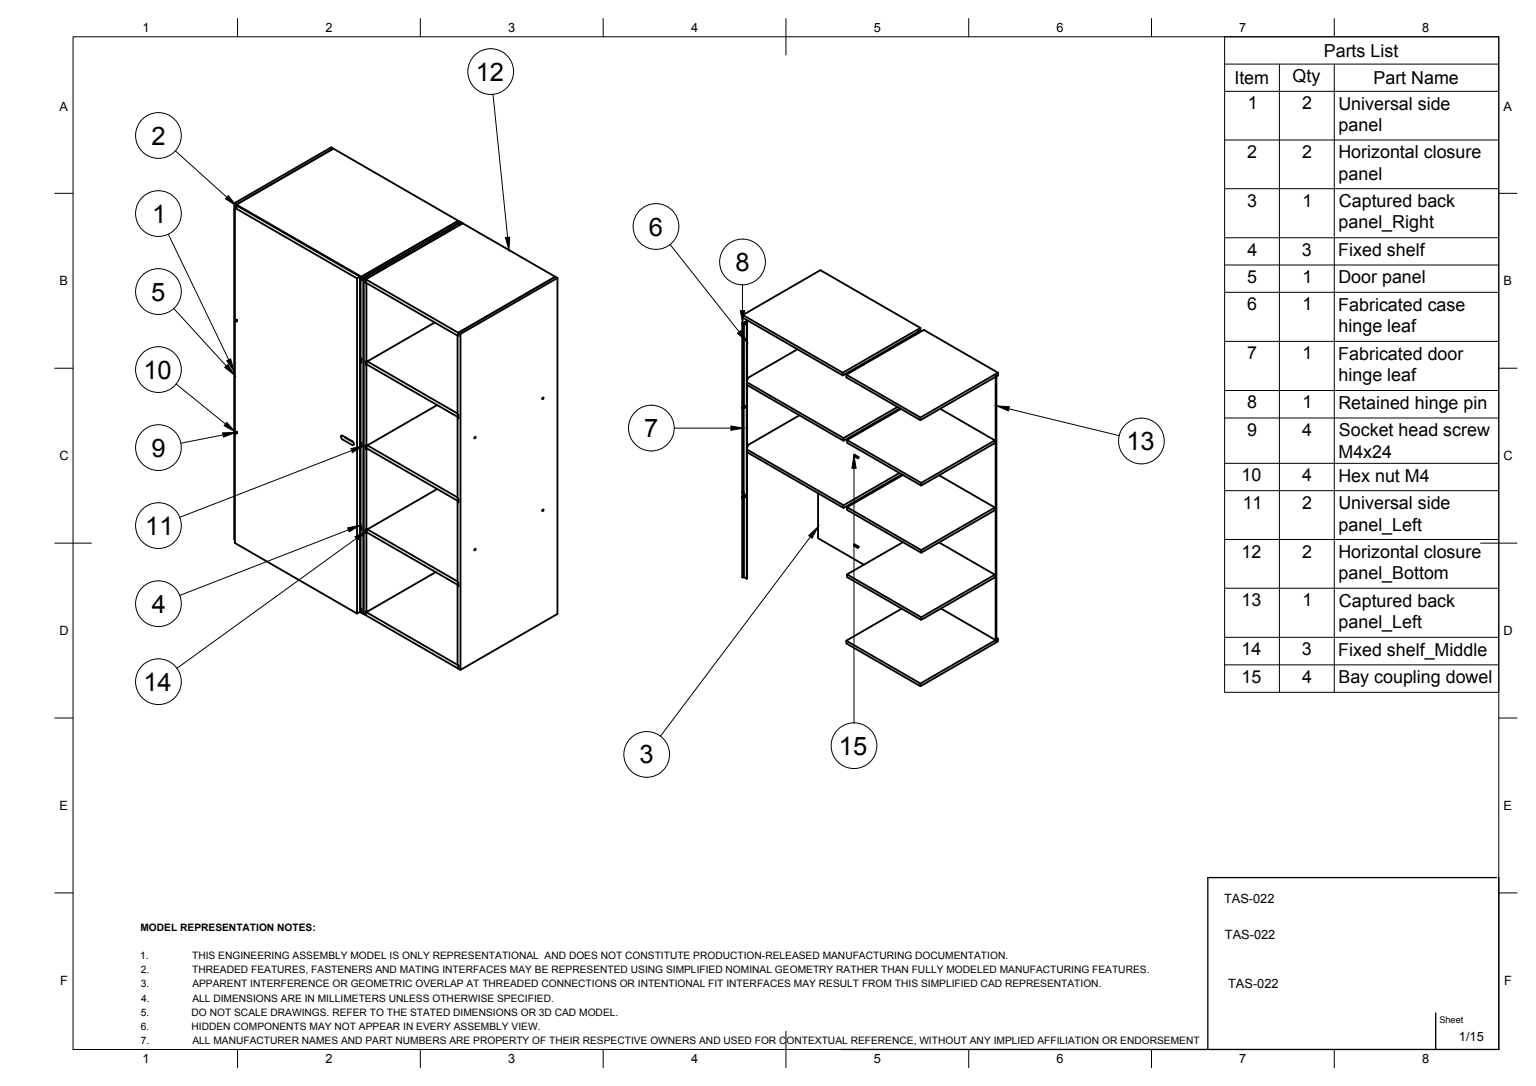
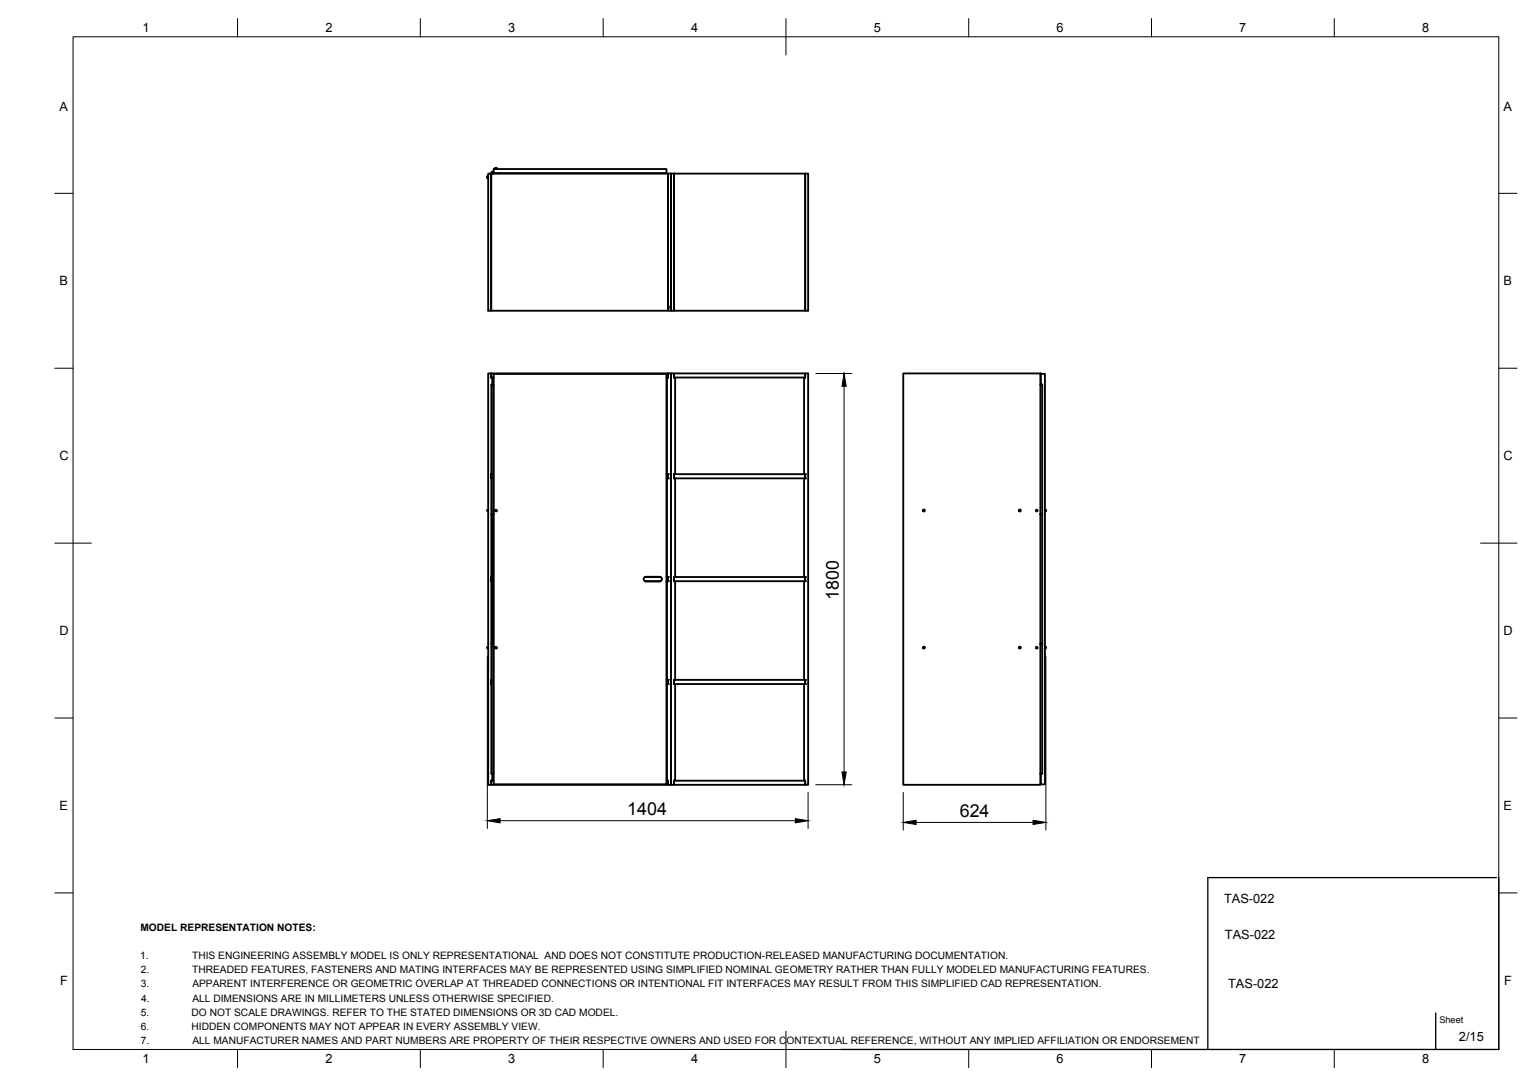
ISO-10303-21;
HEADER;
/* Generated by software containing ST-Developer
 * from STEP Tools, Inc. (www.steptools.com) 
 */

FILE_DESCRIPTION(
/* description */ (''),
/* implementation_level */ '2;1');

FILE_NAME(
/* name */ 'TAS-022.step',
/* time_stamp */ '2026-11-15T21:02:08-08:00',
/* author */ (''),
/* organization */ (''),
/* preprocessor_version */ 'ST-DEVELOPER v20.2',
/* originating_system */ 'Autodesk Translation Framework v15.17.0.0',
/* authorisation */ '');

FILE_SCHEMA (('AUTOMOTIVE_DESIGN { 1 0 10303 214 3 1 1 }'));
ENDSEC;

DATA;
#10=MECHANICAL_DESIGN_GEOMETRIC_PRESENTATION_REPRESENTATION('',(#602,#603,
#604,#605,#606,#607,#608,#609,#610,#611,#612,#613,#614,#615,#616),#31566);
#11=ITEM_DEFINED_TRANSFORMATION($,$,#6008,#6250);
#12=ITEM_DEFINED_TRANSFORMATION($,$,#6069,#6251);
#13=ITEM_DEFINED_TRANSFORMATION($,$,#5897,#6252);
#14=ITEM_DEFINED_TRANSFORMATION($,$,#6080,#6253);
#15=ITEM_DEFINED_TRANSFORMATION($,$,#5904,#6254);
#16=ITEM_DEFINED_TRANSFORMATION($,$,#5925,#6255);
#17=ITEM_DEFINED_TRANSFORMATION($,$,#5958,#6256);
#18=ITEM_DEFINED_TRANSFORMATION($,$,#5987,#6257);
#19=ITEM_DEFINED_TRANSFORMATION($,$,#6089,#6258);
#20=ITEM_DEFINED_TRANSFORMATION($,$,#6143,#6259);
#21=ITEM_DEFINED_TRANSFORMATION($,$,#6171,#6260);
#22=ITEM_DEFINED_TRANSFORMATION($,$,#6226,#6261);
#23=ITEM_DEFINED_TRANSFORMATION($,$,#6001,#6262);
#24=ITEM_DEFINED_TRANSFORMATION($,$,#6237,#6263);
#25=ITEM_DEFINED_TRANSFORMATION($,$,#6244,#6264);
#26=ITEM_DEFINED_TRANSFORMATION($,$,#6008,#6265);
#27=ITEM_DEFINED_TRANSFORMATION($,$,#6069,#6266);
#28=ITEM_DEFINED_TRANSFORMATION($,$,#6080,#6267);
#29=ITEM_DEFINED_TRANSFORMATION($,$,#6080,#6268);
#30=ITEM_DEFINED_TRANSFORMATION($,$,#6089,#6269);
#31=ITEM_DEFINED_TRANSFORMATION($,$,#6143,#6270);
#32=ITEM_DEFINED_TRANSFORMATION($,$,#6089,#6271);
#33=ITEM_DEFINED_TRANSFORMATION($,$,#6143,#6272);
#34=ITEM_DEFINED_TRANSFORMATION($,$,#6089,#6273);
#35=ITEM_DEFINED_TRANSFORMATION($,$,#6143,#6274);
#36=ITEM_DEFINED_TRANSFORMATION($,$,#6171,#6275);
#37=ITEM_DEFINED_TRANSFORMATION($,$,#6226,#6276);
#38=ITEM_DEFINED_TRANSFORMATION($,$,#6237,#6277);
#39=ITEM_DEFINED_TRANSFORMATION($,$,#6237,#6278);
#40=ITEM_DEFINED_TRANSFORMATION($,$,#6244,#6279);
#41=ITEM_DEFINED_TRANSFORMATION($,$,#6244,#6280);
#42=ITEM_DEFINED_TRANSFORMATION($,$,#6244,#6281);
#43=(
REPRESENTATION_RELATIONSHIP($,$,#31642,#31635)
REPRESENTATION_RELATIONSHIP_WITH_TRANSFORMATION(#11)
SHAPE_REPRESENTATION_RELATIONSHIP()
);
#44=(
REPRESENTATION_RELATIONSHIP($,$,#31643,#31635)
REPRESENTATION_RELATIONSHIP_WITH_TRANSFORMATION(#12)
SHAPE_REPRESENTATION_RELATIONSHIP()
);
#45=(
REPRESENTATION_RELATIONSHIP($,$,#31636,#31635)
REPRESENTATION_RELATIONSHIP_WITH_TRANSFORMATION(#13)
SHAPE_REPRESENTATION_RELATIONSHIP()
);
#46=(
REPRESENTATION_RELATIONSHIP($,$,#31644,#31635)
REPRESENTATION_RELATIONSHIP_WITH_TRANSFORMATION(#14)
SHAPE_REPRESENTATION_RELATIONSHIP()
);
#47=(
REPRESENTATION_RELATIONSHIP($,$,#31637,#31635)
REPRESENTATION_RELATIONSHIP_WITH_TRANSFORMATION(#15)
SHAPE_REPRESENTATION_RELATIONSHIP()
);
#48=(
REPRESENTATION_RELATIONSHIP($,$,#31638,#31635)
REPRESENTATION_RELATIONSHIP_WITH_TRANSFORMATION(#16)
SHAPE_REPRESENTATION_RELATIONSHIP()
);
#49=(
REPRESENTATION_RELATIONSHIP($,$,#31639,#31635)
REPRESENTATION_RELATIONSHIP_WITH_TRANSFORMATION(#17)
SHAPE_REPRESENTATION_RELATIONSHIP()
);
#50=(
REPRESENTATION_RELATIONSHIP($,$,#31640,#31635)
REPRESENTATION_RELATIONSHIP_WITH_TRANSFORMATION(#18)
SHAPE_REPRESENTATION_RELATIONSHIP()
);
#51=(
REPRESENTATION_RELATIONSHIP($,$,#31645,#31635)
REPRESENTATION_RELATIONSHIP_WITH_TRANSFORMATION(#19)
SHAPE_REPRESENTATION_RELATIONSHIP()
);
#52=(
REPRESENTATION_RELATIONSHIP($,$,#31646,#31635)
REPRESENTATION_RELATIONSHIP_WITH_TRANSFORMATION(#20)
SHAPE_REPRESENTATION_RELATIONSHIP()
);
#53=(
REPRESENTATION_RELATIONSHIP($,$,#31647,#31635)
REPRESENTATION_RELATIONSHIP_WITH_TRANSFORMATION(#21)
SHAPE_REPRESENTATION_RELATIONSHIP()
);
#54=(
REPRESENTATION_RELATIONSHIP($,$,#31648,#31635)
REPRESENTATION_RELATIONSHIP_WITH_TRANSFORMATION(#22)
SHAPE_REPRESENTATION_RELATIONSHIP()
);
#55=(
REPRESENTATION_RELATIONSHIP($,$,#31641,#31635)
REPRESENTATION_RELATIONSHIP_WITH_TRANSFORMATION(#23)
SHAPE_REPRESENTATION_RELATIONSHIP()
);
#56=(
REPRESENTATION_RELATIONSHIP($,$,#31649,#31635)
REPRESENTATION_RELATIONSHIP_WITH_TRANSFORMATION(#24)
SHAPE_REPRESENTATION_RELATIONSHIP()
);
#57=(
REPRESENTATION_RELATIONSHIP($,$,#31650,#31635)
REPRESENTATION_RELATIONSHIP_WITH_TRANSFORMATION(#25)
SHAPE_REPRESENTATION_RELATIONSHIP()
);
#58=(
REPRESENTATION_RELATIONSHIP($,$,#31642,#31635)
REPRESENTATION_RELATIONSHIP_WITH_TRANSFORMATION(#26)
SHAPE_REPRESENTATION_RELATIONSHIP()
);
#59=(
REPRESENTATION_RELATIONSHIP($,$,#31643,#31635)
REPRESENTATION_RELATIONSHIP_WITH_TRANSFORMATION(#27)
SHAPE_REPRESENTATION_RELATIONSHIP()
);
#60=(
REPRESENTATION_RELATIONSHIP($,$,#31644,#31635)
REPRESENTATION_RELATIONSHIP_WITH_TRANSFORMATION(#28)
SHAPE_REPRESENTATION_RELATIONSHIP()
);
#61=(
REPRESENTATION_RELATIONSHIP($,$,#31644,#31635)
REPRESENTATION_RELATIONSHIP_WITH_TRANSFORMATION(#29)
SHAPE_REPRESENTATION_RELATIONSHIP()
);
#62=(
REPRESENTATION_RELATIONSHIP($,$,#31645,#31635)
REPRESENTATION_RELATIONSHIP_WITH_TRANSFORMATION(#30)
SHAPE_REPRESENTATION_RELATIONSHIP()
);
#63=(
REPRESENTATION_RELATIONSHIP($,$,#31646,#31635)
REPRESENTATION_RELATIONSHIP_WITH_TRANSFORMATION(#31)
SHAPE_REPRESENTATION_RELATIONSHIP()
);
#64=(
REPRESENTATION_RELATIONSHIP($,$,#31645,#31635)
REPRESENTATION_RELATIONSHIP_WITH_TRANSFORMATION(#32)
SHAPE_REPRESENTATION_RELATIONSHIP()
);
#65=(
REPRESENTATION_RELATIONSHIP($,$,#31646,#31635)
REPRESENTATION_RELATIONSHIP_WITH_TRANSFORMATION(#33)
SHAPE_REPRESENTATION_RELATIONSHIP()
);
#66=(
REPRESENTATION_RELATIONSHIP($,$,#31645,#31635)
REPRESENTATION_RELATIONSHIP_WITH_TRANSFORMATION(#34)
SHAPE_REPRESENTATION_RELATIONSHIP()
);
#67=(
REPRESENTATION_RELATIONSHIP($,$,#31646,#31635)
REPRESENTATION_RELATIONSHIP_WITH_TRANSFORMATION(#35)
SHAPE_REPRESENTATION_RELATIONSHIP()
);
#68=(
REPRESENTATION_RELATIONSHIP($,$,#31647,#31635)
REPRESENTATION_RELATIONSHIP_WITH_TRANSFORMATION(#36)
SHAPE_REPRESENTATION_RELATIONSHIP()
);
#69=(
REPRESENTATION_RELATIONSHIP($,$,#31648,#31635)
REPRESENTATION_RELATIONSHIP_WITH_TRANSFORMATION(#37)
SHAPE_REPRESENTATION_RELATIONSHIP()
);
#70=(
REPRESENTATION_RELATIONSHIP($,$,#31649,#31635)
REPRESENTATION_RELATIONSHIP_WITH_TRANSFORMATION(#38)
SHAPE_REPRESENTATION_RELATIONSHIP()
);
#71=(
REPRESENTATION_RELATIONSHIP($,$,#31649,#31635)
REPRESENTATION_RELATIONSHIP_WITH_TRANSFORMATION(#39)
SHAPE_REPRESENTATION_RELATIONSHIP()
);
#72=(
REPRESENTATION_RELATIONSHIP($,$,#31650,#31635)
REPRESENTATION_RELATIONSHIP_WITH_TRANSFORMATION(#40)
SHAPE_REPRESENTATION_RELATIONSHIP()
);
#73=(
REPRESENTATION_RELATIONSHIP($,$,#31650,#31635)
REPRESENTATION_RELATIONSHIP_WITH_TRANSFORMATION(#41)
SHAPE_REPRESENTATION_RELATIONSHIP()
);
#74=(
REPRESENTATION_RELATIONSHIP($,$,#31650,#31635)
REPRESENTATION_RELATIONSHIP_WITH_TRANSFORMATION(#42)
SHAPE_REPRESENTATION_RELATIONSHIP()
);
#75=CONTEXT_DEPENDENT_SHAPE_REPRESENTATION(#43,#31603);
#76=CONTEXT_DEPENDENT_SHAPE_REPRESENTATION(#44,#31604);
#77=CONTEXT_DEPENDENT_SHAPE_REPRESENTATION(#45,#31605);
#78=CONTEXT_DEPENDENT_SHAPE_REPRESENTATION(#46,#31606);
#79=CONTEXT_DEPENDENT_SHAPE_REPRESENTATION(#47,#31607);
#80=CONTEXT_DEPENDENT_SHAPE_REPRESENTATION(#48,#31608);
#81=CONTEXT_DEPENDENT_SHAPE_REPRESENTATION(#49,#31609);
#82=CONTEXT_DEPENDENT_SHAPE_REPRESENTATION(#50,#31610);
#83=CONTEXT_DEPENDENT_SHAPE_REPRESENTATION(#51,#31611);
#84=CONTEXT_DEPENDENT_SHAPE_REPRESENTATION(#52,#31612);
#85=CONTEXT_DEPENDENT_SHAPE_REPRESENTATION(#53,#31613);
#86=CONTEXT_DEPENDENT_SHAPE_REPRESENTATION(#54,#31614);
#87=CONTEXT_DEPENDENT_SHAPE_REPRESENTATION(#55,#31615);
#88=CONTEXT_DEPENDENT_SHAPE_REPRESENTATION(#56,#31616);
#89=CONTEXT_DEPENDENT_SHAPE_REPRESENTATION(#57,#31617);
#90=CONTEXT_DEPENDENT_SHAPE_REPRESENTATION(#58,#31618);
#91=CONTEXT_DEPENDENT_SHAPE_REPRESENTATION(#59,#31619);
#92=CONTEXT_DEPENDENT_SHAPE_REPRESENTATION(#60,#31620);
#93=CONTEXT_DEPENDENT_SHAPE_REPRESENTATION(#61,#31621);
#94=CONTEXT_DEPENDENT_SHAPE_REPRESENTATION(#62,#31622);
#95=CONTEXT_DEPENDENT_SHAPE_REPRESENTATION(#63,#31623);
#96=CONTEXT_DEPENDENT_SHAPE_REPRESENTATION(#64,#31624);
#97=CONTEXT_DEPENDENT_SHAPE_REPRESENTATION(#65,#31625);
#98=CONTEXT_DEPENDENT_SHAPE_REPRESENTATION(#66,#31626);
#99=CONTEXT_DEPENDENT_SHAPE_REPRESENTATION(#67,#31627);
#100=CONTEXT_DEPENDENT_SHAPE_REPRESENTATION(#68,#31628);
#101=CONTEXT_DEPENDENT_SHAPE_REPRESENTATION(#69,#31629);
#102=CONTEXT_DEPENDENT_SHAPE_REPRESENTATION(#70,#31630);
#103=CONTEXT_DEPENDENT_SHAPE_REPRESENTATION(#71,#31631);
#104=CONTEXT_DEPENDENT_SHAPE_REPRESENTATION(#72,#31632);
#105=CONTEXT_DEPENDENT_SHAPE_REPRESENTATION(#73,#31633);
#106=CONTEXT_DEPENDENT_SHAPE_REPRESENTATION(#74,#31634);
#107=NEXT_ASSEMBLY_USAGE_OCCURRENCE('Universal side panel:1',
'Universal side panel:1','Universal side panel:1',#31652,#31659,
'Universal side panel:1');
#108=NEXT_ASSEMBLY_USAGE_OCCURRENCE('Horizontal closure panel:1',
'Horizontal closure panel:1','Horizontal closure panel:1',#31652,#31660,
'Horizontal closure panel:1');
#109=NEXT_ASSEMBLY_USAGE_OCCURRENCE('Captured back panel_Right:1',
'Captured back panel_Right:1','Captured back panel_Right:1',#31652,#31653,
'Captured back panel_Right:1');
#110=NEXT_ASSEMBLY_USAGE_OCCURRENCE('Fixed shelf:1','Fixed shelf:1',
'Fixed shelf:1',#31652,#31661,'Fixed shelf:1');
#111=NEXT_ASSEMBLY_USAGE_OCCURRENCE('Door panel:1','Door panel:1',
'Door panel:1',#31652,#31654,'Door panel:1');
#112=NEXT_ASSEMBLY_USAGE_OCCURRENCE('Fabricated case hinge leaf:1',
'Fabricated case hinge leaf:1','Fabricated case hinge leaf:1',#31652,#31655,
'Fabricated case hinge leaf:1');
#113=NEXT_ASSEMBLY_USAGE_OCCURRENCE('Fabricated door hinge leaf:1',
'Fabricated door hinge leaf:1','Fabricated door hinge leaf:1',#31652,#31656,
'Fabricated door hinge leaf:1');
#114=NEXT_ASSEMBLY_USAGE_OCCURRENCE('Retained hinge pin:1',
'Retained hinge pin:1','Retained hinge pin:1',#31652,#31657,
'Retained hinge pin:1');
#115=NEXT_ASSEMBLY_USAGE_OCCURRENCE('Socket head screw M4x24:1',
'Socket head screw M4x24:1','Socket head screw M4x24:1',#31652,#31662,
'Socket head screw M4x24:1');
#116=NEXT_ASSEMBLY_USAGE_OCCURRENCE('Hex nut M4:1','Hex nut M4:1',
'Hex nut M4:1',#31652,#31663,'Hex nut M4:1');
#117=NEXT_ASSEMBLY_USAGE_OCCURRENCE('Universal side panel_Left:1',
'Universal side panel_Left:1','Universal side panel_Left:1',#31652,#31664,
'Universal side panel_Left:1');
#118=NEXT_ASSEMBLY_USAGE_OCCURRENCE('Horizontal closure panel_Bottom:1',
'Horizontal closure panel_Bottom:1','Horizontal closure panel_Bottom:1',
#31652,#31665,'Horizontal closure panel_Bottom:1');
#119=NEXT_ASSEMBLY_USAGE_OCCURRENCE('Captured back panel_Left:1',
'Captured back panel_Left:1','Captured back panel_Left:1',#31652,#31658,
'Captured back panel_Left:1');
#120=NEXT_ASSEMBLY_USAGE_OCCURRENCE('Fixed shelf_Middle:1',
'Fixed shelf_Middle:1','Fixed shelf_Middle:1',#31652,#31666,
'Fixed shelf_Middle:1');
#121=NEXT_ASSEMBLY_USAGE_OCCURRENCE('Bay coupling dowel:1',
'Bay coupling dowel:1','Bay coupling dowel:1',#31652,#31667,
'Bay coupling dowel:1');
#122=NEXT_ASSEMBLY_USAGE_OCCURRENCE('Universal side panel:2',
'Universal side panel:2','Universal side panel:2',#31652,#31659,
'Universal side panel:2');
#123=NEXT_ASSEMBLY_USAGE_OCCURRENCE('Horizontal closure panel:2',
'Horizontal closure panel:2','Horizontal closure panel:2',#31652,#31660,
'Horizontal closure panel:2');
#124=NEXT_ASSEMBLY_USAGE_OCCURRENCE('Fixed shelf:2','Fixed shelf:2',
'Fixed shelf:2',#31652,#31661,'Fixed shelf:2');
#125=NEXT_ASSEMBLY_USAGE_OCCURRENCE('Fixed shelf:3','Fixed shelf:3',
'Fixed shelf:3',#31652,#31661,'Fixed shelf:3');
#126=NEXT_ASSEMBLY_USAGE_OCCURRENCE('Socket head screw M4x24:2',
'Socket head screw M4x24:2','Socket head screw M4x24:2',#31652,#31662,
'Socket head screw M4x24:2');
#127=NEXT_ASSEMBLY_USAGE_OCCURRENCE('Hex nut M4:2','Hex nut M4:2',
'Hex nut M4:2',#31652,#31663,'Hex nut M4:2');
#128=NEXT_ASSEMBLY_USAGE_OCCURRENCE('Socket head screw M4x24:3',
'Socket head screw M4x24:3','Socket head screw M4x24:3',#31652,#31662,
'Socket head screw M4x24:3');
#129=NEXT_ASSEMBLY_USAGE_OCCURRENCE('Hex nut M4:3','Hex nut M4:3',
'Hex nut M4:3',#31652,#31663,'Hex nut M4:3');
#130=NEXT_ASSEMBLY_USAGE_OCCURRENCE('Socket head screw M4x24:4',
'Socket head screw M4x24:4','Socket head screw M4x24:4',#31652,#31662,
'Socket head screw M4x24:4');
#131=NEXT_ASSEMBLY_USAGE_OCCURRENCE('Hex nut M4:4','Hex nut M4:4',
'Hex nut M4:4',#31652,#31663,'Hex nut M4:4');
#132=NEXT_ASSEMBLY_USAGE_OCCURRENCE('Universal side panel_Left:2',
'Universal side panel_Left:2','Universal side panel_Left:2',#31652,#31664,
'Universal side panel_Left:2');
#133=NEXT_ASSEMBLY_USAGE_OCCURRENCE('Horizontal closure panel_Bottom:2',
'Horizontal closure panel_Bottom:2','Horizontal closure panel_Bottom:2',
#31652,#31665,'Horizontal closure panel_Bottom:2');
#134=NEXT_ASSEMBLY_USAGE_OCCURRENCE('Fixed shelf_Middle:2',
'Fixed shelf_Middle:2','Fixed shelf_Middle:2',#31652,#31666,
'Fixed shelf_Middle:2');
#135=NEXT_ASSEMBLY_USAGE_OCCURRENCE('Fixed shelf_Middle:3',
'Fixed shelf_Middle:3','Fixed shelf_Middle:3',#31652,#31666,
'Fixed shelf_Middle:3');
#136=NEXT_ASSEMBLY_USAGE_OCCURRENCE('Bay coupling dowel:2',
'Bay coupling dowel:2','Bay coupling dowel:2',#31652,#31667,
'Bay coupling dowel:2');
#137=NEXT_ASSEMBLY_USAGE_OCCURRENCE('Bay coupling dowel:3',
'Bay coupling dowel:3','Bay coupling dowel:3',#31652,#31667,
'Bay coupling dowel:3');
#138=NEXT_ASSEMBLY_USAGE_OCCURRENCE('Bay coupling dowel:4',
'Bay coupling dowel:4','Bay coupling dowel:4',#31652,#31667,
'Bay coupling dowel:4');
#139=B_SPLINE_SURFACE_WITH_KNOTS('',3,3,((#26552,#26553,#26554,#26555,#26556,
#26557,#26558,#26559,#26560,#26561,#26562,#26563,#26564,#26565,#26566,#26567,
#26568,#26569,#26570,#26571,#26572,#26573,#26574,#26575,#26576,#26577,#26578,
#26579,#26580,#26581,#26582,#26583,#26584,#26585,#26586,#26587,#26588,#26589,
#26590,#26591,#26592,#26593,#26594,#26595,#26596,#26597,#26598,#26599,#26600,
#26601,#26602,#26603,#26604,#26605,#26606,#26607,#26608,#26609,#26610,#26611,
#26612,#26613,#26614,#26615,#26616,#26617,#26618,#26619,#26620,#26621,#26622,
#26623,#26624,#26625,#26626,#26627,#26628,#26629,#26630,#26631,#26632,#26633,
#26634,#26635,#26636,#26637,#26638,#26639,#26640,#26641,#26642,#26643,#26644,
#26645,#26646,#26647,#26648,#26649,#26650,#26651,#26652,#26653,#26654,#26655,
#26656,#26657,#26658,#26659,#26660,#26661,#26662,#26663,#26664,#26665,#26666,
#26667,#26668,#26669,#26670,#26671,#26672,#26673,#26674,#26675,#26676,#26677,
#26678,#26679,#26680,#26681,#26682,#26683,#26684,#26685,#26686,#26687,#26688,
#26689,#26690,#26691,#26692,#26693,#26694,#26695,#26696,#26697,#26698,#26699,
#26700,#26701,#26702,#26703,#26704,#26705,#26706,#26707,#26708,#26709,#26710,
#26711,#26712,#26713,#26714,#26715,#26716,#26717,#26718,#26719,#26720,#26721,
#26722,#26723,#26724,#26725,#26726,#26727,#26728,#26729,#26730,#26731,#26732,
#26733,#26734,#26735,#26736,#26737,#26738,#26739,#26740,#26741,#26742,#26743,
#26744,#26745,#26746,#26747,#26748,#26749,#26750,#26751,#26752,#26753,#26754,
#26755,#26756,#26757,#26758,#26759,#26760,#26761,#26762,#26763,#26764,#26765,
#26766,#26767,#26768,#26769,#26770,#26771,#26772),(#26773,#26774,#26775,
#26776,#26777,#26778,#26779,#26780,#26781,#26782,#26783,#26784,#26785,#26786,
#26787,#26788,#26789,#26790,#26791,#26792,#26793,#26794,#26795,#26796,#26797,
#26798,#26799,#26800,#26801,#26802,#26803,#26804,#26805,#26806,#26807,#26808,
#26809,#26810,#26811,#26812,#26813,#26814,#26815,#26816,#26817,#26818,#26819,
#26820,#26821,#26822,#26823,#26824,#26825,#26826,#26827,#26828,#26829,#26830,
#26831,#26832,#26833,#26834,#26835,#26836,#26837,#26838,#26839,#26840,#26841,
#26842,#26843,#26844,#26845,#26846,#26847,#26848,#26849,#26850,#26851,#26852,
#26853,#26854,#26855,#26856,#26857,#26858,#26859,#26860,#26861,#26862,#26863,
#26864,#26865,#26866,#26867,#26868,#26869,#26870,#26871,#26872,#26873,#26874,
#26875,#26876,#26877,#26878,#26879,#26880,#26881,#26882,#26883,#26884,#26885,
#26886,#26887,#26888,#26889,#26890,#26891,#26892,#26893,#26894,#26895,#26896,
#26897,#26898,#26899,#26900,#26901,#26902,#26903,#26904,#26905,#26906,#26907,
#26908,#26909,#26910,#26911,#26912,#26913,#26914,#26915,#26916,#26917,#26918,
#26919,#26920,#26921,#26922,#26923,#26924,#26925,#26926,#26927,#26928,#26929,
#26930,#26931,#26932,#26933,#26934,#26935,#26936,#26937,#26938,#26939,#26940,
#26941,#26942,#26943,#26944,#26945,#26946,#26947,#26948,#26949,#26950,#26951,
#26952,#26953,#26954,#26955,#26956,#26957,#26958,#26959,#26960,#26961,#26962,
#26963,#26964,#26965,#26966,#26967,#26968,#26969,#26970,#26971,#26972,#26973,
#26974,#26975,#26976,#26977,#26978,#26979,#26980,#26981,#26982,#26983,#26984,
#26985,#26986,#26987,#26988,#26989,#26990,#26991,#26992,#26993),(#26994,
#26995,#26996,#26997,#26998,#26999,#27000,#27001,#27002,#27003,#27004,#27005,
#27006,#27007,#27008,#27009,#27010,#27011,#27012,#27013,#27014,#27015,#27016,
#27017,#27018,#27019,#27020,#27021,#27022,#27023,#27024,#27025,#27026,#27027,
#27028,#27029,#27030,#27031,#27032,#27033,#27034,#27035,#27036,#27037,#27038,
#27039,#27040,#27041,#27042,#27043,#27044,#27045,#27046,#27047,#27048,#27049,
#27050,#27051,#27052,#27053,#27054,#27055,#27056,#27057,#27058,#27059,#27060,
#27061,#27062,#27063,#27064,#27065,#27066,#27067,#27068,#27069,#27070,#27071,
#27072,#27073,#27074,#27075,#27076,#27077,#27078,#27079,#27080,#27081,#27082,
#27083,#27084,#27085,#27086,#27087,#27088,#27089,#27090,#27091,#27092,#27093,
#27094,#27095,#27096,#27097,#27098,#27099,#27100,#27101,#27102,#27103,#27104,
#27105,#27106,#27107,#27108,#27109,#27110,#27111,#27112,#27113,#27114,#27115,
#27116,#27117,#27118,#27119,#27120,#27121,#27122,#27123,#27124,#27125,#27126,
#27127,#27128,#27129,#27130,#27131,#27132,#27133,#27134,#27135,#27136,#27137,
#27138,#27139,#27140,#27141,#27142,#27143,#27144,#27145,#27146,#27147,#27148,
#27149,#27150,#27151,#27152,#27153,#27154,#27155,#27156,#27157,#27158,#27159,
#27160,#27161,#27162,#27163,#27164,#27165,#27166,#27167,#27168,#27169,#27170,
#27171,#27172,#27173,#27174,#27175,#27176,#27177,#27178,#27179,#27180,#27181,
#27182,#27183,#27184,#27185,#27186,#27187,#27188,#27189,#27190,#27191,#27192,
#27193,#27194,#27195,#27196,#27197,#27198,#27199,#27200,#27201,#27202,#27203,
#27204,#27205,#27206,#27207,#27208,#27209,#27210,#27211,#27212,#27213,#27214),
(#27215,#27216,#27217,#27218,#27219,#27220,#27221,#27222,#27223,#27224,
#27225,#27226,#27227,#27228,#27229,#27230,#27231,#27232,#27233,#27234,#27235,
#27236,#27237,#27238,#27239,#27240,#27241,#27242,#27243,#27244,#27245,#27246,
#27247,#27248,#27249,#27250,#27251,#27252,#27253,#27254,#27255,#27256,#27257,
#27258,#27259,#27260,#27261,#27262,#27263,#27264,#27265,#27266,#27267,#27268,
#27269,#27270,#27271,#27272,#27273,#27274,#27275,#27276,#27277,#27278,#27279,
#27280,#27281,#27282,#27283,#27284,#27285,#27286,#27287,#27288,#27289,#27290,
#27291,#27292,#27293,#27294,#27295,#27296,#27297,#27298,#27299,#27300,#27301,
#27302,#27303,#27304,#27305,#27306,#27307,#27308,#27309,#27310,#27311,#27312,
#27313,#27314,#27315,#27316,#27317,#27318,#27319,#27320,#27321,#27322,#27323,
#27324,#27325,#27326,#27327,#27328,#27329,#27330,#27331,#27332,#27333,#27334,
#27335,#27336,#27337,#27338,#27339,#27340,#27341,#27342,#27343,#27344,#27345,
#27346,#27347,#27348,#27349,#27350,#27351,#27352,#27353,#27354,#27355,#27356,
#27357,#27358,#27359,#27360,#27361,#27362,#27363,#27364,#27365,#27366,#27367,
#27368,#27369,#27370,#27371,#27372,#27373,#27374,#27375,#27376,#27377,#27378,
#27379,#27380,#27381,#27382,#27383,#27384,#27385,#27386,#27387,#27388,#27389,
#27390,#27391,#27392,#27393,#27394,#27395,#27396,#27397,#27398,#27399,#27400,
#27401,#27402,#27403,#27404,#27405,#27406,#27407,#27408,#27409,#27410,#27411,
#27412,#27413,#27414,#27415,#27416,#27417,#27418,#27419,#27420,#27421,#27422,
#27423,#27424,#27425,#27426,#27427,#27428,#27429,#27430,#27431,#27432,#27433,
#27434,#27435)),.UNSPECIFIED.,.F.,.F.,.F.,(4,4),(4,1,1,1,1,1,1,1,1,1,1,
1,1,1,1,1,1,1,1,1,1,1,1,1,1,1,1,1,1,1,1,1,1,1,1,1,1,1,1,1,1,1,1,1,1,1,1,
1,1,1,1,1,1,1,1,1,1,1,1,1,1,1,1,1,1,1,1,1,1,1,1,1,1,1,1,1,1,1,1,1,1,1,1,
1,1,1,1,1,1,1,1,1,1,1,1,1,1,1,1,1,1,1,1,1,1,1,1,1,1,1,1,1,1,1,1,1,1,1,1,
1,1,1,1,1,1,1,1,1,1,1,1,1,1,1,1,1,1,1,1,1,1,1,1,1,1,1,1,1,1,1,1,1,1,1,1,
1,1,1,1,1,1,1,1,1,1,1,1,1,1,1,1,1,1,1,1,1,1,1,1,1,1,1,1,1,1,1,1,1,1,1,1,
1,1,1,1,1,1,1,1,1,1,1,1,1,1,1,1,1,1,1,1,1,1,1,1,1,1,1,4),(-0.000319813591940947,
0.0463078634348368),(8.31044143726206,9.30824121805847,10.305895513377,
11.3035498086955,12.301204104014,13.2988583993325,14.296512694651,15.2941669899695,
16.291821285288,17.2894755806066,18.2871298759251,19.2847841712436,20.2824384665621,
21.2800927618806,22.2777470571991,23.2754013525176,24.2730556478361,25.2707099431546,
26.2683642384732,27.2660185337917,28.2636728291102,29.2613271244287,30.2589814197472,
31.2566357150657,32.2542900103842,33.2519443057027,34.2495986010213,35.2472528963398,
36.2449071916583,37.2425614869768,38.2402157822953,39.2378700776138,40.2355243729323,
41.2331786682508,42.2308329635693,43.2284872588879,44.2261415542064,45.2237958495249,
46.2214501448434,47.2191044401619,48.2167587354804,49.2144130307989,50.2120673261174,
51.209721621436,52.2073759167545,53.205030212073,54.2026845073915,55.20033880271,
56.1979930980285,57.195647393347,58.1933016886655,59.190955983984,60.1886102793026,
61.1862645746211,62.1839188699396,63.1815731652581,64.1792274605766,65.1768817558951,
66.1745360512136,67.1721903465321,68.1698446418506,69.1674989371692,70.1651532324877,
71.1628075278062,72.1604618231247,73.1581161184432,74.1557704137617,75.1534247090802,
76.1510790043987,77.1487332997173,78.1463875950358,79.1440418903543,80.1416961856728,
81.1393504809913,82.1370047763098,83.1346590716283,84.1323133669468,85.1299676622653,
86.1276219575839,87.1252762529024,88.1229305482209,89.1205848435394,90.1182391388579,
91.1158934341764,92.1135477294949,93.1112020248134,94.1088563201319,95.1065106154505,
96.104164910769,97.1018192060875,98.099473501406,99.0971277967245,100.094782092043,
101.092436387362,102.09009068268,103.087744977999,104.085399273317,105.083053568636,
106.080707863954,107.078362159273,108.076016454591,109.07367074991,110.071325045228,
111.068979340547,112.066633635865,113.064287931184,114.061942226502,115.059596521821,
116.057250817139,117.054905112458,118.052559407776,119.050213703095,120.047867998413,
121.045522293732,122.04317658905,123.040830884369,124.038485179687,125.036139475006,
126.033793770324,127.031448065643,128.029102360961,129.02675665628,130.024410951598,
131.022065246917,132.019719542235,133.017373837554,134.015028132872,135.012682428191,
136.010336723509,137.007991018828,138.005645314146,139.003299609465,140.000953904783,
140.998608200102,141.99626249542,142.993916790739,143.991571086058,144.989225381376,
145.986879676695,146.984533972013,147.982188267332,148.97984256265,149.977496857969,
150.975151153287,151.972805448606,152.970459743924,153.968114039243,154.965768334561,
155.96342262988,156.961076925198,157.958731220517,158.956385515835,159.954039811154,
160.951694106472,161.949348401791,162.947002697109,163.944656992428,164.942311287746,
165.939965583065,166.937619878383,167.935274173702,168.93292846902,169.930582764339,
170.928237059657,171.925891354976,172.923545650294,173.921199945613,174.918854240931,
175.91650853625,176.914162831568,177.911817126887,178.909471422205,179.907125717524,
180.904780012842,181.902434308161,182.900088603479,183.897742898798,184.895397194116,
185.893051489435,186.890705784754,187.888360080072,188.886014375391,189.883668670709,
190.881322966028,191.878977261346,192.876631556665,193.874285851983,194.871940147302,
195.86959444262,196.867248737939,197.864903033257,198.862557328576,199.860211623894,
200.857865919213,201.855520214531,202.85317450985,203.850828805168,204.848483100487,
205.846137395805,206.843791691124,207.841445986442,208.839100281761,209.836754577079,
210.834408872398,211.832063167716,212.829717463035,213.827371758353,214.825026053672,
215.82268034899,216.820334644309,217.817988939627,218.815643234946,219.813297530264,
220.810951825583,221.808606120901,222.80626041622,223.803914711538,224.801569006857,
225.799543115767),.UNSPECIFIED.);
#140=B_SPLINE_SURFACE_WITH_KNOTS('',3,3,((#27548,#27549,#27550,#27551,#27552,
#27553,#27554,#27555,#27556,#27557,#27558,#27559,#27560,#27561,#27562,#27563,
#27564,#27565,#27566,#27567,#27568,#27569,#27570,#27571,#27572,#27573,#27574,
#27575,#27576,#27577,#27578,#27579,#27580,#27581,#27582,#27583,#27584,#27585,
#27586,#27587,#27588,#27589,#27590,#27591,#27592,#27593,#27594,#27595,#27596,
#27597,#27598,#27599,#27600,#27601,#27602,#27603,#27604,#27605,#27606,#27607,
#27608,#27609,#27610,#27611,#27612,#27613,#27614,#27615,#27616,#27617,#27618,
#27619,#27620,#27621,#27622,#27623,#27624,#27625,#27626,#27627,#27628,#27629,
#27630,#27631,#27632,#27633,#27634,#27635,#27636,#27637,#27638,#27639,#27640,
#27641,#27642,#27643,#27644,#27645,#27646,#27647,#27648,#27649,#27650,#27651,
#27652,#27653,#27654,#27655,#27656,#27657,#27658,#27659,#27660,#27661,#27662,
#27663,#27664,#27665,#27666,#27667,#27668,#27669,#27670,#27671,#27672,#27673,
#27674,#27675,#27676,#27677,#27678,#27679,#27680,#27681,#27682,#27683,#27684,
#27685,#27686,#27687,#27688,#27689,#27690,#27691,#27692,#27693,#27694,#27695,
#27696,#27697,#27698,#27699,#27700,#27701,#27702,#27703,#27704,#27705,#27706,
#27707,#27708,#27709,#27710,#27711,#27712,#27713,#27714,#27715,#27716,#27717,
#27718,#27719,#27720,#27721,#27722,#27723,#27724,#27725,#27726,#27727,#27728,
#27729,#27730,#27731,#27732,#27733,#27734,#27735,#27736,#27737,#27738,#27739,
#27740,#27741,#27742,#27743,#27744,#27745,#27746,#27747,#27748,#27749,#27750,
#27751,#27752,#27753,#27754,#27755,#27756,#27757,#27758,#27759,#27760,#27761,
#27762,#27763,#27764,#27765,#27766,#27767,#27768),(#27769,#27770,#27771,
#27772,#27773,#27774,#27775,#27776,#27777,#27778,#27779,#27780,#27781,#27782,
#27783,#27784,#27785,#27786,#27787,#27788,#27789,#27790,#27791,#27792,#27793,
#27794,#27795,#27796,#27797,#27798,#27799,#27800,#27801,#27802,#27803,#27804,
#27805,#27806,#27807,#27808,#27809,#27810,#27811,#27812,#27813,#27814,#27815,
#27816,#27817,#27818,#27819,#27820,#27821,#27822,#27823,#27824,#27825,#27826,
#27827,#27828,#27829,#27830,#27831,#27832,#27833,#27834,#27835,#27836,#27837,
#27838,#27839,#27840,#27841,#27842,#27843,#27844,#27845,#27846,#27847,#27848,
#27849,#27850,#27851,#27852,#27853,#27854,#27855,#27856,#27857,#27858,#27859,
#27860,#27861,#27862,#27863,#27864,#27865,#27866,#27867,#27868,#27869,#27870,
#27871,#27872,#27873,#27874,#27875,#27876,#27877,#27878,#27879,#27880,#27881,
#27882,#27883,#27884,#27885,#27886,#27887,#27888,#27889,#27890,#27891,#27892,
#27893,#27894,#27895,#27896,#27897,#27898,#27899,#27900,#27901,#27902,#27903,
#27904,#27905,#27906,#27907,#27908,#27909,#27910,#27911,#27912,#27913,#27914,
#27915,#27916,#27917,#27918,#27919,#27920,#27921,#27922,#27923,#27924,#27925,
#27926,#27927,#27928,#27929,#27930,#27931,#27932,#27933,#27934,#27935,#27936,
#27937,#27938,#27939,#27940,#27941,#27942,#27943,#27944,#27945,#27946,#27947,
#27948,#27949,#27950,#27951,#27952,#27953,#27954,#27955,#27956,#27957,#27958,
#27959,#27960,#27961,#27962,#27963,#27964,#27965,#27966,#27967,#27968,#27969,
#27970,#27971,#27972,#27973,#27974,#27975,#27976,#27977,#27978,#27979,#27980,
#27981,#27982,#27983,#27984,#27985,#27986,#27987,#27988,#27989),(#27990,
#27991,#27992,#27993,#27994,#27995,#27996,#27997,#27998,#27999,#28000,#28001,
#28002,#28003,#28004,#28005,#28006,#28007,#28008,#28009,#28010,#28011,#28012,
#28013,#28014,#28015,#28016,#28017,#28018,#28019,#28020,#28021,#28022,#28023,
#28024,#28025,#28026,#28027,#28028,#28029,#28030,#28031,#28032,#28033,#28034,
#28035,#28036,#28037,#28038,#28039,#28040,#28041,#28042,#28043,#28044,#28045,
#28046,#28047,#28048,#28049,#28050,#28051,#28052,#28053,#28054,#28055,#28056,
#28057,#28058,#28059,#28060,#28061,#28062,#28063,#28064,#28065,#28066,#28067,
#28068,#28069,#28070,#28071,#28072,#28073,#28074,#28075,#28076,#28077,#28078,
#28079,#28080,#28081,#28082,#28083,#28084,#28085,#28086,#28087,#28088,#28089,
#28090,#28091,#28092,#28093,#28094,#28095,#28096,#28097,#28098,#28099,#28100,
#28101,#28102,#28103,#28104,#28105,#28106,#28107,#28108,#28109,#28110,#28111,
#28112,#28113,#28114,#28115,#28116,#28117,#28118,#28119,#28120,#28121,#28122,
#28123,#28124,#28125,#28126,#28127,#28128,#28129,#28130,#28131,#28132,#28133,
#28134,#28135,#28136,#28137,#28138,#28139,#28140,#28141,#28142,#28143,#28144,
#28145,#28146,#28147,#28148,#28149,#28150,#28151,#28152,#28153,#28154,#28155,
#28156,#28157,#28158,#28159,#28160,#28161,#28162,#28163,#28164,#28165,#28166,
#28167,#28168,#28169,#28170,#28171,#28172,#28173,#28174,#28175,#28176,#28177,
#28178,#28179,#28180,#28181,#28182,#28183,#28184,#28185,#28186,#28187,#28188,
#28189,#28190,#28191,#28192,#28193,#28194,#28195,#28196,#28197,#28198,#28199,
#28200,#28201,#28202,#28203,#28204,#28205,#28206,#28207,#28208,#28209,#28210),
(#28211,#28212,#28213,#28214,#28215,#28216,#28217,#28218,#28219,#28220,
#28221,#28222,#28223,#28224,#28225,#28226,#28227,#28228,#28229,#28230,#28231,
#28232,#28233,#28234,#28235,#28236,#28237,#28238,#28239,#28240,#28241,#28242,
#28243,#28244,#28245,#28246,#28247,#28248,#28249,#28250,#28251,#28252,#28253,
#28254,#28255,#28256,#28257,#28258,#28259,#28260,#28261,#28262,#28263,#28264,
#28265,#28266,#28267,#28268,#28269,#28270,#28271,#28272,#28273,#28274,#28275,
#28276,#28277,#28278,#28279,#28280,#28281,#28282,#28283,#28284,#28285,#28286,
#28287,#28288,#28289,#28290,#28291,#28292,#28293,#28294,#28295,#28296,#28297,
#28298,#28299,#28300,#28301,#28302,#28303,#28304,#28305,#28306,#28307,#28308,
#28309,#28310,#28311,#28312,#28313,#28314,#28315,#28316,#28317,#28318,#28319,
#28320,#28321,#28322,#28323,#28324,#28325,#28326,#28327,#28328,#28329,#28330,
#28331,#28332,#28333,#28334,#28335,#28336,#28337,#28338,#28339,#28340,#28341,
#28342,#28343,#28344,#28345,#28346,#28347,#28348,#28349,#28350,#28351,#28352,
#28353,#28354,#28355,#28356,#28357,#28358,#28359,#28360,#28361,#28362,#28363,
#28364,#28365,#28366,#28367,#28368,#28369,#28370,#28371,#28372,#28373,#28374,
#28375,#28376,#28377,#28378,#28379,#28380,#28381,#28382,#28383,#28384,#28385,
#28386,#28387,#28388,#28389,#28390,#28391,#28392,#28393,#28394,#28395,#28396,
#28397,#28398,#28399,#28400,#28401,#28402,#28403,#28404,#28405,#28406,#28407,
#28408,#28409,#28410,#28411,#28412,#28413,#28414,#28415,#28416,#28417,#28418,
#28419,#28420,#28421,#28422,#28423,#28424,#28425,#28426,#28427,#28428,#28429,
#28430,#28431)),.UNSPECIFIED.,.F.,.F.,.F.,(4,4),(4,1,1,1,1,1,1,1,1,1,1,
1,1,1,1,1,1,1,1,1,1,1,1,1,1,1,1,1,1,1,1,1,1,1,1,1,1,1,1,1,1,1,1,1,1,1,1,
1,1,1,1,1,1,1,1,1,1,1,1,1,1,1,1,1,1,1,1,1,1,1,1,1,1,1,1,1,1,1,1,1,1,1,1,
1,1,1,1,1,1,1,1,1,1,1,1,1,1,1,1,1,1,1,1,1,1,1,1,1,1,1,1,1,1,1,1,1,1,1,1,
1,1,1,1,1,1,1,1,1,1,1,1,1,1,1,1,1,1,1,1,1,1,1,1,1,1,1,1,1,1,1,1,1,1,1,1,
1,1,1,1,1,1,1,1,1,1,1,1,1,1,1,1,1,1,1,1,1,1,1,1,1,1,1,1,1,1,1,1,1,1,1,1,
1,1,1,1,1,1,1,1,1,1,1,1,1,1,1,1,1,1,1,1,1,1,1,1,1,1,1,4),(-0.000277866170942688,
0.0463346228827458),(11.6151017126826,12.6130758144294,13.6107301097479,
14.6083844050664,15.6060387003849,16.6036929957034,17.601347291022,18.5990015863405,
19.596655881659,20.5943101769775,21.591964472296,22.5896187676145,23.587273062933,
24.5849273582515,25.58258165357,26.5802359488886,27.5778902442071,28.5755445395256,
29.5731988348441,30.5708531301626,31.5685074254811,32.5661617207996,33.5638160161181,
34.5614703114366,35.5591246067551,36.5567789020737,37.5544331973922,38.5520874927107,
39.5497417880292,40.5473960833477,41.5450503786662,42.5427046739847,43.5403589693032,
44.5380132646217,45.5356675599403,46.5333218552588,47.5309761505773,48.5286304458958,
49.5262847412143,50.5239390365328,51.5215933318513,52.5192476271698,53.5169019224883,
54.5145562178069,55.5122105131254,56.5098648084439,57.5075191037624,58.5051733990809,
59.5028276943994,60.5004819897179,61.4981362850364,62.4957905803549,63.4934448756734,
64.491099170992,65.4887534663105,66.486407761629,67.4840620569475,68.481716352266,
69.4793706475845,70.477024942903,71.4746792382215,72.4723335335401,73.4699878288586,
74.4676421241771,75.4652964194956,76.4629507148141,77.4606050101326,78.4582593054511,
79.4559136007696,80.4535678960881,81.4512221914066,82.4488764867252,83.4465307820437,
84.4441850773622,85.4418393726807,86.4394936679992,87.4371479633177,88.4348022586362,
89.4324565539547,90.4301108492732,91.4277651445918,92.4254194399103,93.4230737352288,
94.4207280305473,95.4183823258658,96.4160366211843,97.4136909165028,98.4113452118213,
99.4089995071398,100.406653802458,101.404308097777,102.401962393095,103.399616688414,
104.397270983732,105.394925279051,106.392579574369,107.390233869688,108.387888165006,
109.385542460325,110.383196755643,111.380851050962,112.37850534628,113.376159641599,
114.373813936918,115.371468232236,116.369122527555,117.366776822873,118.364431118192,
119.36208541351,120.359739708829,121.357394004147,122.355048299466,123.352702594784,
124.350356890103,125.348011185421,126.34566548074,127.343319776058,128.340974071377,
129.338628366695,130.336282662014,131.333936957332,132.331591252651,133.329245547969,
134.326899843288,135.324554138606,136.322208433925,137.319862729243,138.317517024562,
139.31517131988,140.312825615199,141.310479910517,142.308134205836,143.305788501154,
144.303442796473,145.301097091791,146.29875138711,147.296405682428,148.294059977747,
149.291714273065,150.289368568384,151.287022863702,152.284677159021,153.282331454339,
154.279985749658,155.277640044976,156.275294340295,157.272948635613,158.270602930932,
159.268257226251,160.265911521569,161.263565816888,162.261220112206,163.258874407525,
164.256528702843,165.254182998162,166.25183729348,167.249491588799,168.247145884117,
169.244800179436,170.242454474754,171.240108770073,172.237763065391,173.23541736071,
174.233071656028,175.230725951347,176.228380246665,177.226034541984,178.223688837302,
179.221343132621,180.218997427939,181.216651723258,182.214306018576,183.211960313895,
184.209614609213,185.207268904532,186.20492319985,187.202577495169,188.200231790487,
189.197886085806,190.195540381124,191.193194676443,192.190848971761,193.18850326708,
194.186157562398,195.183811857717,196.181466153035,197.179120448354,198.176774743672,
199.174429038991,200.172083334309,201.169737629628,202.167391924946,203.165046220265,
204.162700515584,205.160354810902,206.158009106221,207.155663401539,208.153317696858,
209.150971992176,210.148626287495,211.146280582813,212.143934878132,213.14158917345,
214.139243468769,215.136897764087,216.134552059406,217.132206354724,218.129860650043,
219.127514945361,220.12516924068,221.122823535998,222.120477831317,223.118132126635,
224.115786421954,225.113440717272,226.111095012591,227.108749307909,228.106403603228,
229.104057898546),.UNSPECIFIED.);
#141=B_SPLINE_SURFACE_WITH_KNOTS('',3,3,((#30599,#30600,#30601,#30602,#30603,
#30604,#30605,#30606,#30607,#30608,#30609,#30610,#30611,#30612,#30613,#30614,
#30615,#30616,#30617,#30618,#30619,#30620,#30621,#30622,#30623,#30624,#30625,
#30626,#30627,#30628,#30629,#30630,#30631,#30632,#30633,#30634,#30635,#30636,
#30637,#30638,#30639),(#30640,#30641,#30642,#30643,#30644,#30645,#30646,
#30647,#30648,#30649,#30650,#30651,#30652,#30653,#30654,#30655,#30656,#30657,
#30658,#30659,#30660,#30661,#30662,#30663,#30664,#30665,#30666,#30667,#30668,
#30669,#30670,#30671,#30672,#30673,#30674,#30675,#30676,#30677,#30678,#30679,
#30680),(#30681,#30682,#30683,#30684,#30685,#30686,#30687,#30688,#30689,
#30690,#30691,#30692,#30693,#30694,#30695,#30696,#30697,#30698,#30699,#30700,
#30701,#30702,#30703,#30704,#30705,#30706,#30707,#30708,#30709,#30710,#30711,
#30712,#30713,#30714,#30715,#30716,#30717,#30718,#30719,#30720,#30721),
(#30722,#30723,#30724,#30725,#30726,#30727,#30728,#30729,#30730,#30731,
#30732,#30733,#30734,#30735,#30736,#30737,#30738,#30739,#30740,#30741,#30742,
#30743,#30744,#30745,#30746,#30747,#30748,#30749,#30750,#30751,#30752,#30753,
#30754,#30755,#30756,#30757,#30758,#30759,#30760,#30761,#30762)),
 .UNSPECIFIED.,.F.,.F.,.F.,(4,4),(4,1,1,1,1,1,1,1,1,1,1,1,1,1,1,1,1,1,1,
1,1,1,1,1,1,1,1,1,1,1,1,1,1,1,1,1,1,1,4),(-0.000343277739397919,0.0451836381137164),
(11.8612367265173,12.8594360281068,13.8572920519568,14.8551480758068,15.8530040996568,
16.8508601235068,17.8487161473568,18.8465721712069,19.8444281950569,20.8422842189069,
21.8401402427569,22.8379962666069,23.8358522904569,24.833708314307,25.831564338157,
26.829420362007,27.827276385857,28.825132409707,29.822988433557,30.8208444574071,
31.8187004812571,32.8165565051071,33.8144125289571,34.8122685528071,35.8101245766571,
36.8079806005072,37.8058366243572,38.8036926482072,39.8015486720572,40.7994046959072,
41.7972607197572,42.7951167436073,43.7929727674573,44.7908287913073,45.7886848151573,
46.7865408390073,47.7843968628573,48.7822528867074,49.7801089105574),
 .UNSPECIFIED.);
#142=B_SPLINE_SURFACE_WITH_KNOTS('',3,3,((#30864,#30865,#30866,#30867,#30868,
#30869,#30870,#30871,#30872,#30873,#30874,#30875,#30876,#30877,#30878,#30879,
#30880,#30881,#30882,#30883,#30884,#30885,#30886,#30887,#30888,#30889,#30890,
#30891,#30892,#30893,#30894,#30895,#30896,#30897,#30898,#30899,#30900,#30901,
#30902,#30903,#30904),(#30905,#30906,#30907,#30908,#30909,#30910,#30911,
#30912,#30913,#30914,#30915,#30916,#30917,#30918,#30919,#30920,#30921,#30922,
#30923,#30924,#30925,#30926,#30927,#30928,#30929,#30930,#30931,#30932,#30933,
#30934,#30935,#30936,#30937,#30938,#30939,#30940,#30941,#30942,#30943,#30944,
#30945),(#30946,#30947,#30948,#30949,#30950,#30951,#30952,#30953,#30954,
#30955,#30956,#30957,#30958,#30959,#30960,#30961,#30962,#30963,#30964,#30965,
#30966,#30967,#30968,#30969,#30970,#30971,#30972,#30973,#30974,#30975,#30976,
#30977,#30978,#30979,#30980,#30981,#30982,#30983,#30984,#30985,#30986),
(#30987,#30988,#30989,#30990,#30991,#30992,#30993,#30994,#30995,#30996,
#30997,#30998,#30999,#31000,#31001,#31002,#31003,#31004,#31005,#31006,#31007,
#31008,#31009,#31010,#31011,#31012,#31013,#31014,#31015,#31016,#31017,#31018,
#31019,#31020,#31021,#31022,#31023,#31024,#31025,#31026,#31027)),
 .UNSPECIFIED.,.F.,.F.,.F.,(4,4),(4,1,1,1,1,1,1,1,1,1,1,1,1,1,1,1,1,1,1,
1,1,1,1,1,1,1,1,1,1,1,1,1,1,1,1,1,1,1,4),(-0.000237777559020256,0.0452322082991495),
(14.398141012777,15.395997036627,16.393853060477,17.391709084327,18.389565108177,
19.3874211320271,20.3852771558771,21.3831331797271,22.3809892035771,23.3788452274271,
24.3767012512771,25.3745572751272,26.3724132989772,27.3702693228272,28.3681253466772,
29.3659813705272,30.3638373943772,31.3616934182273,32.3595494420773,33.3574054659273,
34.3552614897773,35.3531175136273,36.3509735374774,37.3488295613274,38.3466855851774,
39.3445416090274,40.3423976328774,41.3402536567274,42.3381096805775,43.3359657044275,
44.3338217282775,45.3316777521275,46.3295337759775,47.3273897998275,48.3252458236776,
49.3231018475276,50.3209578713776,51.3188138952276,52.3170131439472),
 .UNSPECIFIED.);
#143=B_SPLINE_CURVE_WITH_KNOTS('',3,(#8253,#8254,#8255,#8256,#8257,#8258,
#8259,#8260,#8261,#8262,#8263,#8264,#8265,#8266,#8267,#8268,#8269,#8270,
#8271,#8272,#8273,#8274,#8275,#8276,#8277,#8278,#8279,#8280,#8281,#8282,
#8283,#8284,#8285,#8286,#8287,#8288,#8289,#8290,#8291,#8292,#8293,#8294,
#8295,#8296,#8297,#8298,#8299,#8300,#8301,#8302,#8303,#8304,#8305,#8306,
#8307,#8308,#8309,#8310,#8311,#8312,#8313,#8314,#8315,#8316,#8317,#8318,
#8319,#8320,#8321,#8322,#8323,#8324,#8325,#8326,#8327,#8328,#8329,#8330,
#8331,#8332,#8333,#8334,#8335,#8336,#8337,#8338,#8339,#8340,#8341,#8342,
#8343,#8344,#8345,#8346,#8347,#8348,#8349,#8350,#8351,#8352,#8353,#8354,
#8355,#8356,#8357,#8358,#8359,#8360,#8361,#8362,#8363,#8364,#8365,#8366,
#8367,#8368,#8369,#8370,#8371,#8372,#8373,#8374,#8375,#8376,#8377,#8378,
#8379,#8380,#8381,#8382,#8383,#8384,#8385,#8386,#8387,#8388,#8389,#8390,
#8391,#8392,#8393,#8394,#8395,#8396,#8397,#8398,#8399,#8400,#8401,#8402,
#8403,#8404,#8405,#8406,#8407,#8408,#8409,#8410,#8411,#8412,#8413,#8414,
#8415,#8416,#8417,#8418,#8419,#8420,#8421,#8422,#8423,#8424,#8425,#8426,
#8427,#8428,#8429,#8430,#8431,#8432),.UNSPECIFIED.,.F.,.F.,(4,2,2,2,2,2,
2,2,2,2,2,2,2,2,2,2,2,2,2,2,2,2,2,2,2,2,2,2,2,2,2,2,2,2,2,2,2,2,2,2,2,2,
2,2,2,2,2,2,2,2,2,2,2,2,2,2,2,2,2,2,2,2,2,2,2,2,2,2,2,2,2,2,2,2,2,2,2,2,
2,2,2,2,2,2,2,2,2,2,2,4),(-0.653335368055541,-0.630827744391981,-0.626780791882163,
-0.615626822227101,-0.613746386507816,-0.612773986726421,-0.611996972682137,
-0.611081108109938,-0.609417169194799,-0.600987942963921,-0.556733574729332,
-0.540402511494848,-0.537539421553271,-0.535750932317557,-0.534355220875731,
-0.532810773622695,-0.530272110915929,-0.521046244569413,-0.477579256047151,
-0.460385567031773,-0.458303841262293,-0.457304148793678,-0.456528658473224,
-0.455645529724309,-0.454098108893724,-0.447294147774132,-0.405054436843288,
-0.384578213990074,-0.38157676784101,-0.379775756134279,-0.378385853015247,
-0.376886876698328,-0.374508645759818,-0.366710711675292,-0.353961386986977,
-0.318721581419464,-0.304334472491172,-0.302369786948392,-0.301393524301113,
-0.300636770619692,-0.300635149391518,-0.300633934570592,-0.299773777137359,
-0.298296239677128,-0.292512595872408,-0.281693807009336,-0.260197418545613,
-0.228783310911029,-0.225338003047899,-0.223573337585265,-0.222177359960143,
-0.220612973393571,-0.21799528402457,-0.207930804816358,-0.162219818185453,
-0.148527226542504,-0.146557350854722,-0.145569231240051,-0.144791085512274,
-0.144786680978626,-0.144782342094403,-0.144778067499853,-0.144773855871636,
-0.14476970593007,-0.144765616428515,-0.144761586142939,-0.144757613893166,
-0.144753698522794,-0.144749838896611,-0.144746033926486,-0.144742282547943,
-0.144738583717294,-0.144734936410761,-0.14473133964255,-0.144727792454873,
-0.144724293904568,-0.144720843073948,-0.144717439062714,-0.143799095744793,
-0.142128551391516,-0.134081724732716,-0.0862253127166185,-0.074309960962854,
-0.0714277983940767,-0.0697756867164645,-0.0685093800882442,-0.0668722738521374,
-0.0639797476153101,-0.0504343015806197,-0.00237550598267959),
 .UNSPECIFIED.);
#144=B_SPLINE_CURVE_WITH_KNOTS('',3,(#8435,#8436,#8437,#8438,#8439,#8440,
#8441,#8442,#8443,#8444,#8445,#8446,#8447,#8448,#8449,#8450,#8451,#8452,
#8453,#8454,#8455,#8456,#8457,#8458,#8459,#8460,#8461,#8462,#8463,#8464,
#8465,#8466,#8467,#8468,#8469,#8470,#8471,#8472,#8473,#8474,#8475,#8476,
#8477,#8478,#8479,#8480),.UNSPECIFIED.,.F.,.F.,(4,3,3,3,3,3,3,3,3,3,3,3,
3,3,3,4),(11.6154215191109,11.8187185627336,12.0221213811096,12.225521337906,
12.4295729519081,12.6130758144294,12.8095574916101,13.0098506461445,13.2057833991446,
13.4082567544463,13.6107301097479,13.8095830942474,14.0081354944698,14.2064856860045,
14.405222870008,14.5586904309875),.UNSPECIFIED.);
#145=B_SPLINE_CURVE_WITH_KNOTS('',3,(#8485,#8486,#8487,#8488,#8489,#8490,
#8491,#8492,#8493,#8494,#8495,#8496,#8497,#8498,#8499,#8500,#8501,#8502,
#8503,#8504,#8505,#8506,#8507,#8508,#8509,#8510,#8511,#8512,#8513,#8514,
#8515,#8516,#8517,#8518,#8519,#8520,#8521,#8522,#8523,#8524,#8525,#8526,
#8527,#8528,#8529,#8530,#8531,#8532,#8533,#8534,#8535,#8536,#8537,#8538,
#8539,#8540,#8541,#8542,#8543,#8544,#8545,#8546,#8547,#8548,#8549,#8550,
#8551,#8552,#8553,#8554,#8555,#8556,#8557,#8558,#8559,#8560,#8561,#8562,
#8563,#8564,#8565,#8566,#8567,#8568,#8569,#8570,#8571,#8572,#8573,#8574,
#8575,#8576,#8577,#8578,#8579,#8580,#8581,#8582,#8583,#8584,#8585,#8586,
#8587,#8588,#8589,#8590,#8591,#8592,#8593,#8594,#8595,#8596,#8597,#8598,
#8599,#8600,#8601,#8602,#8603,#8604,#8605,#8606,#8607,#8608,#8609,#8610,
#8611,#8612,#8613,#8614,#8615,#8616,#8617,#8618,#8619,#8620,#8621,#8622,
#8623,#8624,#8625,#8626,#8627,#8628,#8629,#8630,#8631,#8632,#8633,#8634,
#8635,#8636,#8637,#8638,#8639,#8640,#8641,#8642,#8643,#8644,#8645,#8646,
#8647,#8648,#8649,#8650,#8651,#8652,#8653,#8654,#8655,#8656,#8657,#8658,
#8659,#8660,#8661,#8662,#8663,#8664,#8665,#8666,#8667,#8668,#8669,#8670,
#8671,#8672,#8673,#8674,#8675,#8676,#8677,#8678,#8679,#8680,#8681,#8682,
#8683,#8684,#8685,#8686,#8687,#8688,#8689,#8690,#8691,#8692,#8693,#8694,
#8695,#8696,#8697,#8698,#8699,#8700,#8701,#8702,#8703,#8704,#8705,#8706,
#8707,#8708,#8709,#8710,#8711,#8712),.UNSPECIFIED.,.F.,.F.,(4,2,2,2,2,2,
2,2,2,2,2,2,2,2,2,2,2,2,2,2,2,2,2,2,2,2,2,2,2,2,2,2,2,2,2,2,2,2,2,2,2,2,
2,2,2,2,2,2,2,2,2,2,2,2,2,2,2,2,2,2,2,2,2,2,2,2,2,2,2,2,2,2,2,2,2,2,2,2,
2,2,2,2,2,2,2,2,2,2,2,2,2,2,2,2,2,2,2,2,2,2,2,2,2,2,2,2,2,2,2,2,2,2,2,4),
(-1.6336654916901,-1.62824277434945,-1.62601171074565,-1.624708877687,-1.6233247278785,
-1.62161410474044,-1.61899596189488,-1.60680221938704,-1.6011802590482,
-1.55684017909535,-1.54916111619138,-1.54753892156619,-1.54663489729833,
-1.54585978304054,-1.54487991998877,-1.54289633121139,-1.5296339235447,
-1.48520136692885,-1.47340055857452,-1.47065690995958,-1.46907012892602,
-1.46768598011242,-1.46597775714764,-1.4633677530548,-1.45129750604337,
-1.44556096533492,-1.40129806456246,-1.39350831030722,-1.39188716495599,
-1.39098333430837,-1.39020826958534,-1.38922827148699,-1.38724344208687,
-1.37393644792458,-1.32949096921034,-1.31773095829262,-1.31499049362004,
-1.31340456923182,-1.31202058445466,-1.31031181617812,-1.30769959177109,
-1.29559297003898,-1.28989305877005,-1.24565483681943,-1.23784311635413,
-1.23622076067487,-1.23531673125631,-1.23454168558734,-1.23356200900558,
-1.23157908814874,-1.21833509092066,-1.17402336377544,-1.16207355744685,
-1.15931923840855,-1.15773004421791,-1.15634601748633,-1.15464080147506,
-1.15204069030614,-1.14011669802976,-1.13425294786415,-1.09002010954997,
-1.08216922476865,-1.08054405662702,-1.07963919938582,-1.07886366008202,
-1.07788370259289,-1.0759018980825,-1.06272293592201,-1.01822887514452,
-1.00642636019806,-1.00368159793581,-1.00209402781417,-1.00070909950449,
-0.998999792590983,-0.996387898992575,-0.984303707478293,-0.978562335419278,
-0.934265673249539,-0.926505505245042,-0.924885861743567,-0.923982208703502,
-0.923207402451168,-0.922227683627303,-0.920241865211176,-0.906873961270504,
-0.88411589228476,-0.851960939902135,-0.848540506939741,-0.846787635027711,
-0.845400566840057,-0.843845769683438,-0.841243335623051,-0.83123413446508,
-0.786213312405221,-0.783501460588735,-0.78068872680155,-0.771150793859352,
-0.769512412813916,-0.768516529635411,-0.767738571407755,-0.766856690726504,
-0.765335358356058,-0.758997735852844,-0.74658534600533,-0.715079298221367,
-0.706091953952895,-0.695113383326078,-0.692334032603312,-0.690722102582697,
-0.689338476098884,-0.687659041120033,-0.684489667747269,-0.663993301109061,
-0.653335368055541),.UNSPECIFIED.);
#146=B_SPLINE_CURVE_WITH_KNOTS('',3,(#8714,#8715,#8716,#8717,#8718,#8719,
#8720,#8721,#8722,#8723,#8724,#8725,#8726,#8727,#8728,#8729,#8730,#8731,
#8732,#8733,#8734,#8735),.UNSPECIFIED.,.F.,.F.,(4,3,3,3,3,3,3,4),(14.5586904309875,
14.6083844050664,14.8072779846533,15.0069681635862,15.205429275443,15.4057339879139,
15.6060387003849,15.7079632679491),.UNSPECIFIED.);
#147=B_SPLINE_CURVE_WITH_KNOTS('',3,(#8736,#8737,#8738,#8739,#8740,#8741,
#8742,#8743,#8744,#8745,#8746,#8747,#8748,#8749,#8750,#8751,#8752,#8753,
#8754,#8755,#8756,#8757,#8758,#8759,#8760,#8761,#8762,#8763,#8764,#8765,
#8766,#8767,#8768,#8769,#8770,#8771,#8772,#8773,#8774,#8775,#8776,#8777,
#8778,#8779,#8780,#8781,#8782,#8783,#8784,#8785,#8786,#8787,#8788,#8789,
#8790,#8791,#8792,#8793,#8794,#8795,#8796,#8797,#8798,#8799,#8800,#8801,
#8802,#8803,#8804,#8805,#8806,#8807,#8808,#8809,#8810,#8811,#8812,#8813,
#8814,#8815,#8816,#8817,#8818,#8819,#8820,#8821,#8822,#8823,#8824,#8825,
#8826,#8827,#8828,#8829,#8830,#8831,#8832,#8833,#8834,#8835,#8836,#8837,
#8838,#8839,#8840,#8841,#8842,#8843,#8844,#8845,#8846,#8847,#8848,#8849,
#8850,#8851,#8852,#8853,#8854,#8855,#8856,#8857,#8858,#8859,#8860,#8861,
#8862,#8863,#8864,#8865,#8866,#8867,#8868,#8869,#8870,#8871,#8872,#8873,
#8874,#8875,#8876,#8877,#8878,#8879,#8880,#8881,#8882,#8883,#8884,#8885,
#8886,#8887,#8888,#8889,#8890,#8891,#8892,#8893,#8894,#8895,#8896,#8897,
#8898,#8899,#8900,#8901,#8902,#8903,#8904,#8905,#8906,#8907,#8908,#8909,
#8910,#8911,#8912,#8913,#8914,#8915,#8916,#8917,#8918,#8919,#8920,#8921,
#8922,#8923,#8924,#8925),.UNSPECIFIED.,.F.,.F.,(4,2,2,2,2,2,2,2,2,2,2,2,
2,2,2,2,2,2,2,2,2,2,2,2,2,2,2,2,2,2,2,2,2,2,2,2,2,2,2,2,2,2,2,2,2,2,2,2,
2,2,2,2,2,2,2,2,2,2,2,2,2,2,2,2,2,2,2,2,2,2,2,2,2,2,2,2,2,2,2,2,2,2,2,2,
2,2,2,2,2,2,2,2,2,2,4),(-1.96156625886934,-1.92659860641184,-1.90732716118048,
-1.90286421065159,-1.90094647127445,-1.89954351095447,-1.8982517845789,
-1.8961662975017,-1.8910505695977,-1.85295586623046,-1.83677685872955,-1.82869766194432,
-1.82556091643153,-1.82328055334917,-1.82224677965939,-1.82150705897721,
-1.82076683087637,-1.81951432342556,-1.81614474862376,-1.77737520988576,
-1.75101524588943,-1.74680273494602,-1.74491784438801,-1.74350935177083,
-1.74219119292114,-1.74001398644813,-1.73441877740491,-1.72902251786991,
-1.68185009784626,-1.67344964171479,-1.67021757871639,-1.66857723309331,
-1.66755432831436,-1.66661569045782,-1.66586016418002,-1.66494256104391,
-1.66330661834126,-1.65625786254823,-1.65112631001996,-1.61401639950501,
-1.60075283621853,-1.59271817070388,-1.59030364055039,-1.58878965239272,
-1.58739112773879,-1.58558629130853,-1.58259410755891,-1.56301235661922,
-1.52015182014857,-1.51327333271664,-1.51171272841562,-1.51082253653344,
-1.51004662635945,-1.50904904701185,-1.50697192224075,-1.48075539495684,
-1.45662573109801,-1.44446585919773,-1.43692019679761,-1.43456166917119,
-1.43306137571554,-1.4316606324867,-1.42983175833002,-1.42675298709056,
-1.42001711839465,-1.41770846204196,-1.41716875646762,-1.41696492803138,
-1.40795048521513,-1.36463969373078,-1.35764500565798,-1.35607705176135,
-1.35518563671651,-1.35440955895738,-1.35341355539906,-1.35134824301463,
-1.32434638940583,-1.2954124703417,-1.28216332848089,-1.27932300317243,
-1.27771471567474,-1.27647054573972,-1.27484724908334,-1.2720161087679,
-1.26038097227321,-1.25422245589898,-1.20985943944406,-1.20211370256844,
-1.20049457541361,-1.1995908433108,-1.19881539007934,-1.19783419533342,
-1.19584416643524,-1.18238927459852,-1.16059938204844),.UNSPECIFIED.);
#148=B_SPLINE_CURVE_WITH_KNOTS('',3,(#8931,#8932,#8933,#8934,#8935,#8936,
#8937,#8938,#8939,#8940,#8941,#8942,#8943,#8944,#8945,#8946,#8947,#8948,
#8949,#8950,#8951,#8952,#8953,#8954,#8955,#8956,#8957,#8958,#8959,#8960,
#8961,#8962,#8963,#8964,#8965,#8966,#8967,#8968,#8969,#8970,#8971,#8972,
#8973,#8974,#8975,#8976,#8977,#8978,#8979,#8980,#8981,#8982,#8983,#8984,
#8985,#8986,#8987,#8988,#8989,#8990,#8991,#8992,#8993,#8994,#8995,#8996,
#8997,#8998,#8999,#9000,#9001,#9002,#9003,#9004,#9005,#9006,#9007,#9008,
#9009,#9010,#9011,#9012,#9013,#9014,#9015,#9016,#9017,#9018,#9019,#9020,
#9021,#9022,#9023,#9024,#9025,#9026,#9027,#9028,#9029,#9030,#9031,#9032,
#9033,#9034,#9035,#9036,#9037,#9038,#9039,#9040,#9041,#9042,#9043,#9044,
#9045,#9046,#9047,#9048,#9049,#9050,#9051,#9052,#9053,#9054,#9055,#9056,
#9057,#9058,#9059,#9060,#9061,#9062,#9063,#9064,#9065,#9066,#9067,#9068,
#9069,#9070,#9071,#9072,#9073,#9074,#9075,#9076,#9077,#9078,#9079,#9080,
#9081,#9082,#9083,#9084,#9085,#9086,#9087,#9088,#9089,#9090,#9091,#9092,
#9093,#9094,#9095,#9096,#9097,#9098,#9099,#9100,#9101,#9102,#9103,#9104,
#9105,#9106,#9107,#9108,#9109,#9110,#9111,#9112,#9113,#9114,#9115,#9116,
#9117,#9118,#9119,#9120,#9121,#9122,#9123,#9124,#9125,#9126,#9127,#9128,
#9129,#9130,#9131,#9132,#9133,#9134),.UNSPECIFIED.,.F.,.F.,(4,2,2,2,2,2,
2,2,2,2,2,2,2,2,2,2,2,2,2,2,2,2,2,2,2,2,2,2,2,2,2,2,2,2,2,2,2,2,2,2,2,2,
2,2,2,2,2,2,2,2,2,2,2,2,2,2,2,2,2,2,2,2,2,2,2,2,2,2,2,2,2,2,2,2,2,2,2,2,
2,2,2,2,2,2,2,2,2,2,2,2,2,2,2,2,2,2,2,2,2,2,2,4),(-0.801408127637272,-0.771904677294534,
-0.751442090154587,-0.748428518202366,-0.746617300878863,-0.745217680836779,
-0.743706329861739,-0.741304237752424,-0.733386602621748,-0.720392548290882,
-0.683066689877591,-0.680645798525123,-0.670881406783786,-0.669230887192859,
-0.668231001131795,-0.667452194474505,-0.666572096085563,-0.665059079143899,
-0.658829139984269,-0.646731802189187,-0.615311961864202,-0.595784809569082,
-0.592794302056391,-0.590989806409757,-0.589591149222151,-0.58807662181382,
-0.585660378563243,-0.577612350772039,-0.564318967812487,-0.527090627162658,
-0.515410864829396,-0.513511092530095,-0.512535428626712,-0.511760485328853,
-0.510853003212082,-0.509215519425141,-0.501155740811697,-0.457121788570278,
-0.451061783489783,-0.439352749456757,-0.436515784737386,-0.434891280240044,
-0.433647313499648,-0.432040620565844,-0.429207006864917,-0.416062417170359,
-0.387544125155396,-0.359970542496619,-0.357913715509054,-0.356919247295317,
-0.356142821151476,-0.355248846198673,-0.353672974964434,-0.346585723927676,
-0.302824429737408,-0.295737905645828,-0.283746050595315,-0.281141179661321,
-0.279434418599533,-0.278050198859604,-0.278046556306593,-0.278042933535727,
-0.278039330860513,-0.278035748120137,-0.278032185143909,-0.278028641790449,
-0.278025117901929,-0.27802161331344,-0.276454418593738,-0.27378638452301,
-0.270528827498608,-0.263883193018837,-0.218608880745754,-0.215607053633344,
-0.204047426930947,-0.202152034702858,-0.201177175042177,-0.200402106203344,
-0.199493588868725,-0.197852007844497,-0.189841277995573,-0.17179962766557,
-0.143562182184153,-0.142818928501005,-0.128370978435724,-0.125607678451565,
-0.123851801111013,-0.122462799847458,-0.121163245944523,-0.1189474899834,
-0.112262154601947,-0.101870128429215,-0.0841239827932793,-0.0506805348753447,
-0.0472186712931119,-0.0459515968833834,-0.0452081520807635,-0.0444189234570229,
-0.0433326806342394,-0.0421190019783787,-0.0400060299954982,-0.000460192131931113),
 .UNSPECIFIED.);
#149=B_SPLINE_CURVE_WITH_KNOTS('',3,(#9135,#9136,#9137,#9138,#9139,#9140,
#9141,#9142,#9143,#9144,#9145,#9146,#9147,#9148,#9149,#9150,#9151,#9152,
#9153,#9154,#9155,#9156,#9157,#9158,#9159,#9160,#9161,#9162,#9163,#9164,
#9165,#9166,#9167,#9168,#9169,#9170,#9171,#9172,#9173,#9174,#9175,#9176,
#9177,#9178,#9179,#9180,#9181,#9182),.UNSPECIFIED.,.F.,.F.,(4,2,2,2,2,2,
2,2,2,2,2,2,2,2,2,2,2,2,2,2,2,2,2,4),(-1.81289741918331,-1.79235234454203,
-1.78478324876529,-1.78272148458332,-1.7812503218432,-1.77995523560585,
-1.77855196256831,-1.77671541388916,-1.77361390266173,-1.74909585464625,
-1.73161125982571,-1.71276134110456,-1.70476946226344,-1.70312906515652,
-1.7022212026979,-1.70144668432188,-1.70047251592632,-1.69857848023461,
-1.68702630209632,-1.68239431982946,-1.67041134096808,-1.64675668637411,
-1.63539767253542,-1.6336654916901),.UNSPECIFIED.);
#150=B_SPLINE_CURVE_WITH_KNOTS('',3,(#9183,#9184,#9185,#9186,#9187,#9188,
#9189,#9190,#9191,#9192,#9193,#9194,#9195,#9196,#9197,#9198,#9199,#9200,
#9201,#9202,#9203,#9204,#9205,#9206,#9207,#9208,#9209,#9210,#9211,#9212,
#9213,#9214,#9215,#9216,#9217,#9218,#9219,#9220,#9221,#9222,#9223,#9224,
#9225,#9226,#9227,#9228,#9229,#9230,#9231,#9232,#9233,#9234,#9235,#9236,
#9237,#9238,#9239,#9240,#9241,#9242,#9243,#9244,#9245,#9246,#9247,#9248,
#9249,#9250,#9251,#9252,#9253,#9254,#9255,#9256,#9257,#9258,#9259,#9260,
#9261,#9262,#9263,#9264,#9265,#9266,#9267,#9268,#9269,#9270,#9271,#9272,
#9273,#9274,#9275,#9276,#9277,#9278,#9279,#9280,#9281,#9282,#9283,#9284,
#9285,#9286,#9287,#9288,#9289,#9290,#9291,#9292,#9293,#9294,#9295,#9296,
#9297,#9298,#9299,#9300,#9301,#9302,#9303,#9304,#9305,#9306,#9307,#9308,
#9309,#9310,#9311,#9312,#9313,#9314,#9315,#9316,#9317,#9318,#9319,#9320,
#9321,#9322,#9323,#9324,#9325,#9326,#9327,#9328,#9329,#9330,#9331,#9332,
#9333,#9334,#9335,#9336,#9337,#9338,#9339,#9340,#9341,#9342,#9343,#9344,
#9345,#9346,#9347,#9348,#9349,#9350,#9351,#9352,#9353,#9354,#9355,#9356,
#9357,#9358,#9359,#9360,#9361,#9362,#9363,#9364,#9365,#9366,#9367,#9368,
#9369,#9370,#9371,#9372,#9373,#9374,#9375,#9376,#9377,#9378,#9379,#9380,
#9381,#9382,#9383,#9384,#9385,#9386,#9387,#9388,#9389,#9390,#9391,#9392,
#9393,#9394,#9395,#9396,#9397,#9398,#9399,#9400,#9401,#9402,#9403,#9404,
#9405,#9406,#9407,#9408,#9409,#9410,#9411,#9412),.UNSPECIFIED.,.F.,.F.,
(4,2,2,2,2,2,2,2,2,2,2,2,2,2,2,2,2,2,2,2,2,2,2,2,2,2,2,2,2,2,2,2,2,2,2,
2,2,2,2,2,2,2,2,2,2,2,2,2,2,2,2,2,2,2,2,2,2,2,2,2,2,2,2,2,2,2,2,2,2,2,2,
2,2,2,2,2,2,2,2,2,2,2,2,2,2,2,2,2,2,2,2,2,2,2,2,2,2,2,2,2,2,2,2,2,2,2,2,
2,2,2,2,2,2,2,4),(-1.16059938204844,-1.1376397772446,-1.12627602602123,
-1.1235642455996,-1.12198454315578,-1.12059976257337,-1.11888194649149,
-1.11624076774638,-1.10370817248241,-1.09839856355534,-1.05405115718455,
-1.04639052196066,-1.04477748284121,-1.04387549746159,-1.0431003064223,
-1.04211799854659,-1.04012159902785,-1.02645301065094,-0.981337467812207,
-0.980728000890515,-0.97777127065291,-0.970968395755761,-0.968317500957512,
-0.96659675087213,-0.96521183928086,-0.963634416107002,-0.960932614519319,
-0.949700756310211,-0.904844704578137,-0.891299986684652,-0.889307262715579,
-0.888325648236691,-0.887550423730124,-0.88664769779691,-0.885031767615919,
-0.877327713087126,-0.83301917203181,-0.827450519045247,-0.815190331133996,
-0.81256684605222,-0.810854332565948,-0.809469725225646,-0.807885732046655,
-0.80515529101041,-0.79354231042098,-0.748945170347644,-0.735573487866166,
-0.733585926908107,-0.732605173851814,-0.731829884440097,-0.730926272233222,
-0.729306374000881,-0.721538602885769,-0.677278750639153,-0.67164297165601,
-0.659460346590478,-0.656842543132981,-0.655131817032984,-0.653747380126196,
-0.652162183977738,-0.649426138983973,-0.637734925803899,-0.593203211178834,
-0.579842744108246,-0.57785563847789,-0.57687502690842,-0.576099783551829,
-0.575196137709143,-0.57357608524576,-0.565805828057025,-0.521548910673776,
-0.515925333397171,-0.503727690052195,-0.501108819157562,-0.499397737304334,
-0.498013239680856,-0.496428223466524,-0.493693120062289,-0.482015714941103,
-0.437470293613529,-0.424107031283538,-0.422119764776551,-0.421139092677314,
-0.420363803615383,-0.419460101222214,-0.417839969156371,-0.410069726470485,
-0.365808978978721,-0.360176112749597,-0.347987368207441,-0.345368969248814,
-0.343657966719378,-0.342273380938134,-0.340688096280346,-0.337952105066744,
-0.334654785091259,-0.327895667582497,-0.282252028942882,-0.278007373554725,
-0.268121248016352,-0.26646460782486,-0.26546285836712,-0.264683753490306,
-0.263804632321155,-0.262296254837789,-0.256297409696362,-0.244803207878878,
-0.200084593430525,-0.194419701583132,-0.190137617062854,-0.188431824324415,
-0.187015054963182,-0.185713404355037,-0.18374539821509,-0.179839088431723),
 .UNSPECIFIED.);
#151=B_SPLINE_CURVE_WITH_KNOTS('',3,(#9417,#9418,#9419,#9420,#9421,#9422,
#9423,#9424,#9425,#9426,#9427,#9428,#9429,#9430,#9431,#9432,#9433,#9434,
#9435,#9436,#9437,#9438,#9439,#9440,#9441,#9442,#9443,#9444,#9445,#9446,
#9447,#9448,#9449,#9450,#9451,#9452,#9453,#9454,#9455,#9456,#9457,#9458,
#9459,#9460,#9461,#9462,#9463,#9464,#9465,#9466,#9467,#9468,#9469,#9470,
#9471,#9472,#9473,#9474,#9475,#9476,#9477,#9478,#9479,#9480,#9481,#9482,
#9483,#9484,#9485,#9486,#9487,#9488,#9489,#9490,#9491,#9492,#9493,#9494,
#9495,#9496,#9497,#9498,#9499,#9500,#9501,#9502,#9503,#9504,#9505,#9506,
#9507,#9508,#9509,#9510,#9511,#9512,#9513,#9514,#9515,#9516,#9517,#9518,
#9519,#9520,#9521,#9522,#9523,#9524,#9525,#9526,#9527,#9528,#9529,#9530,
#9531,#9532,#9533,#9534,#9535,#9536,#9537,#9538,#9539,#9540,#9541,#9542,
#9543,#9544,#9545,#9546,#9547,#9548,#9549,#9550,#9551,#9552,#9553,#9554,
#9555,#9556,#9557,#9558,#9559,#9560,#9561,#9562,#9563,#9564,#9565,#9566,
#9567,#9568,#9569,#9570,#9571,#9572,#9573,#9574,#9575,#9576,#9577,#9578,
#9579,#9580,#9581,#9582,#9583,#9584,#9585,#9586,#9587,#9588,#9589,#9590,
#9591,#9592,#9593,#9594,#9595,#9596,#9597,#9598,#9599,#9600,#9601,#9602,
#9603,#9604,#9605,#9606,#9607,#9608,#9609,#9610,#9611,#9612,#9613,#9614,
#9615,#9616,#9617,#9618,#9619,#9620,#9621,#9622,#9623,#9624,#9625,#9626,
#9627,#9628,#9629,#9630,#9631,#9632,#9633,#9634,#9635,#9636,#9637,#9638,
#9639,#9640,#9641,#9642,#9643,#9644,#9645,#9646,#9647,#9648,#9649,#9650,
#9651,#9652,#9653,#9654,#9655,#9656,#9657,#9658,#9659,#9660,#9661,#9662),
 .UNSPECIFIED.,.F.,.F.,(4,2,2,2,2,2,2,2,2,2,2,2,2,2,2,2,2,2,2,2,2,2,2,2,
2,2,2,2,2,2,2,2,2,2,2,2,2,2,2,2,2,2,2,2,2,2,2,2,2,2,2,2,2,2,2,2,2,2,2,2,
2,2,2,2,2,2,2,2,2,2,2,2,2,2,2,2,2,2,2,2,2,2,2,2,2,2,2,2,2,2,2,2,2,2,2,2,
2,2,2,2,2,2,2,2,2,2,2,2,2,2,2,2,2,2,2,2,2,2,2,2,2,2,4),(-1.78170360182271,
-1.7683034713062,-1.76015236616984,-1.75850313810802,-1.75759311919535,
-1.75681841226449,-1.75584610244542,-1.7539618167832,-1.74266556262803,
-1.73948173379604,-1.69417695521611,-1.6875210575979,-1.6842599541551,-1.68158696731005,
-1.68002014497342,-1.68001665882529,-1.68001315345354,-1.68000962869081,
-1.68000608437026,-1.68000252033479,-1.67999893643978,-1.6799953325033,
-1.67999170837276,-1.67998806410434,-1.6786040634517,-1.67689600952329,
-1.67428623934759,-1.66221675422773,-1.65648257263056,-1.61222843942018,
-1.60443125533508,-1.60280972901297,-1.60190585059751,-1.6011307634256,
-1.60015079482505,-1.59816643150886,-1.58487764914714,-1.54043328091605,
-1.52866065004123,-1.52591909480963,-1.52433282449036,-1.52294870594554,
-1.52123998724339,-1.51862823484705,-1.50653108257774,-1.50082076657738,
-1.45654737952848,-1.44877058525294,-1.44715024079711,-1.44624658910164,
-1.44547142993403,-1.44449102850313,-1.44250467060609,-1.42915784135289,
-1.38460988847945,-1.3729787048207,-1.37024720773038,-1.36866309708836,
-1.36727868011315,-1.36556677833113,-1.36294490741458,-1.35070585169779,
-1.34512190547531,-1.30075430359628,-1.29309009947167,-1.2914766452433,
-1.29057446657813,-1.28979910365859,-1.28881655769146,-1.28681965332622,
-1.27314336775102,-1.22792737328192,-1.21717892514324,-1.21451417774121,
-1.21294474717732,-1.21155851819679,-1.20982515731541,-1.20713388138239,
-1.19382234134101,-1.16103764777963,-1.13889122566265,-1.13635875792502,
-1.13527646427588,-1.13448819239254,-1.13374412780774,-1.13247266843914,
-1.1289801428155,-1.10267999448151,-1.07484765762306,-1.0618766250044,-1.05905417491396,
-1.05745002590426,-1.05620624249344,-1.05457942965848,-1.05173192746894,
-1.04453897210281,-0.994860709142551,-0.986297799958003,-0.98302502426953,
-0.980635604246661,-0.97968360741896,-0.978894906226537,-0.978064199925879,
-0.976773390819549,-0.972809368846552,-0.945708455311416,-0.909985235145147,
-0.904766067901712,-0.902653293736338,-0.901349022433496,-0.899935801846121,
-0.898009969296553,-0.893554244926042,-0.87445635710687,-0.847765591138597,
-0.826984890938684,-0.824869950215989,-0.823864122518408,-0.823086545253413,
-0.822199863358343,-0.820657124645047,-0.814037228101076,-0.801408127637272),
 .UNSPECIFIED.);
#152=B_SPLINE_CURVE_WITH_KNOTS('',3,(#9664,#9665,#9666,#9667,#9668,#9669,
#9670,#9671,#9672,#9673,#9674,#9675,#9676,#9677,#9678,#9679,#9680,#9681,
#9682,#9683,#9684,#9685,#9686,#9687,#9688,#9689,#9690,#9691,#9692,#9693,
#9694,#9695,#9696,#9697,#9698,#9699,#9700,#9701,#9702,#9703,#9704,#9705,
#9706,#9707,#9708,#9709,#9710,#9711),.UNSPECIFIED.,.F.,.F.,(4,2,2,2,2,2,
2,2,2,2,2,2,2,2,2,2,2,2,2,2,2,2,2,4),(-0.179839088431723,-0.179004660102891,
-0.172374834811605,-0.153999719879391,-0.126873490254025,-0.123674374577756,
-0.112527659510257,-0.110814604507059,-0.109796381892867,-0.109015163230315,
-0.108145490985755,-0.106679338754425,-0.101304554848563,-0.0793271074036512,
-0.0601174400930077,-0.0374409868942284,-0.0343738583758793,-0.0325469315184454,
-0.0311447844141434,-0.0298491743177718,-0.0283730448890918,-0.0262994601569834,
-0.0189618397680811,-0.000459929193491284),.UNSPECIFIED.);
#153=B_SPLINE_CURVE_WITH_KNOTS('',3,(#9712,#9713,#9714,#9715,#9716,#9717,
#9718,#9719,#9720,#9721,#9722,#9723,#9724,#9725,#9726,#9727,#9728,#9729,
#9730,#9731,#9732,#9733,#9734,#9735,#9736,#9737,#9738,#9739,#9740,#9741,
#9742,#9743,#9744,#9745,#9746,#9747,#9748,#9749,#9750,#9751,#9752,#9753,
#9754,#9755,#9756,#9757,#9758,#9759,#9760,#9761,#9762,#9763,#9764,#9765,
#9766,#9767,#9768,#9769,#9770,#9771,#9772,#9773,#9774,#9775,#9776,#9777,
#9778,#9779,#9780,#9781,#9782,#9783,#9784,#9785,#9786,#9787,#9788,#9789,
#9790,#9791,#9792,#9793,#9794,#9795,#9796,#9797,#9798,#9799,#9800,#9801,
#9802,#9803,#9804,#9805,#9806,#9807,#9808,#9809,#9810,#9811,#9812,#9813,
#9814,#9815,#9816,#9817,#9818,#9819,#9820,#9821,#9822,#9823,#9824,#9825,
#9826,#9827,#9828,#9829,#9830,#9831,#9832,#9833,#9834,#9835,#9836,#9837,
#9838,#9839,#9840,#9841,#9842,#9843,#9844,#9845,#9846,#9847,#9848,#9849,
#9850,#9851,#9852,#9853,#9854,#9855,#9856,#9857,#9858,#9859,#9860,#9861,
#9862,#9863,#9864,#9865,#9866,#9867,#9868,#9869,#9870,#9871,#9872,#9873,
#9874,#9875,#9876,#9877,#9878,#9879,#9880,#9881,#9882,#9883,#9884,#9885,
#9886,#9887,#9888,#9889,#9890,#9891,#9892,#9893,#9894,#9895,#9896,#9897,
#9898,#9899),.UNSPECIFIED.,.F.,.F.,(4,2,2,2,2,2,2,2,2,2,2,2,2,2,2,2,2,2,
2,2,2,2,2,2,2,2,2,2,2,2,2,2,2,2,2,2,2,2,2,2,2,2,2,2,2,2,2,2,2,2,2,2,2,2,
2,2,2,2,2,2,2,2,2,2,2,2,2,2,2,2,2,2,2,2,2,2,2,2,2,2,2,2,2,2,2,2,2,2,2,2,
2,2,2,4),(-1.96101216699422,-1.92376717516262,-1.91917787234555,-1.9170715814596,
-1.91586081289646,-1.91477679581723,-1.91398832062296,-1.91324491239542,
-1.91197642912747,-1.90850241090579,-1.87547801514069,-1.86158912457042,
-1.84852008682589,-1.84059656044399,-1.83824196921588,-1.83693558219688,
-1.83569195369257,-1.83406594785621,-1.83122140892527,-1.81941367803316,
-1.81692010615816,-1.78422705433009,-1.76863014499697,-1.76130508366823,
-1.75970556859133,-1.75880653793929,-1.75803098224364,-1.75704446118011,
-1.75502708662785,-1.75007437755261,-1.74882325422875,-1.71120624932441,
-1.68886568661235,-1.68556753951387,-1.68287050887521,-1.68129814241858,
-1.68005452906571,-1.67842843291343,-1.67558345517448,-1.66377002905829,
-1.65779691645305,-1.61374502958058,-1.60569256002353,-1.60405568913376,
-1.60314844501536,-1.60237364520623,-1.60139810459358,-1.5994984084991,
-1.5878133738894,-1.58430598393704,-1.53951502022394,-1.52959422421342,
-1.52699809262552,-1.525443918536,-1.52405542162033,-1.52229804978378,-1.51886029944821,
-1.48818017953218,-1.47300156061752,-1.45141937034938,-1.44888796864739,
-1.44780592253626,-1.44701775311612,-1.44627373119915,-1.44500223906049,
-1.44150906290255,-1.41531456876857,-1.38738726300822,-1.37439139561185,
-1.37156753483781,-1.36996317459946,-1.36871950786582,-1.36709325132243,
-1.36424776181924,-1.35242901342353,-1.34645996467531,-1.30240277478005,
-1.29435412790247,-1.29271742926612,-1.29181019781711,-1.29103535865443,
-1.29005970432006,-1.28815959654163,-1.2764656554289,-1.23927878053355,
-1.22598257637473,-1.21793239096081,-1.21551608655893,-1.21400165580142,
-1.21260318188758,-1.21079905653591,-1.20780943779862,-1.18832580841037,
-1.16006334462802),.UNSPECIFIED.);
#154=B_SPLINE_CURVE_WITH_KNOTS('',3,(#9905,#9906,#9907,#9908,#9909,#9910,
#9911,#9912,#9913,#9914,#9915,#9916,#9917,#9918,#9919,#9920,#9921,#9922,
#9923,#9924,#9925,#9926,#9927,#9928,#9929,#9930,#9931,#9932,#9933,#9934,
#9935,#9936,#9937,#9938,#9939,#9940,#9941,#9942,#9943,#9944,#9945,#9946,
#9947,#9948,#9949,#9950,#9951,#9952,#9953,#9954,#9955,#9956,#9957,#9958,
#9959,#9960,#9961,#9962,#9963,#9964,#9965,#9966,#9967,#9968,#9969,#9970,
#9971,#9972,#9973,#9974,#9975,#9976,#9977,#9978,#9979,#9980,#9981,#9982,
#9983,#9984,#9985,#9986,#9987,#9988,#9989,#9990,#9991,#9992,#9993,#9994,
#9995,#9996,#9997,#9998,#9999,#10000,#10001,#10002,#10003,#10004,#10005,
#10006,#10007,#10008,#10009,#10010,#10011,#10012,#10013,#10014,#10015,#10016,
#10017,#10018,#10019,#10020,#10021,#10022,#10023,#10024,#10025,#10026,#10027,
#10028,#10029,#10030,#10031,#10032,#10033,#10034,#10035,#10036,#10037,#10038,
#10039,#10040,#10041,#10042,#10043,#10044,#10045,#10046,#10047,#10048,#10049,
#10050,#10051,#10052,#10053,#10054,#10055,#10056,#10057,#10058,#10059,#10060,
#10061,#10062,#10063,#10064,#10065,#10066,#10067,#10068,#10069,#10070,#10071,
#10072,#10073,#10074,#10075,#10076,#10077,#10078,#10079,#10080,#10081,#10082,
#10083,#10084,#10085,#10086,#10087,#10088,#10089,#10090,#10091,#10092,#10093,
#10094,#10095,#10096),.UNSPECIFIED.,.F.,.F.,(4,2,2,2,2,2,2,2,2,2,2,2,2,
2,2,2,2,2,2,2,2,2,2,2,2,2,2,2,2,2,2,2,2,2,2,2,2,2,2,2,2,2,2,2,2,2,2,2,2,
2,2,2,2,2,2,2,2,2,2,2,2,2,2,2,2,2,2,2,2,2,2,2,2,2,2,2,2,2,2,2,2,2,2,2,2,
2,2,2,2,2,2,2,2,2,2,4),(-0.801823037117727,-0.784023688630058,-0.748236216965953,
-0.743586130610892,-0.734137760490493,-0.732502706660029,-0.731496521688587,
-0.730718715557687,-0.729831825304929,-0.728288847054723,-0.721669774653257,
-0.679532187120232,-0.659054313011043,-0.656039644380564,-0.654227841747118,
-0.65282781291851,-0.651316063679858,-0.648913431264255,-0.640994857138846,
-0.628000107946309,-0.59067408091829,-0.588205860252348,-0.578467710707284,
-0.576818153455657,-0.575818406173578,-0.575039430906672,-0.574158830909266,
-0.572644243380937,-0.566398001636382,-0.554254698223316,-0.522866566914076,
-0.503351584149827,-0.500360679939091,-0.498555806302408,-0.497156773936174,
-0.495641758255807,-0.493224558567718,-0.485171698523447,-0.471868650049994,
-0.434654141773758,-0.42295664892934,-0.421055775568878,-0.420079714382638,
-0.419304542715883,-0.41839689339127,-0.416759365443317,-0.408704504461344,
-0.36465233719712,-0.358600433035996,-0.346877533138093,-0.344038904018225,
-0.34241373939341,-0.341169421219202,-0.339562456542801,-0.336728893046519,
-0.333285133261875,-0.32610575247773,-0.280967774503045,-0.267332966169678,
-0.265336558013755,-0.264353846875286,-0.263578156060303,-0.262675364350169,
-0.261060248456879,-0.253495608508123,-0.209057037856655,-0.203567110206695,
-0.191219352075125,-0.188589374827605,-0.186874494202279,-0.185489208472802,
-0.184185854912427,-0.181955130936223,-0.174829591332179,-0.163534598241662,
-0.141246156991975,-0.113842073031692,-0.110345277958001,-0.109072826961984,
-0.108328342963589,-0.107539760286596,-0.106457257348446,-0.105248874065434,
-0.096530403189441,-0.0637805650890347,-0.0543807919409418,-0.047944208926656,
-0.0355754467491948,-0.032944031202,-0.0312286807453503,-0.0298433250117053,
-0.0285399838281314,-0.026987174811537,-0.0247253126703711,-0.0174352431576566,
-0.000459544977384845),.UNSPECIFIED.);
#155=B_SPLINE_CURVE_WITH_KNOTS('',3,(#10097,#10098,#10099,#10100,#10101,
#10102,#10103,#10104,#10105,#10106,#10107,#10108,#10109,#10110,#10111,#10112,
#10113,#10114,#10115,#10116,#10117,#10118,#10119,#10120,#10121,#10122,#10123,
#10124,#10125,#10126,#10127,#10128,#10129,#10130,#10131,#10132,#10133,#10134,
#10135,#10136,#10137,#10138),.UNSPECIFIED.,.F.,.F.,(4,2,2,2,2,2,2,2,2,2,
2,2,2,2,2,2,2,2,2,2,4),(-1.96082039462719,-1.92070626802204,-1.91715845252776,
-1.91461382190151,-1.91352933422924,-1.91274060793303,-1.91199702907982,
-1.91072838209475,-1.90725461064772,-1.87421821339129,-1.86065306692995,
-1.84738310607834,-1.83937084944378,-1.83700683909421,-1.83569950017748,
-1.83445544565923,-1.83283222266144,-1.83000102813636,-1.81836400302013,
-1.78688518876395,-1.78170360182271),.UNSPECIFIED.);
#156=B_SPLINE_CURVE_WITH_KNOTS('',3,(#10139,#10140,#10141,#10142,#10143,
#10144,#10145,#10146,#10147,#10148,#10149,#10150,#10151,#10152,#10153,#10154,
#10155,#10156,#10157,#10158,#10159,#10160,#10161,#10162,#10163,#10164,#10165,
#10166,#10167,#10168,#10169,#10170,#10171,#10172,#10173,#10174,#10175,#10176,
#10177,#10178,#10179,#10180,#10181,#10182,#10183,#10184,#10185,#10186,#10187,
#10188,#10189,#10190,#10191,#10192,#10193,#10194,#10195,#10196,#10197,#10198,
#10199,#10200,#10201,#10202,#10203,#10204,#10205,#10206,#10207,#10208,#10209,
#10210,#10211,#10212,#10213,#10214,#10215,#10216,#10217,#10218,#10219,#10220,
#10221,#10222,#10223,#10224,#10225,#10226,#10227,#10228,#10229,#10230,#10231,
#10232,#10233,#10234,#10235,#10236,#10237,#10238,#10239,#10240,#10241,#10242,
#10243,#10244,#10245,#10246,#10247,#10248,#10249,#10250,#10251,#10252,#10253,
#10254,#10255,#10256,#10257,#10258,#10259,#10260,#10261,#10262,#10263,#10264,
#10265,#10266,#10267,#10268,#10269,#10270,#10271,#10272,#10273,#10274,#10275,
#10276,#10277,#10278,#10279,#10280,#10281,#10282,#10283,#10284,#10285,#10286,
#10287,#10288,#10289,#10290,#10291,#10292,#10293,#10294,#10295,#10296,#10297,
#10298,#10299,#10300,#10301,#10302,#10303,#10304,#10305,#10306,#10307,#10308,
#10309,#10310,#10311,#10312,#10313,#10314,#10315,#10316,#10317,#10318,#10319,
#10320,#10321,#10322,#10323,#10324,#10325,#10326,#10327,#10328,#10329,#10330,
#10331,#10332,#10333,#10334,#10335,#10336,#10337,#10338,#10339,#10340,#10341,
#10342,#10343,#10344,#10345,#10346,#10347,#10348,#10349,#10350,#10351,#10352,
#10353,#10354,#10355,#10356,#10357,#10358,#10359,#10360,#10361,#10362,#10363,
#10364,#10365,#10366,#10367,#10368,#10369,#10370,#10371,#10372,#10373,#10374,
#10375,#10376,#10377,#10378,#10379,#10380,#10381,#10382,#10383,#10384,#10385,
#10386,#10387,#10388,#10389,#10390,#10391,#10392,#10393,#10394,#10395,#10396,
#10397,#10398,#10399,#10400),.UNSPECIFIED.,.F.,.F.,(4,2,2,2,2,2,2,2,2,2,
2,2,2,2,2,2,2,2,2,2,2,2,2,2,2,2,2,2,2,2,2,2,2,2,2,2,2,2,2,2,2,2,2,2,2,2,
2,2,2,2,2,2,2,2,2,2,2,2,2,2,2,2,2,2,2,2,2,2,2,2,2,2,2,2,2,2,2,2,2,2,2,2,
2,2,2,2,2,2,2,2,2,2,2,2,2,2,2,2,2,2,2,2,2,2,2,2,2,2,2,2,2,2,2,2,2,2,2,2,
2,2,2,2,2,2,2,2,2,2,2,2,4),(-1.16006334462802,-1.15695415773548,-1.14474945801418,
-1.1384835212994,-1.13696775675719,-1.13608710360694,-1.13530850417252,
-1.13430980687523,-1.13266316283683,-1.12297489238004,-1.12044201026335,
-1.11773919680172,-1.07264935312383,-1.0626171347475,-1.06001135200755,
-1.05845499964908,-1.05706681523399,-1.05531289005775,-1.05189147787606,
-1.01969367382795,-0.996664971587923,-0.987683575977689,-0.984301447550536,
-0.98184998017665,-0.980781908412959,-0.979996002807677,-0.979141695400166,
-0.977744027978682,-0.972812016930496,-0.964203164138319,-0.913636729286196,
-0.909632855671912,-0.905359791922181,-0.903655801450463,-0.902239835094713,
-0.900789427450258,-0.89866883324834,-0.892986555460999,-0.86254509480548,
-0.83001341333935,-0.826587213803111,-0.825326045222767,-0.824584079532824,
-0.82379474050363,-0.82270564491046,-0.820133158279236,-0.81653539403444,
-0.806706087163201,-0.790434250599599,-0.75551229896386,-0.750267129360909,
-0.748150329443177,-0.746845589379873,-0.745433442788112,-0.743511902949968,
-0.739078825493073,-0.720157113690752,-0.696429735461047,-0.69189367332266,
-0.672465848865159,-0.670360788465909,-0.669357068236445,-0.668579930658033,
-0.667692434270443,-0.666145216361041,-0.659459703818438,-0.617161185997022,
-0.596926086575843,-0.593918857449199,-0.592109796601966,-0.59071086913406,
-0.589199301478028,-0.586794796819266,-0.578850493438041,-0.565794242564795,
-0.528302874044586,-0.51652982154755,-0.5146269094935,-0.513650780184225,
-0.512876068996261,-0.511969566580366,-0.510335653515445,-0.502329443503596,
-0.45827481948449,-0.452358937542683,-0.440491888383449,-0.437896327364134,
-0.436192738284626,-0.434809137716271,-0.433219446646547,-0.430461757521969,
-0.418457603982108,-0.374156879685298,-0.360934898138545,-0.358952770209601,
-0.35797330452174,-0.357198324398725,-0.356294244948602,-0.354671563827857,
-0.346853483585681,-0.302647613358889,-0.296960961400647,-0.284838745673712,
-0.282225439913434,-0.280516312201983,-0.279132277810025,-0.279128611007164,
-0.279124964267943,-0.279121337871524,-0.279117731647333,-0.279114145433364,
-0.279110579073727,-0.279107032414747,-0.279103505295488,-0.279099997559475,
-0.277534013334995,-0.27486828581183,-0.271615246042411,-0.264981764272871,
-0.219770585861685,-0.217144613204222,-0.214781761059414,-0.20498229486787,
-0.203330010624083,-0.202329597795403,-0.201550721549415,-0.200670941485566,
-0.199159379667798,-0.193079815473416,-0.181369706556269,-0.179645560381916),
 .UNSPECIFIED.);
#157=B_SPLINE_CURVE_WITH_KNOTS('',3,(#10405,#10406,#10407,#10408,#10409,
#10410,#10411,#10412,#10413,#10414,#10415,#10416,#10417,#10418,#10419,#10420,
#10421,#10422,#10423,#10424,#10425,#10426,#10427,#10428,#10429,#10430,#10431,
#10432,#10433,#10434,#10435,#10436,#10437,#10438,#10439,#10440,#10441,#10442,
#10443,#10444,#10445,#10446,#10447,#10448,#10449,#10450,#10451,#10452,#10453,
#10454,#10455,#10456,#10457,#10458,#10459,#10460,#10461,#10462,#10463,#10464,
#10465,#10466,#10467,#10468,#10469,#10470,#10471,#10472,#10473,#10474,#10475,
#10476,#10477,#10478,#10479,#10480,#10481,#10482,#10483,#10484,#10485,#10486,
#10487,#10488,#10489,#10490,#10491,#10492,#10493,#10494,#10495,#10496,#10497,
#10498,#10499,#10500,#10501,#10502,#10503,#10504,#10505,#10506,#10507,#10508,
#10509,#10510,#10511,#10512,#10513,#10514,#10515,#10516,#10517,#10518,#10519,
#10520,#10521,#10522,#10523,#10524,#10525,#10526,#10527,#10528,#10529,#10530,
#10531,#10532,#10533,#10534,#10535,#10536,#10537,#10538,#10539,#10540,#10541,
#10542,#10543,#10544,#10545,#10546,#10547,#10548,#10549,#10550,#10551,#10552,
#10553,#10554,#10555,#10556,#10557,#10558,#10559,#10560,#10561,#10562,#10563,
#10564,#10565,#10566,#10567,#10568,#10569,#10570,#10571,#10572,#10573,#10574,
#10575,#10576,#10577,#10578,#10579,#10580,#10581,#10582,#10583,#10584,#10585,
#10586,#10587,#10588,#10589,#10590,#10591,#10592,#10593,#10594,#10595,#10596,
#10597,#10598,#10599,#10600,#10601,#10602,#10603,#10604,#10605,#10606,#10607,
#10608,#10609,#10610,#10611,#10612,#10613,#10614,#10615,#10616,#10617,#10618,
#10619,#10620,#10621,#10622,#10623,#10624,#10625,#10626,#10627,#10628,#10629,
#10630),.UNSPECIFIED.,.F.,.F.,(4,2,2,2,2,2,2,2,2,2,2,2,2,2,2,2,2,2,2,2,
2,2,2,2,2,2,2,2,2,2,2,2,2,2,2,2,2,2,2,2,2,2,2,2,2,2,2,2,2,2,2,2,2,2,2,2,
2,2,2,2,2,2,2,2,2,2,2,2,2,2,2,2,2,2,2,2,2,2,2,2,2,2,2,2,2,2,2,2,2,2,2,2,
2,2,2,2,2,2,2,2,2,2,2,2,2,2,2,2,2,2,2,2,4),(-1.78245136437627,-1.76744044651287,
-1.75496919641081,-1.74728112270941,-1.74490405263102,-1.74339802224992,
-1.74199611848338,-1.74017170218288,-1.73711360002286,-1.71486580862118,
-1.68499366565813,-1.67378534549286,-1.66985375023133,-1.66796819612799,
-1.66643876899596,-1.66556118299284,-1.66480902918777,-1.66382929018424,
-1.66184704944844,-1.64856351373072,-1.60412737186443,-1.5923178011154,
-1.58957297252364,-1.58798565011603,-1.58660111378115,-1.58489252232963,
-1.5822821607462,-1.57021433320557,-1.56447214109838,-1.52020452863946,
-1.5123993553305,-1.51077689030042,-1.50987259045687,-1.50909720466784,
-1.5081169389866,-1.50613223700723,-1.49285161387435,-1.44841284953191,
-1.43660277466148,-1.43385780268983,-1.43227039322715,-1.43088577849989,
-1.4291770871478,-1.42656656705961,-1.41449789444906,-1.40875552526734,
-1.36448531324231,-1.35667982495156,-1.35505727599923,-1.35415292678178,
-1.35337749705619,-1.35239717377589,-1.35041234846992,-1.33713063438558,
-1.2926887754824,-1.28087886780686,-1.27813380019534,-1.27654631418265,
-1.27516162006554,-1.27345281452343,-1.27084208980897,-1.25877189484171,
-1.25302995623571,-1.20875672779544,-1.20095144357245,-1.19932884235413,
-1.1984244506648,-1.19764897630252,-1.19666858605155,-1.19468359071432,
-1.18139937448144,-1.13695199547072,-1.125145703998,-1.12240078611983,-1.12081327756465,
-1.11942849894447,-1.11771950577922,-1.11510833937865,-1.10303313971384,
-1.09729475574108,-1.05301636508646,-1.04521395682267,-1.04359146636839,
-1.0426870677612,-1.04191154516288,-1.04093103968034,-1.03894563374888,
-1.02565163788004,-0.981186197547841,-0.969613041403155,-0.966786549053474,
-0.965164124911114,-0.963919684307093,-0.962309928405141,-0.959463764181939,
-0.946126913318555,-0.91683411388054,-0.890256546211244,-0.888179354489889,
-0.887180696211669,-0.886403645886897,-0.885511930484752,-0.883947141057405,
-0.8770251718542,-0.833945411873018,-0.82498038043356,-0.813851879763301,
-0.811062702029817,-0.809448885648118,-0.808079154677382,-0.806409161350799,
-0.803282707101805,-0.801823037117727),.UNSPECIFIED.);
#158=B_SPLINE_CURVE_WITH_KNOTS('',3,(#10632,#10633,#10634,#10635,#10636,
#10637,#10638,#10639,#10640,#10641,#10642,#10643,#10644,#10645,#10646,#10647,
#10648,#10649,#10650,#10651,#10652,#10653,#10654,#10655,#10656,#10657,#10658,
#10659,#10660,#10661,#10662,#10663,#10664,#10665,#10666,#10667,#10668,#10669,
#10670,#10671),.UNSPECIFIED.,.F.,.F.,(4,2,2,2,2,2,2,2,2,2,2,2,2,2,2,2,2,
2,2,4),(-0.179645560381916,-0.146159827420209,-0.129625542324312,-0.126756128831658,
-0.124968331411959,-0.123576090393712,-0.122278902789586,-0.120117575492598,
-0.113829602671236,-0.104254931678754,-0.0859058002356539,-0.0515823491832586,
-0.0482339200198023,-0.04698433590299,-0.0462444809476119,-0.0454533815944531,
-0.0443552942672115,-0.0431247166638934,-0.0409690007589198,-0.000460167162021457),
 .UNSPECIFIED.);
#159=B_SPLINE_CURVE_WITH_KNOTS('',3,(#10672,#10673,#10674,#10675,#10676,
#10677,#10678,#10679,#10680,#10681,#10682,#10683,#10684,#10685,#10686,#10687,
#10688,#10689,#10690,#10691,#10692,#10693,#10694,#10695,#10696,#10697,#10698,
#10699,#10700,#10701,#10702,#10703,#10704,#10705,#10706,#10707,#10708,#10709,
#10710,#10711,#10712,#10713,#10714,#10715,#10716,#10717,#10718,#10719,#10720,
#10721,#10722,#10723,#10724,#10725,#10726,#10727,#10728,#10729,#10730,#10731,
#10732,#10733,#10734,#10735,#10736,#10737,#10738,#10739,#10740,#10741,#10742,
#10743,#10744,#10745,#10746,#10747,#10748,#10749,#10750,#10751,#10752,#10753),
 .UNSPECIFIED.,.F.,.F.,(4,3,3,3,3,3,3,3,3,3,3,3,3,3,3,3,3,3,3,3,3,3,3,3,
3,3,3,4),(40.8407044966675,41.037551545115,41.2342884007446,41.4315010101563,
41.5450503786662,41.7435926695272,41.9433706706416,42.1414562093936,42.3420804416891,
42.5427046739847,42.7412469648515,42.9410249659644,43.1391105047221,43.3397347370126,
43.5403589693032,43.7389012601772,43.9386792612883,44.1367648000535,44.3373890323376,
44.5380132646217,44.73655555549,44.9363335566026,45.1344190953619,45.3350433276511,
45.5356675599403,45.7342191671502,45.9323412904286,45.9751165534704),
 .UNSPECIFIED.);
#160=B_SPLINE_CURVE_WITH_KNOTS('',3,(#10759,#10760,#10761,#10762,#10763,
#10764,#10765,#10766,#10767,#10768),.UNSPECIFIED.,.F.,.F.,(4,1,1,1,1,1,
1,4),(47.1238898038471,47.2191044401619,48.2167587354804,49.2144130307989,
50.2120673261174,51.209721621436,52.2073759167545,52.258435828933),
 .UNSPECIFIED.);
#161=B_SPLINE_CURVE_WITH_KNOTS('',3,(#10769,#10770,#10771,#10772,#10773,
#10774,#10775,#10776,#10777,#10778,#10779,#10780,#10781,#10782,#10783,#10784,
#10785,#10786,#10787,#10788,#10789,#10790,#10791,#10792,#10793,#10794,#10795,
#10796,#10797,#10798,#10799,#10800,#10801,#10802,#10803,#10804,#10805,#10806,
#10807,#10808,#10809,#10810,#10811,#10812,#10813,#10814,#10815,#10816,#10817,
#10818,#10819,#10820,#10821,#10822,#10823,#10824,#10825,#10826,#10827,#10828,
#10829,#10830,#10831,#10832,#10833,#10834,#10835,#10836,#10837,#10838,#10839,
#10840,#10841,#10842,#10843,#10844,#10845,#10846,#10847,#10848),
 .UNSPECIFIED.,.F.,.F.,(4,2,2,2,2,2,2,2,2,2,2,2,2,2,2,2,2,2,2,2,2,2,2,2,
2,2,2,2,2,2,2,2,2,2,2,2,2,2,2,4),(-1.96178773563397,-1.92347939810595,-1.91073511481936,
-1.90292598792833,-1.90053555319041,-1.89902662633692,-1.89762587074075,
-1.89580840232572,-1.89277393262601,-1.87151561093926,-1.84084783188495,
-1.82947385729186,-1.82550356473007,-1.8236047526262,-1.82208126938198,
-1.82119774096839,-1.82119520336292,-1.82119265557688,-1.82119009753962,
-1.82118752915564,-1.82118495033417,-1.8211823610022,-1.82117976106885,
-1.82117715043766,-1.82117429426872,-1.82117138581178,-1.82116842391008,
-1.82116540739256,-1.8211623350403,-1.82115920561571,-1.82115601783292,
-1.82115277037097,-1.82114946188555,-1.8211460909899,-1.82114265625302,
-1.82040032794713,-1.81940500783992,-1.81734421145247,-1.78996315859545,
-1.78245136437627),.UNSPECIFIED.);
#162=B_SPLINE_CURVE_WITH_KNOTS('',3,(#10850,#10851,#10852,#10853,#10854,
#10855,#10856,#10857,#10858,#10859,#10860,#10861,#10862,#10863,#10864,#10865,
#10866,#10867,#10868),.UNSPECIFIED.,.F.,.F.,(4,3,3,3,3,3,4),(45.9751165534704,
46.1731883187463,46.371748648452,46.5333218552588,46.7351974297426,46.936614823472,
47.1238898038471),.UNSPECIFIED.);
#163=B_SPLINE_CURVE_WITH_KNOTS('',3,(#10869,#10870,#10871,#10872,#10873,
#10874,#10875,#10876,#10877),.UNSPECIFIED.,.F.,.F.,(4,1,1,1,1,1,4),(47.1238961499042,
47.5309761505773,48.5286304458958,49.5262847412143,50.5239390365328,51.5215933318513,
52.2572181212454),.UNSPECIFIED.);
#164=B_SPLINE_CURVE_WITH_KNOTS('',3,(#10883,#10884,#10885,#10886,#10887,
#10888,#10889,#10890,#10891,#10892,#10893,#10894,#10895,#10896,#10897,#10898,
#10899,#10900,#10901,#10902,#10903,#10904,#10905,#10906,#10907,#10908,#10909,
#10910,#10911,#10912,#10913,#10914,#10915,#10916,#10917,#10918,#10919,#10920,
#10921,#10922,#10923,#10924,#10925,#10926,#10927,#10928,#10929,#10930,#10931,
#10932,#10933,#10934,#10935,#10936,#10937,#10938,#10939,#10940,#10941,#10942,
#10943,#10944,#10945,#10946,#10947,#10948,#10949,#10950,#10951,#10952,#10953,
#10954,#10955,#10956,#10957,#10958,#10959,#10960,#10961),.UNSPECIFIED.,
 .F.,.F.,(4,3,3,3,3,3,3,3,3,3,3,3,3,3,3,3,3,3,3,3,3,3,3,3,3,3,4),(53.4070753006206,
53.6059776023134,53.8012697164857,54.0019771119386,54.2026845073915,54.4012267982613,
54.6010047993735,54.7990903381343,54.9997145704222,55.20033880271,55.3988810935798,
55.598659094692,55.7967446334529,55.9973688657407,56.1979930980285,56.3965353888983,
56.5963133900105,56.7943989287714,56.9950231610592,57.195647393347,57.3941896842168,
57.593967685329,57.7920532240898,57.9926774563777,58.1933016886655,58.3918561713772,
58.5417292850076),.UNSPECIFIED.);
#165=B_SPLINE_CURVE_WITH_KNOTS('',3,(#10962,#10963,#10964,#10965,#10966),
 .UNSPECIFIED.,.F.,.F.,(4,1,4),(52.258435828933,53.205030212073,53.4070751110267),
 .UNSPECIFIED.);
#166=B_SPLINE_CURVE_WITH_KNOTS('',3,(#10968,#10969,#10970,#10971,#10972),
 .UNSPECIFIED.,.F.,.F.,(4,1,4),(52.2572181212454,52.5192476271698,53.4070663386681),
 .UNSPECIFIED.);
#167=B_SPLINE_CURVE_WITH_KNOTS('',3,(#10973,#10974,#10975,#10976,#10977,
#10978,#10979,#10980,#10981,#10982,#10983,#10984,#10985,#10986,#10987,#10988,
#10989,#10990,#10991,#10992,#10993,#10994,#10995,#10996,#10997,#10998,#10999,
#11000,#11001,#11002,#11003,#11004,#11005,#11006,#11007,#11008,#11009,#11010,
#11011,#11012,#11013,#11014,#11015,#11016,#11017,#11018,#11019,#11020,#11021,
#11022,#11023,#11024,#11025,#11026,#11027,#11028,#11029,#11030,#11031,#11032,
#11033,#11034,#11035,#11036,#11037,#11038,#11039,#11040,#11041,#11042,#11043,
#11044,#11045,#11046,#11047,#11048,#11049,#11050,#11051,#11052,#11053,#11054,
#11055,#11056,#11057,#11058,#11059,#11060,#11061,#11062,#11063,#11064,#11065,
#11066,#11067,#11068,#11069,#11070,#11071,#11072,#11073,#11074,#11075,#11076,
#11077,#11078,#11079,#11080,#11081,#11082,#11083,#11084,#11085,#11086,#11087,
#11088,#11089,#11090,#11091,#11092,#11093,#11094,#11095,#11096,#11097,#11098,
#11099,#11100,#11101,#11102,#11103,#11104,#11105,#11106,#11107,#11108,#11109,
#11110,#11111,#11112,#11113,#11114,#11115,#11116,#11117,#11118,#11119,#11120,
#11121,#11122,#11123,#11124,#11125,#11126,#11127,#11128,#11129,#11130,#11131,
#11132,#11133,#11134,#11135,#11136,#11137,#11138,#11139,#11140,#11141,#11142,
#11143,#11144,#11145,#11146,#11147,#11148,#11149,#11150,#11151,#11152,#11153,
#11154,#11155,#11156,#11157,#11158,#11159,#11160,#11161,#11162,#11163,#11164,
#11165,#11166,#11167,#11168,#11169,#11170,#11171,#11172,#11173,#11174,#11175,
#11176,#11177,#11178),.UNSPECIFIED.,.F.,.F.,(4,2,2,2,2,2,2,2,2,2,2,2,2,
2,2,2,2,2,2,2,2,2,2,2,2,2,2,2,2,2,2,2,2,2,2,2,2,2,2,2,2,2,2,2,2,2,2,2,2,
2,2,2,2,2,2,2,2,2,2,2,2,2,2,2,2,2,2,2,2,2,2,2,2,2,2,2,2,2,2,2,2,2,2,2,2,
2,2,2,2,2,2,2,2,2,2,2,2,2,2,2,2,2,4),(-1.96099419632204,-1.9513014516148,
-1.94705951164587,-1.94578983431876,-1.94492169502107,-1.9441940110656,
-1.94341529944014,-1.9424137279511,-1.940756701998,-1.93084818045289,-1.92480688438048,
-1.88994208877432,-1.87783407705868,-1.87031015121589,-1.86795254339656,
-1.86645140333815,-1.8650488587348,-1.86321616798416,-1.86012766341501,
-1.83632661012051,-1.80776401932063,-1.7967812745366,-1.79290358211023,
-1.79103690831438,-1.78952379918941,-1.78864836093318,-1.78787226852566,
-1.78687802310176,-1.78482095368383,-1.75738027635625,-1.73611252486617,
-1.72287171959117,-1.71484626714234,-1.71243310640668,-1.71091968139516,
-1.70952147906946,-1.70771678347637,-1.70472422476947,-1.68509287867101,
-1.65350122315967,-1.64158070348884,-1.63748503725748,-1.63554371449086,
-1.63397964407068,-1.63309383521585,-1.63231896430528,-1.63133966310854,
-1.62935794755935,-1.61613987482373,-1.57186099742114,-1.55986936415193,
-1.55711277197064,-1.55552342328942,-1.55413994866787,-1.55243629460014,
-1.54984020758755,-1.53796381210697,-1.53205178107876,-1.48797261876864,
-1.47996931392474,-1.47833559782826,-1.4774291621164,-1.4766544791083,-1.47567835335914,
-1.47377535273746,-1.46199701405454,-1.45879867385188,-1.42401399646666,
-1.40486802874797,-1.40174719177353,-1.40007901797911,-1.39871017640028,
-1.3970967062199,-1.39430638570165,-1.38315152433583,-1.37418258624708,
-1.34281894606483,-1.33047301571277,-1.3241597126109,-1.32264052491424,
-1.32175925565685,-1.32098102864057,-1.31998398700684,-1.3183424905339,
-1.30875141242944,-1.30608038552172,-1.26882902289581,-1.25585053328359,
-1.24793927144096,-1.24553836663165,-1.24402759529358,-1.24262839942346,
-1.24081757456435,-1.2378042992866,-1.21733797459818,-1.17517999007401,
-1.16855323294771,-1.16701024258132,-1.16612364974782,-1.16534630400568,
-1.16434100140869,-1.16222796112255,-1.16023075385596),.UNSPECIFIED.);
#168=B_SPLINE_CURVE_WITH_KNOTS('',3,(#11184,#11185,#11186,#11187,#11188,
#11189,#11190,#11191,#11192,#11193,#11194,#11195,#11196,#11197,#11198,#11199,
#11200,#11201,#11202,#11203,#11204,#11205,#11206,#11207,#11208,#11209,#11210,
#11211,#11212,#11213,#11214,#11215,#11216,#11217,#11218,#11219,#11220,#11221,
#11222,#11223,#11224,#11225,#11226,#11227,#11228,#11229,#11230,#11231,#11232,
#11233,#11234,#11235,#11236,#11237,#11238,#11239,#11240,#11241,#11242,#11243,
#11244,#11245,#11246,#11247,#11248,#11249,#11250,#11251,#11252,#11253,#11254,
#11255,#11256,#11257,#11258,#11259,#11260,#11261,#11262,#11263,#11264,#11265,
#11266,#11267,#11268,#11269,#11270,#11271,#11272,#11273,#11274,#11275,#11276,
#11277,#11278,#11279,#11280,#11281,#11282,#11283,#11284,#11285,#11286,#11287,
#11288,#11289,#11290,#11291,#11292,#11293,#11294,#11295,#11296,#11297,#11298,
#11299,#11300,#11301,#11302,#11303,#11304,#11305,#11306,#11307,#11308,#11309,
#11310,#11311,#11312,#11313,#11314,#11315,#11316,#11317,#11318,#11319,#11320,
#11321,#11322,#11323,#11324,#11325,#11326,#11327,#11328,#11329,#11330,#11331,
#11332,#11333,#11334,#11335,#11336,#11337,#11338,#11339,#11340,#11341,#11342,
#11343,#11344,#11345,#11346,#11347,#11348,#11349,#11350,#11351,#11352,#11353,
#11354,#11355,#11356,#11357,#11358,#11359,#11360,#11361,#11362,#11363,#11364,
#11365,#11366,#11367),.UNSPECIFIED.,.F.,.F.,(4,2,2,2,2,2,2,2,2,2,2,2,2,
2,2,2,2,2,2,2,2,2,2,2,2,2,2,2,2,2,2,2,2,2,2,2,2,2,2,2,2,2,2,2,2,2,2,2,2,
2,2,2,2,2,2,2,2,2,2,2,2,2,2,2,2,2,2,2,2,2,2,2,2,2,2,2,2,2,2,2,2,2,2,2,2,
2,2,2,2,2,2,4),(-0.801781197037416,-0.801564431273354,-0.784631761412556,
-0.781744864672891,-0.779951571262751,-0.778558361730735,-0.777023050695626,
-0.774513987802849,-0.765555515655339,-0.750078541015869,-0.712062461613006,
-0.704095050805247,-0.70254296593654,-0.701561886926095,-0.700786383110493,
-0.699882544302023,-0.698262408173563,-0.690496512902924,-0.646217299914841,
-0.640520903670275,-0.628406352664212,-0.625792588168675,-0.624082805189035,
-0.622698000843819,-0.621111138389204,-0.61836905316899,-0.606602228616763,
-0.562103221008747,-0.548796073611519,-0.546810231588376,-0.545829663022647,
-0.545054166827803,-0.544149881905276,-0.54252781110346,-0.534731130134631,
-0.490474515673364,-0.484742625951674,-0.472666880447668,-0.470055675414473,
-0.468346645942164,-0.466961839201605,-0.465374299774763,-0.462629333904826,
-0.450823271407513,-0.406349616592483,-0.393057678142898,-0.391072270933003,
-0.390091764204506,-0.389316242003469,-0.388411840638082,-0.386789345982134,
-0.378986540391174,-0.334732647199794,-0.317476722746825,-0.314317944878116,
-0.312641000883609,-0.311330850432392,-0.310032148055082,-0.307712460312073,
-0.300523745112187,-0.289148966853703,-0.265652444933814,-0.239581897585846,
-0.236086357381561,-0.234814108125912,-0.23406966760327,-0.233281068890367,
-0.232198443484937,-0.229665711286987,-0.201547070106141,-0.164858628775972,
-0.159682479308758,-0.157615771150551,-0.156189367115004,-0.154877006209078,
-0.153486256810861,-0.150084949845184,-0.116998059022532,-0.0838468120460744,
-0.080371619684191,-0.0791024991990548,-0.0783586534266667,-0.0775696526049132,
-0.0764848025660079,-0.0739393790443653,-0.0703908251530521,-0.0607605291338429,
-0.0252340113911307,-0.00623987725397335,-0.00300228405538259,-0.00133881889611477,
-0.00045986504465812),.UNSPECIFIED.);
#169=B_SPLINE_CURVE_WITH_KNOTS('',3,(#11368,#11369,#11370,#11371,#11372,
#11373,#11374,#11375,#11376,#11377,#11378,#11379,#11380,#11381,#11382,#11383,
#11384,#11385,#11386,#11387,#11388,#11389),.UNSPECIFIED.,.F.,.F.,(4,3,3,
3,3,3,3,4),(58.5417292850076,58.7398440414221,58.9379236735178,59.1364652376836,
59.190955983984,59.3995207274522,59.607179253882,59.690260417875),
 .UNSPECIFIED.);
#170=B_SPLINE_CURVE_WITH_KNOTS('',3,(#11390,#11391,#11392,#11393,#11394,
#11395,#11396,#11397,#11398,#11399,#11400,#11401,#11402,#11403,#11404,#11405,
#11406,#11407,#11408,#11409,#11410,#11411,#11412,#11413,#11414,#11415,#11416,
#11417,#11418,#11419,#11420,#11421,#11422,#11423,#11424,#11425,#11426,#11427,
#11428,#11429,#11430,#11431,#11432,#11433,#11434,#11435,#11436,#11437,#11438,
#11439,#11440,#11441,#11442,#11443,#11444,#11445,#11446,#11447,#11448,#11449,
#11450,#11451,#11452,#11453,#11454,#11455,#11456,#11457,#11458,#11459,#11460,
#11461,#11462,#11463,#11464,#11465,#11466,#11467,#11468,#11469,#11470,#11471,
#11472,#11473,#11474,#11475,#11476,#11477,#11478,#11479,#11480,#11481,#11482,
#11483,#11484,#11485,#11486,#11487,#11488,#11489,#11490,#11491,#11492,#11493,
#11494,#11495,#11496,#11497,#11498,#11499,#11500,#11501,#11502,#11503,#11504,
#11505,#11506,#11507,#11508,#11509,#11510,#11511,#11512,#11513,#11514,#11515,
#11516,#11517,#11518,#11519,#11520,#11521,#11522,#11523,#11524,#11525,#11526,
#11527,#11528,#11529,#11530,#11531,#11532,#11533,#11534,#11535,#11536,#11537,
#11538,#11539,#11540,#11541,#11542,#11543,#11544,#11545,#11546,#11547,#11548,
#11549,#11550,#11551,#11552,#11553,#11554,#11555,#11556,#11557,#11558,#11559,
#11560,#11561,#11562,#11563,#11564,#11565,#11566,#11567,#11568,#11569,#11570,
#11571,#11572,#11573,#11574,#11575,#11576,#11577,#11578,#11579,#11580,#11581,
#11582,#11583,#11584,#11585,#11586,#11587,#11588,#11589,#11590,#11591,#11592,
#11593,#11594,#11595,#11596,#11597,#11598,#11599,#11600,#11601,#11602,#11603,
#11604,#11605,#11606,#11607),.UNSPECIFIED.,.F.,.F.,(4,2,2,2,2,2,2,2,2,2,
2,2,2,2,2,2,2,2,2,2,2,2,2,2,2,2,2,2,2,2,2,2,2,2,2,2,2,2,2,2,2,2,2,2,2,2,
2,2,2,2,2,2,2,2,2,2,2,2,2,2,2,2,2,2,2,2,2,2,2,2,2,2,2,2,2,2,2,2,2,2,2,2,
2,2,2,2,2,2,2,2,2,2,2,2,2,2,2,2,2,2,2,2,2,2,2,2,2,2,4),(-1.16023075385596,
-1.14169237323851,-1.11328494959453,-1.10024368558995,-1.09230464009489,
-1.08990049019143,-1.08838885812221,-1.08698967384691,-1.08518000243611,
-1.08217112690073,-1.06189512891135,-1.019588407344,-1.01290766308251,-1.01136055927344,
-1.01047297696043,-1.00969566125427,-1.00869158297568,-1.00706287677514,
-0.997729450567957,-0.981122399408477,-0.940802439556804,-0.935874136615297,
-0.934016173491421,-0.932689704952575,-0.931290128595796,-0.929447343929366,
-0.925451336112224,-0.896067619335419,-0.859664942364794,-0.856551556868587,
-0.855338835730635,-0.85460617199995,-0.853809838362817,-0.852682847514768,
-0.849883616349157,-0.83630554657643,-0.817957217836522,-0.785617450479004,
-0.780337576845703,-0.778214564229497,-0.776908456817134,-0.775496753102549,
-0.773579239472408,-0.769170706726171,-0.750447177323274,-0.719163159974299,
-0.712729248105205,-0.702131495051325,-0.700441087596731,-0.699429497105781,
-0.698649213706853,-0.697775968861054,-0.696293687118452,-0.690440709891027,
-0.679418468458758,-0.650604289743791,-0.627110693576659,-0.624027072920194,
-0.622195395785192,-0.620792544437691,-0.619290021906622,-0.616928029913226,
-0.609371287519034,-0.597190500013532,-0.57301093143524,-0.562192712336125,
-0.558402420101115,-0.546587670848953,-0.544682805874833,-0.543706122264937,
-0.542931205032441,-0.542024731531962,-0.54039155148043,-0.532402369338922,
-0.488322463849142,-0.482429130606761,-0.470532961793422,-0.467934864853507,
-0.466230276213823,-0.464846308084849,-0.463256685772964,-0.460500369828686,
-0.448522402927491,-0.404191179446176,-0.390953875388645,-0.388970870322226,
-0.387991090652365,-0.387215920689549,-0.38631168715723,-0.384688897878654,
-0.376873510159706,-0.332653508326875,-0.326374065823214,-0.314766110908833,
-0.311960694958664,-0.310364083153132,-0.309098331123897,-0.307532106446033,
-0.304776231191199,-0.292805739122854,-0.248467104230335,-0.235225889118897,
-0.233242687560179,-0.232262843533949,-0.231487638706339,-0.230583382964214,
-0.22896059995211,-0.22114612221631,-0.179737736516157),.UNSPECIFIED.);
#171=B_SPLINE_CURVE_WITH_KNOTS('',3,(#11612,#11613,#11614,#11615,#11616,
#11617,#11618,#11619,#11620,#11621,#11622,#11623,#11624,#11625,#11626,#11627,
#11628,#11629,#11630,#11631,#11632,#11633,#11634,#11635,#11636,#11637,#11638,
#11639,#11640,#11641,#11642,#11643,#11644,#11645,#11646,#11647,#11648,#11649,
#11650,#11651,#11652,#11653,#11654,#11655,#11656,#11657,#11658,#11659,#11660,
#11661,#11662,#11663,#11664,#11665,#11666,#11667,#11668,#11669,#11670,#11671,
#11672,#11673,#11674,#11675,#11676,#11677,#11678,#11679,#11680,#11681,#11682,
#11683,#11684,#11685,#11686,#11687,#11688,#11689,#11690,#11691,#11692,#11693,
#11694,#11695,#11696,#11697,#11698,#11699,#11700,#11701,#11702,#11703,#11704,
#11705,#11706,#11707,#11708,#11709,#11710,#11711,#11712,#11713,#11714,#11715,
#11716,#11717,#11718,#11719,#11720,#11721,#11722,#11723,#11724,#11725,#11726,
#11727,#11728,#11729,#11730,#11731,#11732,#11733,#11734,#11735,#11736,#11737,
#11738,#11739,#11740,#11741,#11742,#11743,#11744,#11745,#11746,#11747,#11748,
#11749,#11750,#11751,#11752,#11753,#11754,#11755,#11756,#11757,#11758,#11759,
#11760,#11761,#11762,#11763,#11764,#11765,#11766,#11767,#11768,#11769,#11770,
#11771,#11772,#11773,#11774,#11775,#11776,#11777,#11778,#11779,#11780,#11781,
#11782,#11783,#11784,#11785,#11786,#11787,#11788,#11789,#11790,#11791,#11792,
#11793,#11794,#11795,#11796,#11797,#11798,#11799,#11800,#11801,#11802,#11803,
#11804,#11805,#11806,#11807,#11808,#11809,#11810,#11811,#11812,#11813,#11814,
#11815,#11816,#11817,#11818,#11819,#11820,#11821,#11822,#11823,#11824,#11825,
#11826,#11827,#11828,#11829,#11830,#11831,#11832,#11833,#11834,#11835,#11836,
#11837),.UNSPECIFIED.,.F.,.F.,(4,2,2,2,2,2,2,2,2,2,2,2,2,2,2,2,2,2,2,2,
2,2,2,2,2,2,2,2,2,2,2,2,2,2,2,2,2,2,2,2,2,2,2,2,2,2,2,2,2,2,2,2,2,2,2,2,
2,2,2,2,2,2,2,2,2,2,2,2,2,2,2,2,2,2,2,2,2,2,2,2,2,2,2,2,2,2,2,2,2,2,2,2,
2,2,2,2,2,2,2,2,2,2,2,2,2,2,2,2,2,2,2,2,4),(-1.78239840749006,-1.77284562178477,
-1.72778854987453,-1.71777087403357,-1.71516594519601,-1.71360955145615,
-1.7122209815346,-1.71046609554332,-1.70704130712832,-1.675825302405,-1.65445396972294,
-1.64365927870122,-1.63982580401912,-1.63797415348664,-1.63646822466227,
-1.63559538730729,-1.63559347561779,-1.63559241310626,-1.6355913502754,
-1.63559028715512,-1.63558922364734,-1.63485485296981,-1.63387469702792,
-1.63189021683031,-1.61861070353855,-1.57417630052034,-1.56236843104286,
-1.5596238294537,-1.55803661172293,-1.5566521508909,-1.55494363230592,-1.55233334427224,
-1.54026513508306,-1.53452420752606,-1.49025841048117,-1.48245447871828,
-1.48083215321063,-1.47992791442734,-1.47915257070224,-1.47817234500265,
-1.47618768085193,-1.46290560254032,-1.41846554068109,-1.40666148533971,
-1.4039170475879,-1.4023298104286,-1.40094526481334,-1.39923655440781,-1.39662581110934,
-1.38455239745824,-1.37881520388222,-1.33454412174122,-1.32674321952217,
-1.32512101416403,-1.32421677051514,-1.32344137835469,-1.32246103465894,
-1.32047594610352,-1.30718366948274,-1.26272480296003,-1.25094322009141,
-1.2482002758304,-1.24661331194263,-1.24522865369113,-1.24351935291935,
-1.24090686758408,-1.22880932318379,-1.22309282888017,-1.17880471165658,
-1.17102144590226,-1.16940025375004,-1.16849620003081,-1.1677207396055,
-1.16674001309906,-1.1647531796914,-1.15141050868083,-1.10686186725147,
-1.09520250361167,-1.09246822313687,-1.09088311162763,-1.08949818584946,
-1.08778612693812,-1.08516489680534,-1.07294617143502,-1.0673376690503,
-1.02296925849174,-1.01528157186809,-1.01366620817817,-1.01276339549851,
-1.01198775635481,-1.0110052058272,-1.00900942961206,-0.995389611623066,
-0.98124423528614,-0.943311722561338,-0.938198116727199,-0.936102683071357,
-0.93480134148511,-0.933385139599993,-0.93144414372252,-0.926902678137378,
-0.90711886907993,-0.876897772530609,-0.8709700969086,-0.866845968151487,
-0.859696072948218,-0.858197964127305,-0.857233426416594,-0.856458953790592,
-0.855542225640735,-0.853862716329921,-0.845051468345399,-0.801781197037416),
 .UNSPECIFIED.);
#172=B_SPLINE_CURVE_WITH_KNOTS('',3,(#11839,#11840,#11841,#11842,#11843,
#11844,#11845,#11846,#11847,#11848,#11849,#11850,#11851,#11852,#11853,#11854,
#11855,#11856,#11857,#11858,#11859,#11860,#11861,#11862,#11863,#11864,#11865,
#11866,#11867,#11868,#11869,#11870,#11871,#11872,#11873,#11874,#11875,#11876,
#11877,#11878,#11879,#11880,#11881,#11882,#11883,#11884,#11885,#11886,#11887,
#11888,#11889,#11890,#11891,#11892,#11893,#11894,#11895,#11896,#11897,#11898,
#11899,#11900,#11901,#11902,#11903,#11904,#11905,#11906,#11907,#11908,#11909,
#11910,#11911,#11912,#11913,#11914,#11915,#11916),.UNSPECIFIED.,.F.,.F.,
(4,2,2,2,2,2,2,2,2,2,2,2,2,2,2,2,2,2,2,2,2,2,2,2,2,2,2,2,2,2,2,2,2,2,2,
2,2,2,4),(-0.179737736516157,-0.1769232270991,-0.159644222022814,-0.156490498628278,
-0.154815044125389,-0.153505865105826,-0.153475766098181,-0.153451524629101,
-0.153431689909591,-0.153400337945444,-0.153370155173738,-0.153340997035231,
-0.15331273942471,-0.153285274796565,-0.153258509146771,-0.153232359639407,
-0.153206752727951,-0.153181622639818,-0.153156910148042,-0.153132561572531,
-0.15310852793948,-0.153084764295521,-0.153061229129292,-0.153037883877162,
-0.151356144806248,-0.147985758223778,-0.117994593050442,-0.0811636312334916,
-0.0780867407108284,-0.0768799022254691,-0.0761483265207869,-0.075350958552095,
-0.0742187631733703,-0.0713875196662592,-0.0575134608539688,-0.0253441239235573,
-0.00564734167008595,-0.00218675447415778,-0.000459928765327191),
 .UNSPECIFIED.);
#173=B_SPLINE_CURVE_WITH_KNOTS('',3,(#11917,#11918,#11919,#11920,#11921,
#11922,#11923,#11924,#11925,#11926,#11927,#11928,#11929,#11930,#11931,#11932,
#11933,#11934,#11935,#11936,#11937,#11938,#11939,#11940,#11941,#11942,#11943,
#11944,#11945,#11946,#11947,#11948,#11949,#11950,#11951,#11952,#11953,#11954,
#11955,#11956,#11957,#11958,#11959,#11960,#11961,#11962,#11963,#11964,#11965,
#11966,#11967,#11968,#11969,#11970,#11971,#11972,#11973,#11974,#11975,#11976,
#11977,#11978,#11979,#11980,#11981,#11982,#11983,#11984,#11985,#11986,#11987,
#11988,#11989,#11990,#11991,#11992,#11993,#11994,#11995,#11996,#11997,#11998,
#11999,#12000,#12001,#12002,#12003,#12004,#12005,#12006,#12007,#12008,#12009,
#12010,#12011,#12012,#12013,#12014,#12015,#12016,#12017,#12018,#12019,#12020,
#12021,#12022,#12023,#12024,#12025,#12026,#12027,#12028,#12029,#12030,#12031,
#12032,#12033,#12034,#12035,#12036,#12037,#12038,#12039,#12040,#12041,#12042,
#12043,#12044,#12045,#12046,#12047,#12048,#12049,#12050,#12051,#12052,#12053,
#12054,#12055,#12056,#12057,#12058,#12059,#12060,#12061,#12062,#12063,#12064,
#12065,#12066,#12067,#12068,#12069,#12070,#12071,#12072,#12073,#12074,#12075,
#12076,#12077,#12078,#12079,#12080,#12081,#12082,#12083,#12084,#12085,#12086,
#12087,#12088,#12089,#12090,#12091,#12092,#12093,#12094,#12095,#12096,#12097,
#12098,#12099,#12100,#12101,#12102,#12103,#12104,#12105,#12106,#12107,#12108,
#12109,#12110),.UNSPECIFIED.,.F.,.F.,(4,2,2,2,2,2,2,2,2,2,2,2,2,2,2,2,2,
2,2,2,2,2,2,2,2,2,2,2,2,2,2,2,2,2,2,2,2,2,2,2,2,2,2,2,2,2,2,2,2,2,2,2,2,
2,2,2,2,2,2,2,2,2,2,2,2,2,2,2,2,2,2,2,2,2,2,2,2,2,2,2,2,2,2,2,2,2,2,2,2,
2,2,2,2,2,2,2,4),(-1.9600875839387,-1.95934093715801,-1.95805933249976,
-1.95667819987209,-1.95482891097818,-1.95083423577423,-1.94672671667632,
-1.93497892918676,-1.89092130768535,-1.88293385487988,-1.881301859421,-1.88039616971909,
-1.87962199684674,-1.87864635117661,-1.8767438048867,-1.86495193330382,
-1.86115690531924,-1.83018701563879,-1.8154088803222,-1.80673597886826,
-1.80491064335427,-1.80353000125775,-1.8021497171777,-1.8008422165049,-1.79878192320611,
-1.7936348353588,-1.75646869809257,-1.74201405554711,-1.73239541927384,
-1.72885146347219,-1.72630953307478,-1.72522616150818,-1.72443823541844,
-1.72369541003229,-1.72242805827455,-1.7189579099933,-1.68604203700969,
-1.65607040410987,-1.65043352013277,-1.64882792003788,-1.64730045160312,
-1.64594980102297,-1.64422289553059,-1.64098771693729,-1.62167690995825,
-1.57865420762684,-1.57174479024544,-1.57018216749663,-1.56929159549042,
-1.56851548308769,-1.56751797563354,-1.56544298688517,-1.53906457028005,
-1.51500354297263,-1.50292256936688,-1.49541167328284,-1.49305614467637,
-1.49155584981712,-1.49015375987227,-1.48832118171311,-1.48523179305424,
-1.45166371568129,-1.43943946475487,-1.41775204615246,-1.41522200674474,
-1.41414060284988,-1.41335292417017,-1.41260938406906,-1.41133875518179,
-1.40784816982517,-1.38163238947312,-1.35375176496569,-1.34077152517159,
-1.33794991784222,-1.33634667376802,-1.33510379494901,-1.33347845813631,
-1.33063429577889,-1.31881715816348,-1.31285721994045,-1.26882475504054,
-1.2607851991246,-1.25914976991026,-1.25824316281056,-1.2574688084132,-1.25649370273112,
-1.25459448150224,-1.24289989439707,-1.2392540446794,-1.19459751745936,
-1.18472581909819,-1.18213496219784,-1.18058253093539,-1.17919469940038,
-1.17743696075175,-1.17399467190637,-1.15958133138081),.UNSPECIFIED.);
#174=B_SPLINE_CURVE_WITH_KNOTS('',3,(#12116,#12117,#12118,#12119,#12120,
#12121,#12122,#12123,#12124,#12125,#12126,#12127,#12128,#12129,#12130,#12131,
#12132,#12133,#12134,#12135,#12136,#12137,#12138,#12139,#12140,#12141,#12142,
#12143,#12144,#12145,#12146,#12147,#12148,#12149,#12150,#12151,#12152,#12153,
#12154,#12155,#12156,#12157,#12158,#12159,#12160,#12161,#12162,#12163,#12164,
#12165,#12166,#12167,#12168,#12169,#12170,#12171,#12172,#12173,#12174,#12175,
#12176,#12177,#12178,#12179,#12180,#12181,#12182,#12183,#12184,#12185,#12186,
#12187,#12188,#12189,#12190,#12191,#12192,#12193,#12194,#12195,#12196,#12197,
#12198,#12199,#12200,#12201,#12202,#12203,#12204,#12205,#12206,#12207,#12208,
#12209,#12210,#12211,#12212,#12213,#12214,#12215,#12216,#12217,#12218,#12219,
#12220,#12221,#12222,#12223,#12224,#12225,#12226,#12227,#12228,#12229,#12230,
#12231,#12232,#12233,#12234,#12235,#12236,#12237,#12238,#12239,#12240,#12241,
#12242,#12243,#12244,#12245,#12246,#12247,#12248,#12249,#12250,#12251,#12252,
#12253,#12254,#12255,#12256,#12257,#12258,#12259,#12260,#12261,#12262,#12263,
#12264,#12265,#12266,#12267,#12268,#12269,#12270,#12271,#12272,#12273,#12274,
#12275,#12276,#12277,#12278,#12279,#12280,#12281,#12282,#12283,#12284,#12285,
#12286,#12287,#12288,#12289,#12290,#12291,#12292,#12293,#12294,#12295,#12296,
#12297,#12298,#12299,#12300,#12301,#12302,#12303,#12304,#12305,#12306,#12307,
#12308,#12309,#12310,#12311,#12312,#12313,#12314,#12315,#12316,#12317,#12318,
#12319,#12320,#12321,#12322,#12323,#12324,#12325,#12326,#12327,#12328,#12329,
#12330,#12331,#12332,#12333,#12334,#12335),.UNSPECIFIED.,.F.,.F.,(4,2,2,
2,2,2,2,2,2,2,2,2,2,2,2,2,2,2,2,2,2,2,2,2,2,2,2,2,2,2,2,2,2,2,2,2,2,2,2,
2,2,2,2,2,2,2,2,2,2,2,2,2,2,2,2,2,2,2,2,2,2,2,2,2,2,2,2,2,2,2,2,2,2,2,2,
2,2,2,2,2,2,2,2,2,2,2,2,2,2,2,2,2,2,2,2,2,2,2,2,2,2,2,2,2,2,2,2,2,2,4),
(-0.801722752441873,-0.78065717023981,-0.767362084515214,-0.765377067388483,
-0.764396824969129,-0.763621546938173,-0.762717470689388,-0.76109566007094,
-0.753298060507483,-0.709056128687175,-0.703322235667132,-0.691253819841489,
-0.688643607569661,-0.686935134061989,-0.685550715385673,-0.683963552116032,
-0.681219062189337,-0.669412299506496,-0.624953702235781,-0.611667051281045,
-0.609682245572363,-0.608702020197228,-0.607926712834498,-0.607022553163146,
-0.60540047001783,-0.5975992232714,-0.553358021684475,-0.54762001048994,
-0.535555380534457,-0.532945348157145,-0.531236891174371,-0.529852418512279,
-0.528265119177102,-0.525520205636661,-0.513708653362249,-0.469251123666496,
-0.455965643469658,-0.45398080917297,-0.453000552705642,-0.452225212431715,
-0.451321004815732,-0.449698811778175,-0.441896582234841,-0.397653969918475,
-0.391914956011652,-0.379850639401331,-0.377240550463772,-0.375532036757892,
-0.374147505015917,-0.37256012350856,-0.369815031209097,-0.358002131985904,
-0.313543250445868,-0.30025377472458,-0.29827123072108,-0.297291408397522,
-0.296539287975931,-0.295661722340187,-0.294139317927457,-0.292259897439224,
-0.28834640497997,-0.277216274844477,-0.247761380106628,-0.225040245846044,
-0.221971851959613,-0.220144378650866,-0.218741929044931,-0.21723707896719,
-0.214865607327831,-0.207228221955087,-0.194868620467261,-0.172283141841685,
-0.144743779054548,-0.14268541881812,-0.141690526590898,-0.140948427976586,
-0.140945004504463,-0.140941644597975,-0.140938346837832,-0.140935109846264,
-0.14093193228487,-0.140928812829985,-0.140925750210286,-0.140922743198353,
-0.14091979059585,-0.140916891222301,-0.140914043927115,-0.140911435093213,
-0.1409088369345,-0.140906249362769,-0.140903672286988,-0.140901105617953,
-0.140898549279099,-0.140896003179264,-0.140893467241901,-0.140009651033863,
-0.138485285185047,-0.136585161562114,-0.132611404217846,-0.12122411065082,
-0.0904944251324556,-0.069343359262306,-0.0663115254870869,-0.0644947211505962,
-0.0630939494698289,-0.0615844847895973,-0.0591920876558504,-0.0513667070427022,
-0.0385839865583593,-0.000460346267092497),.UNSPECIFIED.);
#175=B_SPLINE_CURVE_WITH_KNOTS('',3,(#12336,#12337,#12338,#12339,#12340,
#12341,#12342,#12343,#12344,#12345,#12346,#12347,#12348,#12349,#12350,#12351,
#12352,#12353,#12354,#12355,#12356,#12357,#12358,#12359,#12360,#12361,#12362,
#12363,#12364,#12365,#12366,#12367,#12368,#12369,#12370,#12371,#12372,#12373,
#12374,#12375,#12376,#12377,#12378,#12379,#12380,#12381,#12382,#12383,#12384,
#12385,#12386,#12387,#12388,#12389,#12390,#12391,#12392,#12393),
 .UNSPECIFIED.,.F.,.F.,(4,2,2,2,2,2,2,2,2,2,2,2,2,2,2,2,2,2,2,2,2,2,2,2,
2,2,2,2,4),(-1.96155185877725,-1.94987305567131,-1.94854983047148,-1.94765950245194,
-1.9469272038431,-1.94615159644688,-1.94516776474917,-1.94360639721424,
-1.93548419247702,-1.92964326762137,-1.89364864512461,-1.88085803289035,
-1.87302840038722,-1.87063566330137,-1.8691261996907,-1.86772557693905,
-1.86590917406853,-1.86287844117196,-1.84177023273213,-1.81098481128685,
-1.79958134117371,-1.79560413647834,-1.79370293947677,-1.79216611434465,
-1.79128548516075,-1.79050954111915,-1.78952162698962,-1.78749838779007,
-1.78239840749006),.UNSPECIFIED.);
#176=B_SPLINE_CURVE_WITH_KNOTS('',3,(#12394,#12395,#12396,#12397,#12398,
#12399,#12400,#12401,#12402,#12403,#12404,#12405,#12406,#12407,#12408,#12409,
#12410,#12411,#12412,#12413,#12414,#12415,#12416,#12417,#12418,#12419,#12420,
#12421,#12422,#12423,#12424,#12425,#12426,#12427,#12428,#12429,#12430,#12431,
#12432,#12433,#12434,#12435,#12436,#12437,#12438,#12439,#12440,#12441,#12442,
#12443,#12444,#12445,#12446,#12447,#12448,#12449,#12450,#12451,#12452,#12453,
#12454,#12455,#12456,#12457,#12458,#12459,#12460,#12461,#12462,#12463,#12464,
#12465,#12466,#12467,#12468,#12469,#12470,#12471,#12472,#12473,#12474,#12475,
#12476,#12477,#12478,#12479,#12480,#12481,#12482,#12483,#12484,#12485,#12486,
#12487,#12488,#12489,#12490,#12491,#12492,#12493,#12494,#12495,#12496,#12497,
#12498,#12499,#12500,#12501,#12502,#12503,#12504,#12505,#12506,#12507,#12508,
#12509,#12510,#12511,#12512,#12513,#12514,#12515,#12516,#12517,#12518,#12519,
#12520,#12521,#12522,#12523,#12524,#12525,#12526,#12527,#12528,#12529,#12530,
#12531,#12532,#12533,#12534,#12535,#12536,#12537,#12538,#12539,#12540,#12541,
#12542,#12543,#12544,#12545,#12546,#12547,#12548,#12549,#12550,#12551,#12552,
#12553,#12554,#12555,#12556,#12557,#12558,#12559,#12560,#12561,#12562,#12563,
#12564,#12565,#12566,#12567,#12568,#12569,#12570,#12571,#12572,#12573,#12574,
#12575,#12576,#12577,#12578,#12579,#12580,#12581,#12582,#12583,#12584,#12585,
#12586,#12587,#12588,#12589,#12590,#12591,#12592,#12593,#12594,#12595,#12596,
#12597,#12598,#12599,#12600,#12601,#12602,#12603,#12604,#12605,#12606,#12607,
#12608,#12609),.UNSPECIFIED.,.F.,.F.,(4,2,2,2,2,2,2,2,2,2,2,2,2,2,2,2,2,
2,2,2,2,2,2,2,2,2,2,2,2,2,2,2,2,2,2,2,2,2,2,2,2,2,2,2,2,2,2,2,2,2,2,2,2,
2,2,2,2,2,2,2,2,2,2,2,2,2,2,2,2,2,2,2,2,2,2,2,2,2,2,2,2,2,2,2,2,2,2,2,2,
2,2,2,2,2,2,2,2,2,2,2,2,2,2,2,2,2,2,4),(-1.15958133138081,-1.14530457866119,
-1.12483368809695,-1.11163403576874,-1.10503853507038,-1.10349845086023,
-1.1026128107544,-1.10183583021972,-1.10083037770834,-1.09871481324313,
-1.07734590571552,-1.05121430682451,-1.03220486816744,-1.02776143864966,
-1.02583867904839,-1.02442686941848,-1.02312330519995,-1.02101035942866,
-1.01578427188395,-0.980307983620089,-0.963674202751702,-0.950258281455218,
-0.948270573228327,-0.947290286350016,-0.946515603785185,-0.945612959448085,
-0.94399556664806,-0.936254359713296,-0.892012388924327,-0.88641167918616,
-0.874203380763913,-0.871584734488881,-0.869874413800588,-0.868490939442315,
-0.866907541422678,-0.864176358749767,-0.852533123478051,-0.808003830245064,
-0.794642339862062,-0.792656328679721,-0.791676356213017,-0.790901666489291,
-0.789998720170527,-0.788380054632066,-0.780618948074043,-0.73639083984906,
-0.730767925334323,-0.718582979154276,-0.715966268198572,-0.714256506900754,
-0.712873017385328,-0.711289088816377,-0.70855569364178,-0.696882942514304,
-0.652372416140613,-0.63902194840188,-0.637036228625098,-0.636056288953383,
-0.63528157083429,-0.634378529011887,-0.632759536698366,-0.624993921257931,
-0.580767230004565,-0.575139358219915,-0.562959158778991,-0.56034268924591,
-0.558632963075584,-0.557249420587868,-0.555665342022872,-0.552931462031809,
-0.541253135629998,-0.496744260384614,-0.483395236440537,-0.481409495622696,
-0.480429526121469,-0.479654774902392,-0.478751683562759,-0.477132575212989,
-0.469365887438029,-0.425137839085798,-0.419508892827036,-0.407329084537554,
-0.404712562444806,-0.403002780401332,-0.401619178408638,-0.400035016025266,
-0.397300951696883,-0.385621222195671,-0.341111021912406,-0.327761697339501,
-0.325775924943254,-0.324795923498939,-0.324036174860809,-0.323159646904321,
-0.32222035495408,-0.320778137973031,-0.318075969119637,-0.289943309751929,
-0.255409972254572,-0.250156961702153,-0.24803925756151,-0.246734667349714,
-0.245323236279037,-0.243403656949208,-0.238979513629093,-0.220123039434933,
-0.192053274695651,-0.179622088260795),.UNSPECIFIED.);
#177=B_SPLINE_CURVE_WITH_KNOTS('',3,(#12614,#12615,#12616,#12617,#12618,
#12619,#12620,#12621,#12622,#12623,#12624,#12625,#12626,#12627,#12628,#12629,
#12630,#12631,#12632,#12633,#12634,#12635,#12636,#12637,#12638,#12639,#12640,
#12641,#12642,#12643,#12644,#12645,#12646,#12647,#12648,#12649,#12650,#12651,
#12652,#12653,#12654,#12655,#12656,#12657,#12658,#12659,#12660,#12661,#12662,
#12663,#12664,#12665,#12666,#12667,#12668,#12669,#12670,#12671,#12672,#12673,
#12674,#12675,#12676,#12677,#12678,#12679,#12680,#12681,#12682,#12683,#12684,
#12685,#12686,#12687,#12688,#12689,#12690,#12691,#12692,#12693,#12694,#12695,
#12696,#12697,#12698,#12699,#12700,#12701,#12702,#12703,#12704,#12705,#12706,
#12707,#12708,#12709,#12710,#12711,#12712,#12713,#12714,#12715,#12716,#12717,
#12718,#12719,#12720,#12721,#12722,#12723,#12724,#12725,#12726,#12727,#12728,
#12729,#12730,#12731,#12732,#12733,#12734,#12735,#12736,#12737,#12738,#12739,
#12740,#12741,#12742,#12743,#12744,#12745,#12746,#12747,#12748,#12749,#12750,
#12751,#12752,#12753,#12754,#12755,#12756,#12757,#12758,#12759,#12760,#12761,
#12762,#12763,#12764,#12765,#12766,#12767,#12768,#12769,#12770,#12771,#12772,
#12773,#12774,#12775,#12776,#12777,#12778,#12779,#12780,#12781,#12782,#12783,
#12784,#12785,#12786,#12787,#12788,#12789,#12790,#12791,#12792,#12793,#12794,
#12795,#12796,#12797,#12798,#12799,#12800,#12801,#12802,#12803,#12804,#12805,
#12806,#12807,#12808,#12809,#12810,#12811,#12812,#12813,#12814,#12815,#12816,
#12817,#12818,#12819,#12820,#12821,#12822,#12823,#12824,#12825,#12826,#12827,
#12828,#12829,#12830,#12831,#12832,#12833,#12834,#12835,#12836,#12837,#12838,
#12839,#12840,#12841,#12842,#12843,#12844,#12845,#12846,#12847,#12848,#12849,
#12850,#12851,#12852,#12853),.UNSPECIFIED.,.F.,.F.,(4,2,2,2,2,2,2,2,2,2,
2,2,2,2,2,2,2,2,2,2,2,2,2,2,2,2,2,2,2,2,2,2,2,2,2,2,2,2,2,2,2,2,2,2,2,2,
2,2,2,2,2,2,2,2,2,2,2,2,2,2,2,2,2,2,2,2,2,2,2,2,2,2,2,2,2,2,2,2,2,2,2,2,
2,2,2,2,2,2,2,2,2,2,2,2,2,2,2,2,2,2,2,2,2,2,2,2,2,2,2,2,2,2,2,2,2,2,2,2,
2,4),(-1.78180985311435,-1.77825266409,-1.77649562722809,-1.77510332126124,
-1.7735695193173,-1.7710640873189,-1.76305956789903,-1.71703756079089,-1.7010450209152,
-1.69908708188978,-1.69811253487568,-1.69733795777592,-1.6964303012081,
-1.69483495978262,-1.68827533000465,-1.6461197212578,-1.63238871561382,
-1.62693790394529,-1.62411304409934,-1.62169750505939,-1.62018353819947,
-1.618785479316,-1.61698186749213,-1.61399304244887,-1.59450378578539,-1.56311469317457,
-1.55095924308641,-1.54471095845163,-1.54319689293844,-1.54231678012067,
-1.54153835441266,-1.54053947441449,-1.53889168835474,-1.52917270690637,
-1.52669317337052,-1.48942391024915,-1.47644110520431,-1.46852824512162,
-1.4661272400671,-1.46461648460115,-1.46321735495467,-1.46140668516399,
-1.45839380912516,-1.43793233570973,-1.39578945689481,-1.38916923725802,
-1.38762677788022,-1.38674032365478,-1.38596298602337,-1.384957529054,-1.38284356986091,
-1.36209628446893,-1.33541790232099,-1.32139939936812,-1.31587012253483,
-1.31173342415358,-1.30986479483821,-1.30846139265048,-1.30714287478308,
-1.3053145953017,-1.30057691663108,-1.29756869105931,-1.29525216762823,
-1.2935076318331,-1.29304438562751,-1.29286411014328,-1.24981118055704,
-1.23916166995177,-1.23344492648263,-1.23197435165953,-1.23110377104137,
-1.23032292026565,-1.22930672681737,-1.22760039788386,-1.21661706353546,
-1.21090926922551,-1.16707132855638,-1.15760298571133,-1.15504700621201,
-1.15350174146035,-1.1521115526828,-1.15033881644478,-1.14670743017367,
-1.14149006082097,-1.09818808706836,-1.08464385753197,-1.07793573764695,
-1.07638668388754,-1.07549868877602,-1.0747214674267,-1.07371809773257,
-1.07161536692718,-1.0528927141948,-1.04541857876941,-1.02129766906186,
-1.0029621897881,-0.999871271680354,-0.998209172260584,-0.996840192106802,
-0.995220529317871,-0.992404377093466,-0.980947526066571,-0.936394277279604,
-0.923052470168436,-0.921065984029007,-0.920085472414105,-0.919310204889693,
-0.91840639763235,-0.916785710074557,-0.909005665452878,-0.864751810349182,
-0.859038195805657,-0.846947967826858,-0.844336349654703,-0.842627479878105,
-0.84124308868024,-0.839656340490345,-0.836913541691698,-0.825129361556584,
-0.801722752441873),.UNSPECIFIED.);
#178=B_SPLINE_CURVE_WITH_KNOTS('',3,(#12855,#12856,#12857,#12858,#12859,
#12860,#12861,#12862,#12863,#12864,#12865,#12866,#12867,#12868,#12869,#12870,
#12871,#12872,#12873,#12874,#12875,#12876,#12877,#12878,#12879,#12880,#12881,
#12882,#12883,#12884,#12885,#12886,#12887,#12888,#12889,#12890,#12891,#12892,
#12893,#12894,#12895,#12896,#12897,#12898,#12899,#12900,#12901,#12902,#12903,
#12904,#12905,#12906,#12907,#12908,#12909,#12910,#12911,#12912,#12913,#12914,
#12915,#12916,#12917,#12918,#12919,#12920,#12921,#12922,#12923,#12924,#12925,
#12926,#12927,#12928,#12929,#12930,#12931,#12932,#12933,#12934,#12935,#12936,
#12937,#12938,#12939,#12940,#12941,#12942,#12943,#12944,#12945,#12946,#12947,
#12948,#12949,#12950,#12951,#12952,#12953,#12954),.UNSPECIFIED.,.F.,.F.,
(4,2,2,2,2,2,2,2,2,2,2,2,2,2,2,2,2,2,2,2,2,2,2,2,2,2,2,2,2,2,2,2,2,2,2,
2,2,2,2,2,2,2,2,2,2,2,2,2,2,4),(-0.179622088260795,-0.172374607901156,-0.170268173383137,
-0.169264380712101,-0.168517786869452,-0.168515300919091,-0.168512838350807,
-0.168510391795445,-0.168507961153133,-0.168505546309182,-0.168503147138293,
-0.168500763541524,-0.168498390557965,-0.168496023095012,-0.16849367057981,
-0.168491332887838,-0.16848900989474,-0.168486701502562,-0.16848440760483,
-0.168482128105852,-0.168479862891079,-0.168477611855461,-0.168475374894854,
-0.168473151915777,-0.168470942801158,-0.167595299574883,-0.166078007122841,
-0.16420799867126,-0.160321337522865,-0.149303453012972,-0.120512283999247,
-0.0969967272189737,-0.0939129301970814,-0.092081289530703,-0.0906785479401655,
-0.0891762227318545,-0.0868147085420767,-0.0792609286287479,-0.0670862848672435,
-0.027603499308661,-0.0219317403002707,-0.0201903824192217,-0.0155585596301801,
-0.01413575877173,-0.0132757739927139,-0.0125272992372366,-0.0117595462868871,
-0.0107489723956134,-0.00913518205521087,-0.000459424761613156),
 .UNSPECIFIED.);
#179=B_SPLINE_CURVE_WITH_KNOTS('',3,(#12955,#12956,#12957,#12958,#12959,
#12960,#12961,#12962,#12963,#12964,#12965,#12966,#12967,#12968,#12969,#12970,
#12971,#12972,#12973,#12974,#12975,#12976,#12977,#12978,#12979,#12980,#12981,
#12982,#12983,#12984,#12985,#12986,#12987,#12988,#12989,#12990,#12991,#12992,
#12993,#12994,#12995,#12996,#12997,#12998,#12999,#13000,#13001,#13002,#13003,
#13004,#13005,#13006,#13007,#13008,#13009,#13010,#13011,#13012,#13013,#13014,
#13015,#13016,#13017,#13018,#13019,#13020,#13021,#13022,#13023,#13024,#13025,
#13026,#13027,#13028,#13029,#13030,#13031,#13032,#13033,#13034,#13035,#13036,
#13037,#13038,#13039,#13040,#13041,#13042,#13043,#13044,#13045,#13046,#13047,
#13048,#13049,#13050,#13051,#13052,#13053,#13054,#13055,#13056,#13057,#13058,
#13059,#13060,#13061,#13062,#13063,#13064,#13065,#13066,#13067,#13068,#13069,
#13070,#13071,#13072,#13073,#13074,#13075,#13076,#13077,#13078,#13079,#13080,
#13081,#13082,#13083,#13084,#13085,#13086,#13087,#13088,#13089,#13090,#13091,
#13092,#13093,#13094,#13095,#13096,#13097,#13098,#13099,#13100,#13101,#13102,
#13103,#13104,#13105,#13106,#13107,#13108,#13109,#13110,#13111,#13112,#13113,
#13114,#13115,#13116,#13117,#13118,#13119,#13120,#13121,#13122,#13123,#13124,
#13125,#13126,#13127,#13128,#13129,#13130,#13131,#13132,#13133,#13134,#13135,
#13136,#13137,#13138,#13139,#13140,#13141,#13142,#13143,#13144,#13145,#13146,
#13147,#13148),.UNSPECIFIED.,.F.,.F.,(4,2,2,2,2,2,2,2,2,2,2,2,2,2,2,2,2,
2,2,2,2,2,2,2,2,2,2,2,2,2,2,2,2,2,2,2,2,2,2,2,2,2,2,2,2,2,2,2,2,2,2,2,2,
2,2,2,2,2,2,2,2,2,2,2,2,2,2,2,2,2,2,2,2,2,2,2,2,2,2,2,2,2,2,2,2,2,2,2,2,
2,2,2,2,2,2,2,4),(-1.96146538068136,-1.9225304253061,-1.90383070095087,
-1.89942562847256,-1.89750917597009,-1.89609808255127,-1.89479241568132,
-1.89266985006171,-1.88738973706424,-1.85528202876609,-1.83649722903484,
-1.82647857779344,-1.82283423001772,-1.82104874699235,-1.81959973659847,
-1.81873361870667,-1.81799537723252,-1.8170076092791,-1.81498337010756,
-1.80034046124051,-1.76891939329666,-1.74853947446037,-1.74392639143348,
-1.74197402508409,-1.74055658200039,-1.73925897767339,-1.73718027004422,
-1.73216192636669,-1.69289498133107,-1.66875524932273,-1.66623411913357,
-1.66486091963958,-1.663950140907,-1.66309578857874,-1.66234179059955,-1.66133569521654,
-1.6592181873244,-1.63767628734376,-1.61167560092799,-1.59267664780642,
-1.58823361519605,-1.58631041073267,-1.58489804135184,-1.58359379629092,
-1.58147937975776,-1.57624784314212,-1.5408468668102,-1.52496766467099,
-1.51182417719274,-1.50907306176176,-1.50795408195252,-1.50715941646251,
-1.50642517799848,-1.5052035419586,-1.50203400902748,-1.5010768211437,-1.49979667073604,
-1.4971082564235,-1.49309684180038,-1.47779986719723,-1.45355051130261,
-1.43499031598387,-1.43189117131455,-1.43022754115955,-1.42885879593576,
-1.4272411739766,-1.42443300338077,-1.41306767427709,-1.40984903105896,
-1.37452851755286,-1.36104362060793,-1.35435460297857,-1.35280708310944,
-1.35191950531526,-1.35114235225081,-1.35013869353996,-1.34851108121659,
-1.33919493806612,-1.33644715284248,-1.2995318673895,-1.28618441373468,
-1.27811248441603,-1.27569414257748,-1.27417944215607,-1.27278140428006,
-1.27097879966951,-1.26799377395149,-1.24866739678322,-1.20562925313045,
-1.19871914053297,-1.19715568099967,-1.19626452508796,-1.19548783489501,
-1.19448949442455,-1.19241245943815,-1.16588454451059,-1.16050672125936),
 .UNSPECIFIED.);
#180=B_SPLINE_CURVE_WITH_KNOTS('',3,(#13154,#13155,#13156,#13157,#13158,
#13159,#13160,#13161,#13162,#13163,#13164,#13165,#13166,#13167,#13168,#13169,
#13170,#13171,#13172,#13173,#13174,#13175,#13176,#13177,#13178,#13179,#13180,
#13181,#13182,#13183,#13184,#13185,#13186,#13187,#13188,#13189,#13190,#13191,
#13192,#13193,#13194,#13195,#13196,#13197,#13198,#13199,#13200,#13201,#13202,
#13203,#13204,#13205,#13206,#13207,#13208,#13209,#13210,#13211,#13212,#13213,
#13214,#13215,#13216,#13217,#13218,#13219,#13220,#13221,#13222,#13223,#13224,
#13225,#13226,#13227,#13228,#13229,#13230,#13231,#13232,#13233,#13234,#13235,
#13236,#13237,#13238,#13239,#13240,#13241,#13242,#13243,#13244,#13245,#13246,
#13247,#13248,#13249,#13250,#13251,#13252,#13253,#13254,#13255,#13256,#13257,
#13258,#13259,#13260,#13261,#13262,#13263,#13264,#13265,#13266,#13267,#13268,
#13269,#13270,#13271,#13272,#13273,#13274,#13275,#13276,#13277,#13278,#13279,
#13280,#13281,#13282,#13283,#13284,#13285,#13286,#13287,#13288,#13289,#13290,
#13291,#13292,#13293,#13294,#13295,#13296,#13297,#13298,#13299,#13300,#13301,
#13302,#13303,#13304,#13305,#13306,#13307,#13308,#13309,#13310,#13311,#13312,
#13313,#13314,#13315,#13316,#13317,#13318,#13319,#13320,#13321,#13322,#13323,
#13324,#13325,#13326,#13327,#13328,#13329,#13330,#13331,#13332,#13333,#13334,
#13335,#13336,#13337,#13338,#13339,#13340,#13341,#13342,#13343,#13344,#13345,
#13346,#13347,#13348,#13349,#13350,#13351,#13352,#13353,#13354,#13355,#13356,
#13357),.UNSPECIFIED.,.F.,.F.,(4,2,2,2,2,2,2,2,2,2,2,2,2,2,2,2,2,2,2,2,
2,2,2,2,2,2,2,2,2,2,2,2,2,2,2,2,2,2,2,2,2,2,2,2,2,2,2,2,2,2,2,2,2,2,2,2,
2,2,2,2,2,2,2,2,2,2,2,2,2,2,2,2,2,2,2,2,2,2,2,2,2,2,2,2,2,2,2,2,2,2,2,2,
2,2,2,2,2,2,2,2,2,4),(-0.801433111655479,-0.775159245849183,-0.754653621656624,
-0.751639129200467,-0.749827706159005,-0.748428132005271,-0.746917033744593,
-0.744515779544564,-0.736604867850778,-0.723625824496955,-0.68635394912236,
-0.683669172705429,-0.674080726758402,-0.672439025902231,-0.671441781763254,
-0.670663342698426,-0.669781751618357,-0.668261822573895,-0.661942496006328,
-0.649581857774969,-0.618223829352296,-0.60925925728251,-0.598150562812303,
-0.595363667354653,-0.593750687981787,-0.592381382022701,-0.59071155589933,
-0.587584360946739,-0.568282944182112,-0.532146905883789,-0.518744541593491,
-0.516756145412135,-0.51577527442042,-0.515000008141656,-0.514096530145747,
-0.512477249976737,-0.504719407655079,-0.460449677449668,-0.454761500524851,
-0.442643609743187,-0.440030185246532,-0.43832079227486,-0.43693641524014,
-0.435350164972444,-0.432609448213555,-0.42085335974348,-0.376363467348406,
-0.363057677502036,-0.361072369490632,-0.360092092164516,-0.359316839800562,
-0.358412854720092,-0.356791360491892,-0.348998186687032,-0.304754729938819,
-0.299025867806436,-0.286952586347072,-0.284342114852897,-0.282633597265193,
-0.281249226451485,-0.281245579387401,-0.281241952243014,-0.281238345312432,
-0.281234758432733,-0.281231191439533,-0.281227644172117,-0.281224116479174,
-0.281220608194223,-0.281217119159661,-0.279649882043694,-0.276976487620036,
-0.273714566257554,-0.267056618791725,-0.221725854512607,-0.218552941149592,
-0.207225331694529,-0.20533928083146,-0.204366423002644,-0.203591471213309,
-0.202681383243968,-0.201032595909647,-0.192895113711643,-0.174371873182415,
-0.143101921734939,-0.131233224080841,-0.128636337198476,-0.126931692005924,
-0.125547106322859,-0.124242488570711,-0.121927955135659,-0.11437317444251,
-0.102135049643601,-0.0876110376321648,-0.0538191250905355,-0.0503915729741181,
-0.0491297206439079,-0.0483872992140738,-0.0475974243730106,-0.0465074923170961,
-0.043932577175537,-0.0403310696103786,-0.000460210966472357),
 .UNSPECIFIED.);
#181=B_SPLINE_CURVE_WITH_KNOTS('',3,(#13358,#13359,#13360,#13361,#13362,
#13363,#13364,#13365,#13366,#13367,#13368,#13369,#13370,#13371,#13372,#13373,
#13374,#13375,#13376,#13377,#13378,#13379,#13380,#13381,#13382,#13383,#13384,
#13385,#13386,#13387,#13388,#13389,#13390,#13391,#13392,#13393,#13394,#13395,
#13396,#13397,#13398,#13399,#13400,#13401,#13402,#13403,#13404,#13405,#13406,
#13407),.UNSPECIFIED.,.F.,.F.,(4,2,2,2,2,2,2,2,2,2,2,2,2,2,2,2,2,2,2,2,
2,2,2,2,4),(-1.96102705992237,-1.94412017883534,-1.93679141301454,-1.93448028336829,
-1.93290767593673,-1.93160159451574,-1.9303582798539,-1.92873284212444,
-1.9258896905923,-1.91409267225893,-1.90663976279395,-1.89712543469352,
-1.86488877597605,-1.85616304049253,-1.85495512329353,-1.85387317308645,
-1.85308518461179,-1.85234141434389,-1.85107051574839,-1.84757984900415,
-1.82011283268145,-1.79749119233811,-1.78650204388423,-1.78183577529276,
-1.78180985311435),.UNSPECIFIED.);
#182=B_SPLINE_CURVE_WITH_KNOTS('',3,(#13408,#13409,#13410,#13411,#13412,
#13413,#13414,#13415,#13416,#13417,#13418,#13419,#13420,#13421,#13422,#13423,
#13424,#13425,#13426,#13427,#13428,#13429,#13430,#13431,#13432,#13433,#13434,
#13435,#13436,#13437,#13438,#13439,#13440,#13441,#13442,#13443,#13444,#13445,
#13446,#13447,#13448,#13449,#13450,#13451,#13452,#13453,#13454,#13455,#13456,
#13457,#13458,#13459,#13460,#13461,#13462,#13463,#13464,#13465,#13466,#13467,
#13468,#13469,#13470,#13471,#13472,#13473,#13474,#13475,#13476,#13477,#13478,
#13479,#13480,#13481,#13482,#13483,#13484,#13485,#13486,#13487,#13488,#13489,
#13490,#13491,#13492,#13493,#13494,#13495,#13496,#13497,#13498,#13499,#13500,
#13501,#13502,#13503,#13504,#13505,#13506,#13507,#13508,#13509,#13510,#13511,
#13512,#13513,#13514,#13515,#13516,#13517,#13518,#13519,#13520,#13521,#13522,
#13523,#13524,#13525,#13526,#13527,#13528,#13529,#13530,#13531,#13532,#13533,
#13534,#13535,#13536,#13537,#13538,#13539,#13540,#13541,#13542,#13543,#13544,
#13545,#13546,#13547,#13548,#13549,#13550,#13551,#13552,#13553,#13554,#13555,
#13556,#13557,#13558,#13559,#13560,#13561,#13562,#13563,#13564,#13565,#13566,
#13567,#13568,#13569,#13570,#13571,#13572,#13573,#13574,#13575,#13576,#13577,
#13578,#13579,#13580,#13581,#13582,#13583,#13584,#13585,#13586,#13587,#13588,
#13589,#13590,#13591,#13592,#13593,#13594,#13595,#13596,#13597,#13598,#13599,
#13600,#13601,#13602,#13603,#13604,#13605,#13606,#13607,#13608,#13609,#13610,
#13611,#13612,#13613,#13614,#13615,#13616,#13617,#13618,#13619,#13620,#13621,
#13622,#13623,#13624,#13625,#13626,#13627,#13628,#13629,#13630,#13631,#13632,
#13633,#13634,#13635,#13636,#13637,#13638,#13639,#13640,#13641,#13642,#13643,
#13644,#13645,#13646,#13647,#13648,#13649,#13650,#13651,#13652,#13653,#13654,
#13655,#13656,#13657,#13658,#13659,#13660,#13661,#13662,#13663,#13664,#13665,
#13666,#13667,#13668,#13669,#13670,#13671,#13672,#13673,#13674,#13675,#13676,
#13677,#13678,#13679,#13680,#13681,#13682,#13683,#13684,#13685,#13686,#13687,
#13688,#13689,#13690,#13691,#13692,#13693,#13694,#13695,#13696,#13697,#13698,
#13699,#13700,#13701,#13702,#13703,#13704,#13705,#13706,#13707,#13708,#13709,
#13710,#13711,#13712,#13713,#13714,#13715,#13716,#13717,#13718,#13719,#13720,
#13721,#13722,#13723,#13724,#13725,#13726,#13727,#13728,#13729,#13730,#13731,
#13732,#13733,#13734,#13735,#13736,#13737,#13738,#13739,#13740,#13741,#13742,
#13743,#13744,#13745,#13746,#13747,#13748,#13749,#13750,#13751,#13752,#13753,
#13754,#13755,#13756,#13757,#13758,#13759,#13760,#13761,#13762,#13763,#13764,
#13765,#13766,#13767,#13768,#13769,#13770,#13771,#13772,#13773,#13774,#13775,
#13776,#13777,#13778,#13779,#13780,#13781,#13782,#13783,#13784,#13785,#13786,
#13787,#13788,#13789,#13790,#13791,#13792,#13793,#13794,#13795,#13796,#13797,
#13798,#13799),.UNSPECIFIED.,.F.,.F.,(4,2,2,2,2,2,2,2,2,2,2,2,2,2,2,2,2,
2,2,2,2,2,2,2,2,2,2,2,2,2,2,2,2,2,2,2,2,2,2,2,2,2,2,2,2,2,2,2,2,2,2,2,2,
2,2,2,2,2,2,2,2,2,2,2,2,2,2,2,2,2,2,2,2,2,2,2,2,2,2,2,2,2,2,2,2,2,2,2,2,
2,2,2,2,2,2,2,2,2,2,2,2,2,2,2,2,2,2,2,2,2,2,2,2,2,2,2,2,2,2,2,2,2,2,2,2,
2,2,2,2,2,2,2,2,2,2,2,2,2,2,2,2,2,2,2,2,2,2,2,2,2,2,2,2,2,2,2,2,2,2,2,2,
2,2,2,2,2,2,2,2,2,2,2,2,2,2,2,2,2,2,2,2,2,2,2,2,2,2,2,2,2,2,2,2,2,2,4),
(-1.16050672125936,-1.13658797771447,-1.12325146763907,-1.12040624604766,
-1.11879714613831,-1.11755326941281,-1.11593166924341,-1.11310683508528,
-1.1015440333472,-1.09533917016703,-1.05141500268395,-1.04318894357646,
-1.04154187277803,-1.04063234732588,-1.03985764275991,-1.03888481974403,
-1.03699803944337,-1.02564064794427,-1.01216043658711,-0.981311096955009,
-0.967844709397715,-0.9651434330647,-0.963406854909695,-0.962020152090692,
-0.960452432223601,-0.957796086446112,-0.947157022676203,-0.901820982983431,
-0.89681332168628,-0.887740070346934,-0.886124703940506,-0.885124530860051,
-0.884347469966316,-0.88345706668008,-0.881897726581934,-0.875050001580883,
-0.832241811488523,-0.812639565198644,-0.809646851508131,-0.807841660840296,
-0.806442845716016,-0.804928529580441,-0.802513456431045,-0.794477182880794,
-0.781211689771461,-0.743840597244101,-0.732227967153351,-0.730330709843061,
-0.72935555838399,-0.728580614859418,-0.727672674197026,-0.726033217740437,
-0.71794100239879,-0.673932163862546,-0.667907050424341,-0.656151911367998,
-0.653311071940292,-0.651685627219854,-0.650441615056989,-0.648835662942649,
-0.646005686365083,-0.632921510287751,-0.604650023138001,-0.587407689850453,
-0.576482898555614,-0.574778643868645,-0.573762972623271,-0.572982091572767,
-0.572111002620281,-0.57063855928568,-0.564901965089997,-0.554201216951262,
-0.510334353318773,-0.50726942733268,-0.500753020889885,-0.498015224500325,
-0.496267505748658,-0.494879818212073,-0.49331936623797,-0.490695566177447,
-0.480452682402657,-0.434796051841406,-0.430598756339604,-0.42066195834132,
-0.419002917052987,-0.418000489194207,-0.417221333861661,-0.416342687777439,
-0.414836343440348,-0.408691245774602,-0.396841466417074,-0.365235547677384,
-0.345528611545284,-0.342533293469695,-0.340727335627656,-0.339328402285089,
-0.339323857935652,-0.339319352370189,-0.339314885236623,-0.33931045619602,
-0.339306064898714,-0.339301711008387,-0.339297394170184,-0.339293114045987,
-0.339288870311452,-0.339284662631023,-0.339280490664529,-0.339276354092131,
-0.33927225258856,-0.339268185852101,-0.339264153544142,-0.339260155354349,
-0.339256190976604,-0.339252260114969,-0.339248362443475,-0.339244497673467,
-0.339240665514632,-0.339236865653649,-0.339233097789755,-0.339229361650208,
-0.339225656940361,-0.339221983369571,-0.339218340651027,-0.339214728527488,
-0.339211146714534,-0.339207594938659,-0.339204072920932,-0.33920058038965,
-0.339197117075535,-0.33919368272291,-0.339190277075752,-0.339186899854147,
-0.339183550804388,-0.339180229696334,-0.33917693626758,-0.339173670264504,
-0.339171163995327,-0.339168662973366,-0.33916616678394,-0.339163675419185,
-0.339161188874753,-0.339158707143298,-0.339156230204622,-0.339153758026079,
-0.339151290602902,-0.339148827921157,-0.339146369982959,-0.339143916767275,
-0.339141468250363,-0.339139024431141,-0.339136585286716,-0.339134150817317,
-0.339131721004108,-0.339129295813795,-0.339126875245179,-0.339124459281576,
-0.339122047936093,-0.33911964119357,-0.3391172390237,-0.339114841390878,
-0.339112448302961,-0.339110059760955,-0.33910767572495,-0.339105296186166,
-0.339102921133349,-0.339100550561894,-0.337545801628347,-0.3349011609442,
-0.331699631582162,-0.325211962534818,-0.280588976144251,-0.276869237098302,
-0.265098134172531,-0.263194700597936,-0.262218225312468,-0.261443198504544,
-0.260536279385063,-0.258901495635772,-0.251003341027479,-0.20685139100601,
-0.201057954306407,-0.189047947845654,-0.186441624012335,-0.184734327430287,
-0.183349953970372,-0.183338368875809,-0.183327191713962,-0.183316408267552,
-0.183306003692731,-0.183295963745638,-0.183286276051788,-0.183276928768914,
-0.183267906941564,-0.183259198518953,-0.181669373545164,-0.179852073555682),
 .UNSPECIFIED.);
#183=B_SPLINE_CURVE_WITH_KNOTS('',3,(#13804,#13805,#13806,#13807,#13808,
#13809,#13810,#13811,#13812,#13813,#13814,#13815,#13816,#13817,#13818,#13819,
#13820,#13821,#13822,#13823,#13824,#13825,#13826,#13827,#13828,#13829,#13830,
#13831,#13832,#13833,#13834,#13835,#13836,#13837,#13838,#13839,#13840,#13841,
#13842,#13843,#13844,#13845,#13846,#13847,#13848,#13849,#13850,#13851,#13852,
#13853,#13854,#13855,#13856,#13857,#13858,#13859,#13860,#13861,#13862,#13863,
#13864,#13865,#13866,#13867,#13868,#13869,#13870,#13871,#13872,#13873,#13874,
#13875,#13876,#13877,#13878,#13879,#13880,#13881,#13882,#13883,#13884,#13885,
#13886,#13887,#13888,#13889,#13890,#13891,#13892,#13893,#13894,#13895,#13896,
#13897,#13898,#13899,#13900,#13901,#13902,#13903,#13904,#13905,#13906,#13907,
#13908,#13909,#13910,#13911,#13912,#13913,#13914,#13915,#13916,#13917,#13918,
#13919,#13920,#13921,#13922,#13923,#13924,#13925,#13926,#13927,#13928,#13929,
#13930,#13931,#13932,#13933,#13934,#13935,#13936,#13937,#13938,#13939,#13940,
#13941,#13942,#13943,#13944,#13945,#13946,#13947,#13948,#13949,#13950,#13951,
#13952,#13953,#13954,#13955,#13956,#13957,#13958,#13959,#13960,#13961,#13962,
#13963,#13964,#13965,#13966,#13967,#13968,#13969,#13970,#13971,#13972,#13973,
#13974,#13975,#13976,#13977,#13978,#13979,#13980,#13981,#13982,#13983,#13984,
#13985,#13986,#13987,#13988,#13989,#13990,#13991,#13992,#13993,#13994,#13995,
#13996,#13997,#13998,#13999,#14000,#14001,#14002,#14003,#14004,#14005,#14006,
#14007,#14008,#14009,#14010,#14011,#14012,#14013,#14014,#14015,#14016,#14017,
#14018,#14019,#14020,#14021,#14022,#14023,#14024,#14025,#14026,#14027,#14028,
#14029,#14030,#14031,#14032,#14033,#14034,#14035,#14036,#14037,#14038,#14039,
#14040,#14041,#14042,#14043,#14044,#14045,#14046,#14047,#14048,#14049),
 .UNSPECIFIED.,.F.,.F.,(4,2,2,2,2,2,2,2,2,2,2,2,2,2,2,2,2,2,2,2,2,2,2,2,
2,2,2,2,2,2,2,2,2,2,2,2,2,2,2,2,2,2,2,2,2,2,2,2,2,2,2,2,2,2,2,2,2,2,2,2,
2,2,2,2,2,2,2,2,2,2,2,2,2,2,2,2,2,2,2,2,2,2,2,2,2,2,2,2,2,2,2,2,2,2,2,2,
2,2,2,2,2,2,2,2,2,2,2,2,2,2,2,2,2,2,2,2,2,2,2,2,2,2,4),(-1.78170741026359,
-1.77139420245484,-1.76332743792697,-1.76168306777715,-1.7607741496317,
-1.75999942313482,-1.75902587233313,-1.75713561890463,-1.74569030602177,
-1.74260851916196,-1.69734956609914,-1.69070338081476,-1.68744577678322,
-1.68477757017397,-1.68321072749998,-1.68320722821,-1.68320370964983,-1.6832001716673,
-1.68319661410376,-1.68319303680128,-1.68318943959573,-1.6831858223304,
-1.68318218484626,-1.68317852720448,-1.68179464445203,-1.68008686597183,
-1.67747775836826,-1.66541595601263,-1.65967617399006,-1.61542964749078,
-1.60762790099442,-1.60600618574291,-1.60510230907244,-1.60432728938023,
-1.60334749069679,-1.60136374784442,-1.58809008197448,-1.5436734689132,
-1.53186727292633,-1.52912347545126,-1.52753678829489,-1.52615282920023,
-1.52444497983836,-1.52183580733392,-1.5097745337863,-1.50403334230908,
-1.45978506202724,-1.45198194850415,-1.45036008520169,-1.44945614518642,
-1.4486810829916,-1.44770124572058,-1.44571747422532,-1.43244557578626,
-1.38803077178286,-1.37621776566786,-1.37347337658652,-1.37188650374007,
-1.37050247559103,-1.36879466040507,-1.36618576215494,-1.3541299962284,
-1.34838292660021,-1.30413594753992,-1.29632765893282,-1.29470541546936,
-1.29380136148975,-1.29302626189234,-1.29204645466502,-1.29006299659631,
-1.27680317922937,-1.2324077662769,-1.22056285708051,-1.21781609678637,
-1.21622864658763,-1.21484458601124,-1.21313733586261,-1.21053042536963,
-1.19850527800456,-1.19272976835506,-1.14849934940822,-1.14066682387664,
-1.13904304144341,-1.13813862083536,-1.13736350909541,-1.13638407377269,
-1.13440263230767,-1.1212058383141,-1.07691420359242,-1.06491541041669,
-1.06215772345684,-1.06056781406325,-1.05918389020121,-1.05747972968807,
-1.0548829504671,-1.04300428626409,-1.03568456526173,-0.991982193092347,
-0.984910625319681,-0.983335839248477,-0.982442119419145,-0.981665681534951,
-0.98067089988623,-0.978612390404106,-0.975904803983002,-0.947661542595715,
-0.913237037660929,-0.907979562174086,-0.905860392343265,-0.904554998790264,
-0.903142774435695,-0.901222247930651,-0.896796482759925,-0.877935781650044,
-0.851356180149381,-0.830191596028536,-0.828075088674039,-0.827068998675036,
-0.826291439579715,-0.825405024502319,-0.823863323342374,-0.817256504014559,
-0.801433111655479),.UNSPECIFIED.);
#184=B_SPLINE_CURVE_WITH_KNOTS('',3,(#14051,#14052,#14053,#14054,#14055,
#14056,#14057,#14058,#14059,#14060,#14061,#14062,#14063,#14064,#14065,#14066,
#14067,#14068,#14069,#14070,#14071,#14072,#14073,#14074,#14075,#14076,#14077,
#14078,#14079,#14080,#14081,#14082,#14083,#14084,#14085,#14086,#14087,#14088,
#14089,#14090,#14091,#14092,#14093,#14094,#14095,#14096,#14097,#14098,#14099,
#14100),.UNSPECIFIED.,.F.,.F.,(4,2,2,2,2,2,2,2,2,2,2,2,2,2,2,2,2,2,2,2,
2,2,2,2,4),(-0.179852073555682,-0.178878435810792,-0.175450539953574,-0.168316256847422,
-0.14771672789062,-0.111178057748267,-0.108072550368483,-0.106861072900725,
-0.106128620433403,-0.105332032945858,-0.104203869302599,-0.101397602678173,
-0.0892071044472608,-0.0586364436391121,-0.0496241211686591,-0.0456935464141843,
-0.0334250198293235,-0.030800780394571,-0.0290879388733611,-0.0277031758227639,
-0.0264000299616105,-0.0248463918548199,-0.0225820312570058,-0.0156371952265505,
-0.000459509676940365),.UNSPECIFIED.);
#185=B_SPLINE_CURVE_WITH_KNOTS('',3,(#14101,#14102,#14103,#14104,#14105,
#14106,#14107,#14108,#14109,#14110,#14111,#14112,#14113,#14114,#14115,#14116,
#14117,#14118,#14119,#14120,#14121,#14122,#14123,#14124,#14125,#14126,#14127,
#14128,#14129,#14130,#14131,#14132,#14133,#14134,#14135,#14136,#14137,#14138,
#14139,#14140,#14141,#14142,#14143,#14144,#14145,#14146,#14147,#14148,#14149,
#14150,#14151,#14152,#14153,#14154,#14155,#14156,#14157,#14158,#14159,#14160,
#14161,#14162,#14163,#14164,#14165,#14166,#14167,#14168,#14169,#14170,#14171,
#14172,#14173,#14174,#14175,#14176,#14177,#14178,#14179,#14180,#14181,#14182,
#14183,#14184,#14185,#14186,#14187,#14188,#14189,#14190,#14191,#14192,#14193,
#14194,#14195,#14196,#14197,#14198,#14199,#14200,#14201,#14202,#14203,#14204,
#14205,#14206,#14207,#14208,#14209,#14210,#14211,#14212,#14213,#14214,#14215,
#14216,#14217,#14218,#14219,#14220,#14221,#14222,#14223,#14224,#14225,#14226,
#14227,#14228,#14229,#14230,#14231,#14232,#14233,#14234,#14235,#14236,#14237,
#14238,#14239,#14240,#14241,#14242,#14243,#14244,#14245,#14246,#14247,#14248,
#14249,#14250,#14251,#14252,#14253,#14254,#14255,#14256,#14257,#14258,#14259,
#14260,#14261,#14262,#14263,#14264,#14265,#14266,#14267,#14268,#14269,#14270,
#14271,#14272,#14273,#14274,#14275,#14276,#14277,#14278,#14279,#14280,#14281,
#14282,#14283,#14284,#14285,#14286,#14287,#14288,#14289,#14290,#14291,#14292,
#14293,#14294,#14295,#14296,#14297,#14298,#14299,#14300),.UNSPECIFIED.,
 .F.,.F.,(4,2,2,2,2,2,2,2,2,2,2,2,2,2,2,2,2,2,2,2,2,2,2,2,2,2,2,2,2,2,2,
2,2,2,2,2,2,2,2,2,2,2,2,2,2,2,2,2,2,2,2,2,2,2,2,2,2,2,2,2,2,2,2,2,2,2,2,
2,2,2,2,2,2,2,2,2,2,2,2,2,2,2,2,2,2,2,2,2,2,2,2,2,2,2,2,2,2,2,2,4),(-1.96069987759182,
-1.91845884062044,-1.91490970624029,-1.91236466372798,-1.91128050011752,
-1.91049220108497,-1.90974918646458,-1.90848186321831,-1.90501377579469,
-1.87177032517842,-1.8582009874233,-1.84507642640989,-1.83712775120393,
-1.83477211187913,-1.8334660218736,-1.83222279387898,-1.8305981325039,-1.82775803702758,
-1.81599755965749,-1.80998148156486,-1.76597016925142,-1.75789691373428,
-1.75625265022867,-1.75534397892635,-1.75456958037236,-1.75359660568952,
-1.75170796113064,-1.74028926353391,-1.73718781016408,-1.6919285709932,
-1.68528011084203,-1.68202205084216,-1.67935006559657,-1.67778456422658,
-1.67778108423104,-1.6777775849879,-1.67777406632914,-1.67777052811106,
-1.67776697017973,-1.67776339236119,-1.67775979449114,-1.67775617640286,
-1.6777525379283,-1.67774887911552,-1.67636536954792,-1.67465562350651,
-1.67203899064432,-1.6598561591188,-1.6542247615872,-1.60997465978654,-1.60220583877028,
-1.60058658823094,-1.59968347174851,-1.59890872933706,-1.59792881529424,
-1.59594332484397,-1.5825994599447,-1.53811128811494,-1.52643687298707,
-1.5237032454324,-1.52211919470659,-1.52073560529017,-1.5190257293684,-1.51640883951757,
-1.50422368749246,-1.49859343623657,-1.45433981757096,-1.44657185353636,
-1.44495259156031,-1.44404944182408,-1.44327465430576,-1.44229466193643,
-1.44030894315071,-1.42696074276319,-1.38246369429336,-1.3707975735219,
-1.36806443776634,-1.36648044043244,-1.36509675958176,-1.36338659265735,
-1.3607689252673,-1.34857373642418,-1.34295150844639,-1.29868945320575,
-1.290928442227,-1.2893095426576,-1.2884064412267,-1.28763160022206,-1.28665141838019,
-1.28466491682819,-1.27129536869087,-1.22675887188467,-1.21514368919964,
-1.2124141293189,-1.21083086477891,-1.20944702446029,-1.20773562856479,
-1.20511415254834,-1.19287010978845,-1.15986353876316),.UNSPECIFIED.);
#186=B_SPLINE_CURVE_WITH_KNOTS('',3,(#14306,#14307,#14308,#14309,#14310,
#14311,#14312,#14313,#14314,#14315,#14316,#14317,#14318,#14319,#14320,#14321,
#14322,#14323,#14324,#14325,#14326,#14327,#14328,#14329,#14330,#14331,#14332,
#14333,#14334,#14335,#14336,#14337,#14338,#14339,#14340,#14341,#14342,#14343,
#14344,#14345,#14346,#14347,#14348,#14349,#14350,#14351,#14352,#14353,#14354,
#14355,#14356,#14357,#14358,#14359,#14360,#14361,#14362,#14363,#14364,#14365,
#14366,#14367,#14368,#14369,#14370,#14371,#14372,#14373,#14374,#14375,#14376,
#14377,#14378,#14379,#14380,#14381,#14382,#14383,#14384,#14385,#14386,#14387,
#14388,#14389,#14390,#14391,#14392,#14393,#14394,#14395,#14396,#14397,#14398,
#14399,#14400,#14401,#14402,#14403,#14404,#14405,#14406,#14407,#14408,#14409,
#14410,#14411,#14412,#14413,#14414,#14415,#14416,#14417,#14418,#14419,#14420,
#14421,#14422,#14423,#14424,#14425,#14426,#14427,#14428,#14429,#14430,#14431,
#14432,#14433,#14434,#14435,#14436,#14437,#14438,#14439,#14440,#14441,#14442,
#14443,#14444,#14445,#14446,#14447,#14448,#14449,#14450,#14451,#14452,#14453,
#14454,#14455,#14456,#14457,#14458,#14459,#14460,#14461,#14462,#14463,#14464,
#14465,#14466,#14467,#14468,#14469,#14470,#14471,#14472,#14473,#14474,#14475,
#14476,#14477,#14478,#14479,#14480,#14481,#14482,#14483,#14484,#14485,#14486,
#14487,#14488,#14489,#14490,#14491,#14492,#14493,#14494,#14495,#14496,#14497,
#14498,#14499,#14500,#14501,#14502,#14503),.UNSPECIFIED.,.F.,.F.,(4,2,2,
2,2,2,2,2,2,2,2,2,2,2,2,2,2,2,2,2,2,2,2,2,2,2,2,2,2,2,2,2,2,2,2,2,2,2,2,
2,2,2,2,2,2,2,2,2,2,2,2,2,2,2,2,2,2,2,2,2,2,2,2,2,2,2,2,2,2,2,2,2,2,2,2,
2,2,2,2,2,2,2,2,2,2,2,2,2,2,2,2,2,2,2,2,2,2,2,4),(-0.801736014421406,-0.799581811946282,
-0.786209666041104,-0.74936065287489,-0.746990920996527,-0.737255478959455,
-0.735606057239272,-0.734606350787257,-0.733827381547235,-0.732946759298924,
-0.731432067556231,-0.725184478761221,-0.713037220202634,-0.681652814287474,
-0.662139640151576,-0.65914878586409,-0.657343928333994,-0.655944900135632,
-0.654429880668577,-0.652012656973972,-0.643959550155184,-0.630655923318393,
-0.593444004693946,-0.581745016771518,-0.579844087335122,-0.578868014973784,
-0.578092843662842,-0.577185205425138,-0.575547724460788,-0.567493632303464,
-0.523440945880881,-0.5173900401822,-0.505666078908615,-0.502827366741388,
-0.501202184643843,-0.499957868908011,-0.498350926083002,-0.495517455474805,
-0.482384326914722,-0.453918733901765,-0.444577110488416,-0.436139833649767,
-0.425951636746667,-0.424280237635206,-0.423274079479185,-0.422494329466205,
-0.421617580490128,-0.420120225711973,-0.414088640926143,-0.402564846887454,
-0.371379915070074,-0.350845008934168,-0.347828888464038,-0.346016659672986,
-0.344616564658634,-0.343105004868396,-0.340703233739555,-0.332792583503428,
-0.319815939748242,-0.276376738732361,-0.275623251472852,-0.273817368571057,
-0.269447399524127,-0.268055445688625,-0.267202113744547,-0.266415215595033,
-0.265343097293166,-0.263029103693493,-0.245890571718042,-0.203821008599721,
-0.198910163307287,-0.196251849981033,-0.192581081170869,-0.190763692728898,
-0.18944754718031,-0.188041564262708,-0.186198210194599,-0.182175397196218,
-0.176782914666108,-0.163267578331553,-0.141761351985546,-0.11492981288647,
-0.11285975016619,-0.11186249878683,-0.111085596799273,-0.110192985811116,
-0.108624087553022,-0.101756566331568,-0.0819348749466729,-0.0640483815359052,
-0.0396378439030753,-0.0365365080531776,-0.0346993352740578,-0.0332951743186159,
-0.0319991340209431,-0.0305265880276274,-0.0284625165163476,-0.0209035907064299,
-0.000459615136305543),.UNSPECIFIED.);
#187=B_SPLINE_CURVE_WITH_KNOTS('',3,(#14504,#14505,#14506,#14507,#14508,
#14509,#14510,#14511,#14512,#14513,#14514,#14515,#14516,#14517,#14518,#14519,
#14520,#14521,#14522,#14523,#14524,#14525,#14526,#14527,#14528,#14529,#14530,
#14531,#14532,#14533,#14534,#14535,#14536,#14537,#14538,#14539,#14540,#14541,
#14542,#14543,#14544,#14545),.UNSPECIFIED.,.F.,.F.,(4,2,2,2,2,2,2,2,2,2,
2,2,2,2,2,2,2,2,2,2,4),(-1.96080348278997,-1.92112421592769,-1.91900621949408,
-1.91779070717829,-1.91670329693965,-1.91591411202519,-1.91517143078537,
-1.91390718425261,-1.91046181988859,-1.87688943572253,-1.85901222475556,
-1.8488083647261,-1.84221430945411,-1.84001055546783,-1.83871197973006,
-1.83732281946126,-1.83556117019383,-1.83277779482363,-1.81793256979077,
-1.78965448236495,-1.78170741026359),.UNSPECIFIED.);
#188=B_SPLINE_CURVE_WITH_KNOTS('',3,(#14546,#14547,#14548,#14549,#14550,
#14551,#14552,#14553,#14554,#14555,#14556,#14557,#14558,#14559,#14560,#14561,
#14562,#14563,#14564,#14565,#14566,#14567,#14568,#14569,#14570,#14571,#14572,
#14573,#14574,#14575,#14576,#14577,#14578,#14579,#14580,#14581,#14582,#14583,
#14584,#14585,#14586,#14587,#14588,#14589,#14590,#14591,#14592,#14593,#14594,
#14595,#14596,#14597,#14598,#14599,#14600,#14601,#14602,#14603,#14604,#14605,
#14606,#14607,#14608,#14609,#14610,#14611,#14612,#14613,#14614,#14615,#14616,
#14617,#14618,#14619,#14620,#14621,#14622,#14623,#14624,#14625,#14626,#14627,
#14628,#14629,#14630,#14631,#14632,#14633,#14634,#14635,#14636,#14637,#14638,
#14639,#14640,#14641,#14642,#14643,#14644,#14645,#14646,#14647,#14648,#14649,
#14650,#14651,#14652,#14653,#14654,#14655,#14656,#14657,#14658,#14659,#14660,
#14661,#14662,#14663,#14664,#14665,#14666,#14667,#14668,#14669,#14670,#14671,
#14672,#14673,#14674,#14675,#14676,#14677,#14678,#14679,#14680,#14681,#14682,
#14683,#14684,#14685,#14686,#14687,#14688,#14689,#14690,#14691,#14692,#14693,
#14694,#14695,#14696,#14697,#14698,#14699,#14700,#14701,#14702,#14703,#14704,
#14705,#14706,#14707,#14708,#14709,#14710,#14711,#14712,#14713,#14714,#14715,
#14716,#14717,#14718,#14719,#14720,#14721,#14722,#14723,#14724,#14725,#14726,
#14727,#14728,#14729,#14730,#14731,#14732,#14733,#14734,#14735,#14736,#14737,
#14738,#14739,#14740,#14741,#14742,#14743,#14744,#14745,#14746,#14747,#14748,
#14749,#14750,#14751,#14752,#14753,#14754,#14755,#14756,#14757,#14758,#14759,
#14760,#14761,#14762,#14763,#14764,#14765,#14766,#14767,#14768,#14769,#14770,
#14771,#14772,#14773,#14774,#14775,#14776,#14777,#14778,#14779,#14780,#14781,
#14782,#14783,#14784,#14785,#14786,#14787,#14788,#14789,#14790,#14791,#14792,
#14793,#14794,#14795,#14796,#14797,#14798,#14799,#14800,#14801),
 .UNSPECIFIED.,.F.,.F.,(4,2,2,2,2,2,2,2,2,2,2,2,2,2,2,2,2,2,2,2,2,2,2,2,
2,2,2,2,2,2,2,2,2,2,2,2,2,2,2,2,2,2,2,2,2,2,2,2,2,2,2,2,2,2,2,2,2,2,2,2,
2,2,2,2,2,2,2,2,2,2,2,2,2,2,2,2,2,2,2,2,2,2,2,2,2,2,2,2,2,2,2,2,2,2,2,2,
2,2,2,2,2,2,2,2,2,2,2,2,2,2,2,2,2,2,2,2,2,2,2,2,2,2,2,2,2,2,2,4),(-1.15986353876316,
-1.15495867850168,-1.14175904705784,-1.1351629966844,-1.13362261718722,
-1.13273677987422,-1.13195960835742,-1.13095388491762,-1.12883766586569,
-1.10740677657844,-1.08131814215635,-1.06231067802686,-1.05786699876735,
-1.05594391764032,-1.05453179125116,-1.05322787780649,-1.0511142389345,
-1.04588581019901,-1.0104321745147,-0.980666401933017,-0.978460612453208,
-0.977448638450662,-0.976668587876089,-0.975796190960301,-0.97431663989005,
-0.968490849648887,-0.957541774780541,-0.936340089929828,-0.905229067644997,
-0.901803915865218,-0.900049503700995,-0.898661637452001,-0.89710637963854,
-0.894504186833417,-0.884507856564803,-0.839507550004001,-0.836515338582123,
-0.834012864181881,-0.824432458371408,-0.822791485487271,-0.821794611158168,
-0.821016417682501,-0.820135068691051,-0.818615486547449,-0.812296704528674,
-0.799936473572604,-0.76856760039765,-0.759601643664272,-0.748500022717946,
-0.745714253073186,-0.7441018269715,-0.742732935527723,-0.74106354982356,
-0.737936995467345,-0.718634870499409,-0.68250151589321,-0.669094006890376,
-0.667105849646672,-0.666125202821074,-0.665350168083612,-0.664447035633299,
-0.662828574539928,-0.65507860489707,-0.610820297515902,-0.605211207037558,
-0.593002979424579,-0.59038394479401,-0.588673086537345,-0.587288988968702,
-0.585704671020448,-0.582971379341359,-0.571311078773968,-0.52676947647019,
-0.513406452537092,-0.511419672278857,-0.510439275763811,-0.509664229016491,
-0.508760841517006,-0.507141322659481,-0.499374944175718,-0.455127672194173,
-0.449500261110734,-0.437311781993052,-0.434694000353402,-0.432983490301602,
-0.431599362279075,-0.430014666872687,-0.427279857768263,-0.4155996636971,
-0.371069940060048,-0.357714094278084,-0.355727480084304,-0.354747091231235,
-0.35397201418579,-0.353068549603149,-0.351448788432619,-0.34367927845436,
-0.299432310379321,-0.293801497053899,-0.281616019753565,-0.278998361741958,
-0.27728785033777,-0.275903666698296,-0.275899970384863,-0.275896294307179,
-0.275892638723789,-0.275889003472613,-0.275885388368658,-0.275881793268624,
-0.275878218012326,-0.275874662428703,-0.275871126379079,-0.275867609688949,
-0.27430115952195,-0.27163961612077,-0.268388698231828,-0.261761342997514,
-0.216576682819282,-0.214178274703862,-0.210534877081703,-0.201660088246841,
-0.200055481560891,-0.199058586684916,-0.198281891664026,-0.197389451716405,
-0.195852238546242,-0.189244216540455,-0.179585755313572),.UNSPECIFIED.);
#189=B_SPLINE_CURVE_WITH_KNOTS('',3,(#14806,#14807,#14808,#14809,#14810,
#14811,#14812,#14813,#14814,#14815,#14816,#14817,#14818,#14819,#14820,#14821,
#14822,#14823,#14824,#14825,#14826,#14827,#14828,#14829,#14830,#14831,#14832,
#14833,#14834,#14835,#14836,#14837,#14838,#14839,#14840,#14841,#14842,#14843,
#14844,#14845,#14846,#14847,#14848,#14849,#14850,#14851,#14852,#14853,#14854,
#14855,#14856,#14857,#14858,#14859,#14860,#14861,#14862,#14863,#14864,#14865,
#14866,#14867,#14868,#14869,#14870,#14871,#14872,#14873,#14874,#14875,#14876,
#14877,#14878,#14879,#14880,#14881,#14882,#14883,#14884,#14885,#14886,#14887,
#14888,#14889,#14890,#14891,#14892,#14893,#14894,#14895,#14896,#14897,#14898,
#14899,#14900,#14901,#14902,#14903,#14904,#14905,#14906,#14907,#14908,#14909,
#14910,#14911,#14912,#14913,#14914,#14915,#14916,#14917,#14918,#14919,#14920,
#14921,#14922,#14923,#14924,#14925,#14926,#14927,#14928,#14929,#14930,#14931,
#14932,#14933,#14934,#14935,#14936,#14937,#14938,#14939,#14940,#14941,#14942,
#14943,#14944,#14945,#14946,#14947,#14948,#14949,#14950,#14951,#14952,#14953,
#14954,#14955,#14956,#14957,#14958,#14959,#14960,#14961,#14962,#14963,#14964,
#14965,#14966,#14967,#14968,#14969,#14970,#14971,#14972,#14973,#14974,#14975,
#14976,#14977,#14978,#14979,#14980,#14981,#14982,#14983,#14984,#14985,#14986,
#14987,#14988,#14989,#14990,#14991,#14992,#14993,#14994,#14995,#14996,#14997,
#14998,#14999,#15000,#15001,#15002,#15003,#15004,#15005,#15006,#15007,#15008,
#15009,#15010,#15011,#15012,#15013,#15014,#15015,#15016,#15017,#15018,#15019,
#15020,#15021,#15022,#15023,#15024,#15025,#15026,#15027,#15028,#15029,#15030,
#15031,#15032,#15033,#15034,#15035,#15036,#15037,#15038,#15039,#15040,#15041,
#15042,#15043,#15044,#15045,#15046,#15047),.UNSPECIFIED.,.F.,.F.,(4,2,2,
2,2,2,2,2,2,2,2,2,2,2,2,2,2,2,2,2,2,2,2,2,2,2,2,2,2,2,2,2,2,2,2,2,2,2,2,
2,2,2,2,2,2,2,2,2,2,2,2,2,2,2,2,2,2,2,2,2,2,2,2,2,2,2,2,2,2,2,2,2,2,2,2,
2,2,2,2,2,2,2,2,2,2,2,2,2,2,2,2,2,2,2,2,2,2,2,2,2,2,2,2,2,2,2,2,2,2,2,2,
2,2,2,2,2,2,2,2,2,4),(-1.78190244653125,-1.77200868256019,-1.75328004368102,
-1.74887061521904,-1.74695295631717,-1.74554123240277,-1.74423516243715,
-1.74211234313619,-1.73683348299684,-1.70421673361218,-1.68584745493587,
-1.67588936352327,-1.67225964458583,-1.67047911262385,-1.66904226233087,
-1.66822238692452,-1.66744721360907,-1.66646723515569,-1.66448317552644,
-1.6512092584759,-1.60678788985221,-1.59497347602076,-1.59222871393679,
-1.59064161815708,-1.5892573912631,-1.58754932530048,-1.58494003366211,
-1.57288225332685,-1.56713461767231,-1.52288112234591,-1.51507193410924,
-1.51344947154688,-1.51254529093412,-1.51177007997497,-1.51079012839565,
-1.50880636641984,-1.49554405586124,-1.45931070509532,-1.44649224817082,
-1.43865066013505,-1.43625682861186,-1.43474726379943,-1.43334695256219,
-1.43153152701537,-1.42850368046637,-1.407494623618,-1.37664021955004,-1.36521899408719,
-1.35922464044709,-1.35773055345891,-1.35685465848211,-1.35607494105831,
-1.35506789137943,-1.35339306487235,-1.34312904726704,-1.32725767432596,
-1.30297643698827,-1.29064042446784,-1.28301303048465,-1.28064293414308,
-1.27913854391298,-1.27773623516422,-1.27590853323477,-1.27283881580251,
-1.25004440996076,-1.22063140048047,-1.20950557322381,-1.20361609010587,
-1.20213064080079,-1.2012566380236,-1.20047642961679,-1.19946591263889,
-1.19777935925272,-1.18727064336203,-1.17162391919845,-1.1473553115595,
-1.12876414179781,-1.12566291869733,-1.12399844276655,-1.12262913782025,
-1.1210110117645,-1.11820235209479,-1.10683968477102,-1.1004529000864,-1.05657106709834,
-1.04826964419452,-1.04661801281888,-1.04570736457408,-1.04493254226705,
-1.04396062104761,-1.04243836183204,-1.03493599535656,-0.996672112128502,
-0.981036614342849,-0.978619059928186,-0.976094644725976,-0.97108996763833,
-0.969012718378032,-0.96771478796018,-0.966295990134023,-0.964339934999445,
-0.959709549548212,-0.939193525411031,-0.904988690061857,-0.902508925466035,
-0.892898127035476,-0.891254952756727,-0.890257116585476,-0.889478405216726,
-0.888596720156414,-0.887077117940799,-0.880766052288347,-0.868431766917954,
-0.837101558379535,-0.817787889837261,-0.814802370709961,-0.81299912476786,
-0.811600390825296,-0.810084736028705,-0.807664431424583,-0.801736014421406),
 .UNSPECIFIED.);
#190=B_SPLINE_CURVE_WITH_KNOTS('',3,(#15049,#15050,#15051,#15052,#15053,
#15054,#15055,#15056,#15057,#15058,#15059,#15060,#15061,#15062,#15063,#15064,
#15065,#15066,#15067,#15068,#15069,#15070,#15071,#15072,#15073,#15074,#15075,
#15076,#15077,#15078,#15079,#15080,#15081,#15082,#15083,#15084,#15085,#15086,
#15087,#15088,#15089,#15090,#15091,#15092,#15093,#15094,#15095,#15096),
 .UNSPECIFIED.,.F.,.F.,(4,2,2,2,2,2,2,2,2,2,2,2,2,2,2,2,2,2,2,2,2,2,2,4),
(-0.179585755313572,-0.175967937818465,-0.145634237770135,-0.136632875108729,
-0.12573674578162,-0.122965633031804,-0.121356158290008,-0.119973254234572,
-0.118650029470105,-0.116080412267979,-0.10589524409011,-0.0871223915043526,
-0.0765752847012227,-0.0608164388935438,-0.0578246341694164,-0.0462515126542455,
-0.0443559436050484,-0.0433812055735334,-0.0426063519953875,-0.0416982405767139,
-0.0407356219690761,-0.0392376733234128,-0.0363880930835168,-0.000460083170512367),
 .UNSPECIFIED.);
#191=B_SPLINE_CURVE_WITH_KNOTS('',3,(#15097,#15098,#15099,#15100,#15101,
#15102,#15103,#15104,#15105,#15106,#15107,#15108,#15109,#15110,#15111,#15112,
#15113,#15114,#15115,#15116,#15117,#15118,#15119,#15120,#15121,#15122,#15123,
#15124,#15125,#15126,#15127,#15128,#15129,#15130,#15131,#15132,#15133,#15134,
#15135,#15136,#15137,#15138,#15139,#15140,#15141,#15142,#15143,#15144,#15145,
#15146,#15147,#15148,#15149,#15150,#15151,#15152,#15153,#15154,#15155,#15156,
#15157,#15158,#15159,#15160,#15161,#15162,#15163,#15164,#15165,#15166,#15167,
#15168,#15169,#15170,#15171,#15172,#15173,#15174,#15175,#15176,#15177,#15178,
#15179,#15180,#15181,#15182,#15183,#15184,#15185,#15186,#15187,#15188,#15189,
#15190,#15191,#15192,#15193,#15194,#15195,#15196,#15197,#15198,#15199,#15200,
#15201,#15202,#15203,#15204,#15205,#15206,#15207,#15208,#15209,#15210,#15211,
#15212,#15213,#15214,#15215,#15216,#15217,#15218,#15219,#15220,#15221,#15222,
#15223,#15224,#15225,#15226,#15227,#15228,#15229,#15230,#15231,#15232,#15233,
#15234,#15235,#15236,#15237,#15238,#15239,#15240,#15241,#15242,#15243,#15244,
#15245,#15246,#15247,#15248,#15249,#15250,#15251,#15252,#15253,#15254,#15255,
#15256,#15257,#15258,#15259,#15260,#15261,#15262,#15263,#15264,#15265,#15266,
#15267,#15268,#15269,#15270,#15271,#15272,#15273,#15274,#15275,#15276,#15277,
#15278,#15279,#15280,#15281,#15282,#15283,#15284),.UNSPECIFIED.,.F.,.F.,
(4,2,2,2,2,2,2,2,2,2,2,2,2,2,2,2,2,2,2,2,2,2,2,2,2,2,2,2,2,2,2,2,2,2,2,
2,2,2,2,2,2,2,2,2,2,2,2,2,2,2,2,2,2,2,2,2,2,2,2,2,2,2,2,2,2,2,2,2,2,2,2,
2,2,2,2,2,2,2,2,2,2,2,2,2,2,2,2,2,2,2,2,2,2,4),(-1.96101303986741,-1.93902401091282,
-1.93113846510848,-1.92894324877324,-1.92741834039913,-1.92612012274045,
-1.92473222852842,-1.92297639792385,-1.91954411705765,-1.8931174819877,
-1.87529707263454,-1.85327739359925,-1.84994765342302,-1.84901615134286,
-1.84813011971587,-1.84735299763854,-1.84634762918817,-1.84471378202726,
-1.83526883130606,-1.81924644662274,-1.79774973243118,-1.78310945761126,
-1.77451653327791,-1.77203519316913,-1.77072863867773,-1.76948529762749,
-1.76786277831882,-1.76503224350567,-1.75339069778963,-1.71324624518786,
-1.69671232685801,-1.69411819909489,-1.69299722255528,-1.69220226652829,
-1.69146863637253,-1.69024979469663,-1.68709694070262,-1.68610250863524,
-1.68275133659059,-1.63800954869283,-1.62605200703821,-1.61859643106826,
-1.6162467927143,-1.61474749542882,-1.61334440509118,-1.61150773513733,
-1.60840522264195,-1.58381306331285,-1.56195946248712,-1.54093884855941,
-1.53840942963677,-1.53732794952146,-1.53654008479381,-1.53579626450685,
-1.53452492947323,-1.53103115499119,-1.50462156490907,-1.47688013913641,
-1.46393391637975,-1.46111389564662,-1.45951071638265,-1.45826749337579,
-1.45664114202461,-1.45379376307038,-1.44194328316521,-1.4360089645457,
-1.39194727688528,-1.38392672259596,-1.38229207967544,-1.38138548593529,
-1.38061088522677,-1.37963514054276,-1.3777337030146,-1.36599276707245,
-1.36229560630959,-1.31769132294265,-1.30784362638777,-1.30525436153139,
-1.30370200241855,-1.30231367907121,-1.30055456246614,-1.29710718493171,
-1.26781524875205,-1.25121268257237,-1.24289363998706,-1.22998683065394,
-1.22726223270271,-1.22614774752391,-1.22535403886612,-1.22461893855669,
-1.22339229425033,-1.22019029989984,-1.18507537092657,-1.16012005622424),
 .UNSPECIFIED.);
#192=B_SPLINE_CURVE_WITH_KNOTS('',3,(#15290,#15291,#15292,#15293,#15294,
#15295,#15296,#15297,#15298,#15299,#15300,#15301,#15302,#15303,#15304,#15305,
#15306,#15307,#15308,#15309,#15310,#15311,#15312,#15313,#15314,#15315,#15316,
#15317,#15318,#15319,#15320,#15321,#15322,#15323,#15324,#15325,#15326,#15327,
#15328,#15329,#15330,#15331,#15332,#15333,#15334,#15335,#15336,#15337,#15338,
#15339,#15340,#15341,#15342,#15343,#15344,#15345,#15346,#15347,#15348,#15349,
#15350,#15351,#15352,#15353,#15354,#15355,#15356,#15357,#15358,#15359,#15360,
#15361,#15362,#15363,#15364,#15365,#15366,#15367,#15368,#15369,#15370,#15371,
#15372,#15373,#15374,#15375,#15376,#15377,#15378,#15379,#15380,#15381,#15382,
#15383,#15384,#15385,#15386,#15387,#15388,#15389,#15390,#15391,#15392,#15393,
#15394,#15395,#15396,#15397,#15398,#15399,#15400,#15401,#15402,#15403,#15404,
#15405,#15406,#15407,#15408,#15409,#15410,#15411,#15412,#15413,#15414,#15415,
#15416,#15417,#15418,#15419,#15420,#15421,#15422,#15423,#15424,#15425,#15426,
#15427,#15428,#15429,#15430,#15431,#15432,#15433,#15434,#15435,#15436,#15437,
#15438,#15439,#15440,#15441,#15442,#15443,#15444,#15445,#15446,#15447,#15448,
#15449,#15450,#15451,#15452,#15453,#15454,#15455,#15456,#15457,#15458,#15459,
#15460,#15461,#15462,#15463,#15464,#15465,#15466,#15467,#15468,#15469,#15470,
#15471,#15472,#15473,#15474,#15475,#15476,#15477,#15478,#15479,#15480,#15481,
#15482,#15483,#15484,#15485,#15486,#15487,#15488,#15489,#15490,#15491,#15492,
#15493,#15494,#15495,#15496,#15497),.UNSPECIFIED.,.F.,.F.,(4,2,2,2,2,2,
2,2,2,2,2,2,2,2,2,2,2,2,2,2,2,2,2,2,2,2,2,2,2,2,2,2,2,2,2,2,2,2,2,2,2,2,
2,2,2,2,2,2,2,2,2,2,2,2,2,2,2,2,2,2,2,2,2,2,2,2,2,2,2,2,2,2,2,2,2,2,2,2,
2,2,2,2,2,2,2,2,2,2,2,2,2,2,2,2,2,2,2,2,2,2,2,2,2,4),(-0.801445826041384,
-0.800349872747114,-0.798233649121384,-0.797227462568897,-0.796449722874802,
-0.795562983792323,-0.794020444136553,-0.787405896305061,-0.745282452454743,
-0.724792932592394,-0.72177821601145,-0.719966491510252,-0.718566586111227,
-0.717055032691816,-0.714652845801367,-0.706736959950589,-0.693747847084072,
-0.656441125823533,-0.653896555831325,-0.644209249979237,-0.642562325177746,
-0.641563406516178,-0.640784597730487,-0.639903645509488,-0.638387224591242,
-0.632116295283881,-0.619899951401964,-0.588574070016861,-0.569103302469967,
-0.566113776876449,-0.564309400269157,-0.562910554451685,-0.561395542430526,
-0.558977919157017,-0.550919658642684,-0.537603603411906,-0.500456054967528,
-0.496273369488784,-0.488377184934789,-0.486829596030842,-0.485849921398991,
-0.485074566802187,-0.484169796547961,-0.482545229310055,-0.474705514007188,
-0.430488826995907,-0.424705793814949,-0.41268897356705,-0.410081980099038,
-0.40837435215295,-0.406989778392695,-0.405401511506826,-0.402652760045989,
-0.390790460628714,-0.346361891053286,-0.333094991300973,-0.331110579736527,
-0.330130335301258,-0.329354908091178,-0.328468659343816,-0.326904649506807,
-0.324963596360095,-0.320870029795502,-0.30896338727734,-0.277384920028211,
-0.257736322028934,-0.254742071525236,-0.252936218517003,-0.251537043489257,
-0.250022488151055,-0.247607352678036,-0.239573692920807,-0.22631494733403,
-0.205031505395017,-0.177570105319812,-0.175511292045496,-0.174516267460523,
-0.173739597030473,-0.172863521179655,-0.171350359937348,-0.169483324409091,
-0.165605886374729,-0.154628715563976,-0.12609596652198,-0.102270638965284,
-0.0991800710208497,-0.0973460714663988,-0.0959424819366718,-0.0944401796405462,
-0.0920806497362481,-0.0845497257440485,-0.0689544035445026,-0.0385355031996928,
-0.032373166813516,-0.0321516368702968,-0.02163216896645,-0.0199448253821705,
-0.0189339640671128,-0.0181535664101605,-0.0174261139967939,-0.016562105395811,
-0.015303185199615,-0.0109280128442772,-0.000459407788868288),
 .UNSPECIFIED.);
#193=B_SPLINE_CURVE_WITH_KNOTS('',3,(#15498,#15499,#15500,#15501,#15502,
#15503,#15504,#15505,#15506,#15507,#15508,#15509,#15510,#15511,#15512,#15513,
#15514,#15515,#15516,#15517,#15518,#15519,#15520,#15521,#15522,#15523,#15524,
#15525,#15526,#15527,#15528,#15529,#15530,#15531,#15532,#15533,#15534,#15535,
#15536,#15537,#15538,#15539),.UNSPECIFIED.,.F.,.F.,(4,2,2,2,2,2,2,2,2,2,
2,2,2,2,2,2,2,2,2,2,4),(-1.96128995591211,-1.92896923717076,-1.90915238863806,
-1.90460711608528,-1.90266581915441,-1.9012498872605,-1.89994913118757,
-1.89785539507136,-1.8927497295996,-1.85469262340958,-1.83834374865397,
-1.83052648440257,-1.82745437191466,-1.82520885095882,-1.82417525899136,
-1.82343299341078,-1.82268947117772,-1.82142116943337,-1.81794974541144,
-1.81752473904244,-1.78190244653125),.UNSPECIFIED.);
#194=B_SPLINE_CURVE_WITH_KNOTS('',3,(#15540,#15541,#15542,#15543,#15544,
#15545,#15546,#15547,#15548,#15549,#15550,#15551,#15552,#15553,#15554,#15555,
#15556,#15557,#15558,#15559,#15560,#15561,#15562,#15563,#15564,#15565,#15566,
#15567,#15568,#15569,#15570,#15571,#15572,#15573,#15574,#15575,#15576,#15577,
#15578,#15579,#15580,#15581,#15582,#15583,#15584,#15585,#15586,#15587,#15588,
#15589,#15590,#15591,#15592,#15593,#15594,#15595,#15596,#15597,#15598,#15599,
#15600,#15601,#15602,#15603,#15604,#15605,#15606,#15607,#15608,#15609,#15610,
#15611,#15612,#15613,#15614,#15615,#15616,#15617,#15618,#15619,#15620,#15621,
#15622,#15623,#15624,#15625,#15626,#15627,#15628,#15629,#15630,#15631,#15632,
#15633,#15634,#15635,#15636,#15637,#15638,#15639,#15640,#15641,#15642,#15643,
#15644,#15645,#15646,#15647,#15648,#15649,#15650,#15651,#15652,#15653,#15654,
#15655,#15656,#15657,#15658,#15659,#15660,#15661,#15662,#15663,#15664,#15665,
#15666,#15667,#15668,#15669,#15670,#15671,#15672,#15673,#15674,#15675,#15676,
#15677,#15678,#15679,#15680,#15681,#15682,#15683,#15684,#15685,#15686,#15687,
#15688,#15689,#15690,#15691,#15692,#15693,#15694,#15695,#15696,#15697,#15698,
#15699,#15700,#15701,#15702,#15703,#15704,#15705,#15706,#15707,#15708,#15709,
#15710,#15711,#15712,#15713,#15714,#15715,#15716,#15717,#15718,#15719,#15720,
#15721,#15722,#15723,#15724,#15725,#15726,#15727,#15728,#15729,#15730,#15731,
#15732,#15733,#15734,#15735,#15736,#15737,#15738,#15739,#15740,#15741,#15742,
#15743,#15744,#15745,#15746,#15747,#15748,#15749,#15750,#15751,#15752,#15753,
#15754,#15755,#15756,#15757,#15758,#15759,#15760,#15761,#15762,#15763,#15764,
#15765,#15766,#15767,#15768,#15769,#15770,#15771,#15772,#15773,#15774,#15775,
#15776,#15777,#15778,#15779),.UNSPECIFIED.,.F.,.F.,(4,2,2,2,2,2,2,2,2,2,
2,2,2,2,2,2,2,2,2,2,2,2,2,2,2,2,2,2,2,2,2,2,2,2,2,2,2,2,2,2,2,2,2,2,2,2,
2,2,2,2,2,2,2,2,2,2,2,2,2,2,2,2,2,2,2,2,2,2,2,2,2,2,2,2,2,2,2,2,2,2,2,2,
2,2,2,2,2,2,2,2,2,2,2,2,2,2,2,2,2,2,2,2,2,2,2,2,2,2,2,2,2,2,2,2,2,2,2,2,
2,4),(-1.16012005622424,-1.15415813050765,-1.15044685505235,-1.14865884109744,
-1.14726724866216,-1.14573120252076,-1.14321521305641,-1.13512049870346,
-1.13396102106544,-1.13373336672688,-1.08729962664451,-1.07764256493671,
-1.07408832682855,-1.07154034941925,-1.07045557817196,-1.06966708134879,
-1.06892407530831,-1.06765718839674,-1.06419268431622,-1.03535532330225,
-0.999284713641795,-0.995056232045912,-0.993171210352436,-0.991765435043037,
-0.990451878352686,-0.98864184224745,-0.984013991047981,-0.980812189523047,
-0.969509609496407,-0.946083219768486,-0.919857268268363,-0.916364437150595,
-0.915093186215055,-0.914349335666649,-0.913561372470622,-0.912479650843354,
-0.909949182919926,-0.888344440827802,-0.874037908551752,-0.84254476738048,
-0.839117849737984,-0.837363039771678,-0.835975107626667,-0.834420036767001,
-0.831818776909092,-0.821833726842604,-0.776863594799361,-0.773774600973159,
-0.770932056135287,-0.761710213942626,-0.760087552197246,-0.7590854243908,
-0.758308482307567,-0.757420048400854,-0.755868472902261,-0.74912221708597,
-0.73546018596828,-0.702648300221043,-0.686412338616625,-0.683558993829449,
-0.68177637404806,-0.680385174442506,-0.678845683479245,-0.67631516491035,
-0.667120697648695,-0.623690262423908,-0.606514485084176,-0.604434535733032,
-0.603435680968508,-0.602659006567975,-0.601768329715578,-0.600206814099761,
-0.593322625486607,-0.550394814609992,-0.530971301534117,-0.527984084170803,
-0.526180858437776,-0.5247827645668,-0.523268429371774,-0.520851594346215,
-0.512793382934143,-0.499475218952549,-0.462344527025023,-0.458244348019622,
-0.450272237834714,-0.448720454523785,-0.447739759462335,-0.446964690764981,
-0.446061523521919,-0.444443011983169,-0.436693025213383,-0.392432546389212,
-0.386823569434167,-0.374614413881065,-0.371995239021018,-0.370284298426949,
-0.368900140394718,-0.36731575998158,-0.364582377584561,-0.35292195375019,
-0.308378152637977,-0.295014398285981,-0.293027527126415,-0.292047087212644,
-0.291272006869944,-0.29045247645357,-0.289013942049652,-0.287233415920234,
-0.28360367381898,-0.273645944872561,-0.239275826685809,-0.219656087035516,
-0.21666367922967,-0.214858853159472,-0.213460427308733,-0.211946639042526,
-0.209532637939071,-0.2015020629797,-0.188248151775626,-0.17987795927969),
 .UNSPECIFIED.);
#195=B_SPLINE_CURVE_WITH_KNOTS('',3,(#15784,#15785,#15786,#15787,#15788,
#15789,#15790,#15791,#15792,#15793,#15794,#15795,#15796,#15797,#15798,#15799,
#15800,#15801,#15802,#15803,#15804,#15805,#15806,#15807,#15808,#15809,#15810,
#15811,#15812,#15813,#15814,#15815,#15816,#15817,#15818,#15819,#15820,#15821,
#15822,#15823,#15824,#15825,#15826,#15827,#15828,#15829,#15830,#15831,#15832,
#15833,#15834,#15835,#15836,#15837,#15838,#15839,#15840,#15841,#15842,#15843,
#15844,#15845,#15846,#15847,#15848,#15849,#15850,#15851,#15852,#15853,#15854,
#15855,#15856,#15857,#15858,#15859,#15860,#15861,#15862,#15863,#15864,#15865,
#15866,#15867,#15868,#15869,#15870,#15871,#15872,#15873,#15874,#15875,#15876,
#15877,#15878,#15879,#15880,#15881,#15882,#15883,#15884,#15885,#15886,#15887,
#15888,#15889,#15890,#15891,#15892,#15893,#15894,#15895,#15896,#15897,#15898,
#15899,#15900,#15901,#15902,#15903,#15904,#15905,#15906,#15907,#15908,#15909,
#15910,#15911,#15912,#15913,#15914,#15915,#15916,#15917,#15918,#15919,#15920,
#15921,#15922,#15923,#15924,#15925,#15926,#15927,#15928,#15929,#15930,#15931,
#15932,#15933,#15934,#15935,#15936,#15937,#15938,#15939,#15940,#15941,#15942,
#15943,#15944,#15945,#15946,#15947,#15948,#15949,#15950,#15951,#15952,#15953,
#15954,#15955,#15956,#15957,#15958,#15959,#15960,#15961,#15962,#15963,#15964,
#15965,#15966,#15967,#15968,#15969,#15970,#15971,#15972,#15973,#15974,#15975,
#15976,#15977,#15978,#15979,#15980,#15981,#15982,#15983,#15984,#15985,#15986,
#15987,#15988,#15989,#15990,#15991,#15992,#15993,#15994,#15995,#15996,#15997,
#15998,#15999,#16000,#16001,#16002,#16003,#16004,#16005,#16006,#16007,#16008,
#16009,#16010,#16011),.UNSPECIFIED.,.F.,.F.,(4,2,2,2,2,2,2,2,2,2,2,2,2,
2,2,2,2,2,2,2,2,2,2,2,2,2,2,2,2,2,2,2,2,2,2,2,2,2,2,2,2,2,2,2,2,2,2,2,2,
2,2,2,2,2,2,2,2,2,2,2,2,2,2,2,2,2,2,2,2,2,2,2,2,2,2,2,2,2,2,2,2,2,2,2,2,
2,2,2,2,2,2,2,2,2,2,2,2,2,2,2,2,2,2,2,2,2,2,2,2,2,2,2,2,4),(-1.7820183274493,
-1.77638176080533,-1.74715212882205,-1.73833521233597,-1.73499552512745,
-1.73256791526149,-1.73150382689449,-1.73071830156585,-1.72996829096072,
-1.72866767460946,-1.72499426195066,-1.72344811708588,-1.67485095227704,
-1.66397287879935,-1.65701637496962,-1.65530428363814,-1.65369986399018,
-1.6523477953927,-1.65071053970372,-1.64787124038574,-1.63583794333267,
-1.63004712718618,-1.58575486349801,-1.57797877267479,-1.57635805682508,
-1.57545412478334,-1.57467867994129,-1.57369785922229,-1.57171046213532,
-1.55834901701542,-1.5137672909055,-1.50215645110387,-1.4994257439447,-1.49784145138354,
-1.49645649319771,-1.49474342866019,-1.49211885453612,-1.47984899192827,
-1.44194754241661,-1.42873981219348,-1.42213958354263,-1.42059807233498,
-1.41971155431095,-1.41893376159289,-1.4179271876616,-1.41580900364501,
-1.39400946423344,-1.38829795325573,-1.35982960417762,-1.34669547024539,
-1.34386202417565,-1.3422551137299,-1.34101082874239,-1.33938570056183,
-1.33654710679659,-1.32482413520142,-1.31876638779678,-1.27469201592413,
-1.26663225904502,-1.26499438278356,-1.26408664086502,-1.26331144853767,
-1.26233544059798,-1.2604349040229,-1.24874581441117,-1.24525586328687,
-1.20044383639529,-1.19051993139808,-1.18792267273261,-1.18636775368084,
-1.18497854429074,-1.18322020403655,-1.17978033483721,-1.1527222218404,
-1.14614919292542,-1.12553946981631,-1.11590822462521,-1.11235976839988,
-1.10981464006502,-1.10872990641278,-1.10794098833984,-1.10719721838534,
-1.10592822305707,-1.10245337221938,-1.07400989047575,-1.03729458758953,
-1.03322445961232,-1.03136752899994,-1.02996541863394,-1.02864260311311,
-1.02679952077802,-1.02197163841473,-0.980595005383374,-0.96683214214974,
-0.955683882751211,-0.953970449650863,-0.952951972635141,-0.952170538977476,
-0.951300593586297,-0.949833893519707,-0.944166428436368,-0.933654875851704,
-0.926145783705573,-0.925335701235225,-0.882593183474118,-0.877926393932956,
-0.876109201278924,-0.874793204445442,-0.87338738685576,-0.871506757785655,
-0.867306855534465,-0.850196437521089,-0.821319314117838,-0.801445826041384),
 .UNSPECIFIED.);
#196=B_SPLINE_CURVE_WITH_KNOTS('',3,(#16013,#16014,#16015,#16016,#16017,
#16018,#16019,#16020,#16021,#16022,#16023,#16024,#16025,#16026,#16027,#16028,
#16029,#16030,#16031,#16032,#16033,#16034,#16035,#16036,#16037,#16038,#16039,
#16040,#16041,#16042,#16043,#16044,#16045,#16046,#16047,#16048,#16049,#16050,
#16051,#16052,#16053,#16054),.UNSPECIFIED.,.F.,.F.,(4,2,2,2,2,2,2,2,2,2,
2,2,2,2,2,2,2,2,2,2,4),(-0.17987795927969,-0.145959516617287,-0.138816103552565,
-0.137318875760568,-0.136354831707817,-0.135580707523949,-0.134682747526293,
-0.133106271723474,-0.131118248051813,-0.126885155200885,-0.114356570881015,
-0.0822039428817398,-0.0755338261407026,-0.0632995564264635,-0.0606778611037748,
-0.0589659393235315,-0.0575814286910333,-0.0559971284805531,-0.053265106453469,
-0.0416293542253508,-0.000460323532593378),.UNSPECIFIED.);
#197=B_SPLINE_CURVE_WITH_KNOTS('',3,(#16055,#16056,#16057,#16058,#16059,
#16060,#16061,#16062,#16063,#16064,#16065,#16066,#16067,#16068,#16069,#16070,
#16071,#16072,#16073,#16074,#16075,#16076,#16077,#16078,#16079,#16080,#16081,
#16082,#16083,#16084,#16085,#16086,#16087,#16088,#16089,#16090,#16091,#16092,
#16093,#16094,#16095,#16096,#16097,#16098,#16099,#16100,#16101,#16102,#16103,
#16104,#16105,#16106,#16107,#16108,#16109,#16110,#16111,#16112,#16113,#16114,
#16115,#16116,#16117,#16118,#16119,#16120,#16121,#16122,#16123,#16124,#16125,
#16126,#16127,#16128,#16129,#16130,#16131,#16132,#16133,#16134,#16135,#16136),
 .UNSPECIFIED.,.F.,.F.,(4,3,3,3,3,3,3,3,3,3,3,3,3,3,3,3,3,3,3,3,3,3,3,3,
3,3,3,4),(116.238928182823,116.369122527555,116.567664818425,116.767442819537,
116.965528358298,117.166152590585,117.366776822873,117.565319113743,117.765097114855,
117.963182653616,118.163806885904,118.364431118192,118.562973409062,118.762751410174,
118.960836948935,119.161461181222,119.36208541351,119.56062770438,119.760405705492,
119.958491244253,120.159115476541,120.359739708829,120.558281999699,120.758060000811,
120.956145539572,121.156769771859,121.357394004147,121.373252558517),
 .UNSPECIFIED.);
#198=B_SPLINE_CURVE_WITH_KNOTS('',3,(#16142,#16143,#16144,#16145,#16146,
#16147,#16148,#16149,#16150),.UNSPECIFIED.,.F.,.F.,(4,1,1,1,1,1,4),(122.522113490002,
123.040830884369,124.038485179687,125.036139475006,126.033793770324,127.031448065643,
127.655725185573),.UNSPECIFIED.);
#199=B_SPLINE_CURVE_WITH_KNOTS('',3,(#16151,#16152,#16153,#16154,#16155,
#16156,#16157,#16158,#16159,#16160,#16161,#16162,#16163,#16164,#16165,#16166,
#16167,#16168,#16169,#16170,#16171,#16172,#16173,#16174,#16175,#16176,#16177,
#16178,#16179,#16180,#16181,#16182,#16183,#16184,#16185,#16186,#16187,#16188,
#16189,#16190,#16191,#16192,#16193,#16194,#16195,#16196,#16197,#16198,#16199,
#16200,#16201,#16202,#16203,#16204,#16205,#16206,#16207,#16208,#16209,#16210,
#16211,#16212,#16213,#16214,#16215,#16216,#16217,#16218,#16219,#16220,#16221,
#16222,#16223,#16224,#16225,#16226,#16227,#16228,#16229,#16230,#16231,#16232,
#16233,#16234),.UNSPECIFIED.,.F.,.F.,(4,2,2,2,2,2,2,2,2,2,2,2,2,2,2,2,2,
2,2,2,2,2,2,2,2,2,2,2,2,2,2,2,2,2,2,2,2,2,2,2,2,4),(-1.96128222253846,-1.95958363623628,
-1.95630370014159,-1.94144445515337,-1.89718230505077,-1.88936987786217,
-1.88774696253415,-1.88684256059216,-1.88606717896178,-1.88508703610749,
-1.88310296685397,-1.8698417562419,-1.8346986810638,-1.8211583699688,-1.81300241363437,
-1.81120770552465,-1.80954407165404,-1.80952953053889,-1.80951457375782,
-1.80949916961573,-1.80948328329705,-1.80946687643486,-1.80944990661459,
-1.80943232678431,-1.80941408455338,-1.80939512135814,-1.8093753714631,
-1.80935476074941,-1.80933320523811,-1.80931060928038,-1.80928686332031,
-1.80926184108749,-1.80923539605991,-1.80920735663572,-1.8091775206023,
-1.80914564843925,-1.80911883506897,-1.80908079907286,-1.80774045339956,
-1.80600936930746,-1.80260197344681,-1.7820183274493),.UNSPECIFIED.);
#200=B_SPLINE_CURVE_WITH_KNOTS('',3,(#16236,#16237,#16238,#16239,#16240,
#16241,#16242,#16243,#16244,#16245,#16246,#16247,#16248,#16249,#16250,#16251,
#16252,#16253,#16254),.UNSPECIFIED.,.F.,.F.,(4,3,3,3,3,3,4),(121.373252558517,
121.571751272604,121.7700124529,121.968092146591,122.166669391268,122.355048299466,
122.522113490002),.UNSPECIFIED.);
#201=B_SPLINE_CURVE_WITH_KNOTS('',3,(#16255,#16256,#16257,#16258,#16259,
#16260,#16261,#16262,#16263),.UNSPECIFIED.,.F.,.F.,(4,1,1,1,1,1,4),(122.522119580395,
123.352702594784,124.350356890103,125.348011185421,126.34566548074,127.343319776058,
127.657159480932),.UNSPECIFIED.);
#202=B_SPLINE_CURVE_WITH_KNOTS('',3,(#16269,#16270,#16271,#16272,#16273,
#16274,#16275,#16276,#16277,#16278,#16279,#16280,#16281,#16282,#16283,#16284,
#16285,#16286,#16287,#16288,#16289,#16290,#16291,#16292,#16293,#16294,#16295,
#16296,#16297,#16298,#16299,#16300,#16301,#16302,#16303,#16304,#16305,#16306,
#16307,#16308,#16309,#16310,#16311,#16312,#16313,#16314,#16315,#16316,#16317,
#16318,#16319,#16320,#16321,#16322,#16323,#16324,#16325,#16326,#16327,#16328,
#16329,#16330,#16331,#16332,#16333,#16334,#16335,#16336,#16337,#16338,#16339,
#16340,#16341,#16342,#16343,#16344,#16345,#16346,#16347),.UNSPECIFIED.,
 .F.,.F.,(4,3,3,3,3,3,3,3,3,3,3,3,3,3,3,3,3,3,3,3,3,3,3,3,3,3,4),(128.805298797182,
129.02675665628,129.22529894715,129.425076948262,129.623162487023,129.82378671931,
130.024410951598,130.222953242468,130.42273124358,130.620816782341,130.821441014629,
131.022065246917,131.220607537787,131.420385538899,131.61847107766,131.819095309947,
132.019719542235,132.218261833105,132.418039834217,132.616125372978,132.816749605266,
133.017373837554,133.215921390413,133.414151854748,133.612180481121,133.810554859578,
133.939161505613),.UNSPECIFIED.);
#203=B_SPLINE_CURVE_WITH_KNOTS('',3,(#16348,#16349,#16350,#16351,#16352),
 .UNSPECIFIED.,.F.,.F.,(4,1,4),(127.655725185573,128.029102360961,128.805297760461),
 .UNSPECIFIED.);
#204=B_SPLINE_CURVE_WITH_KNOTS('',3,(#16354,#16355,#16356,#16357,#16358),
 .UNSPECIFIED.,.F.,.F.,(4,1,4),(127.657159480932,128.340974071377,128.805296175662),
 .UNSPECIFIED.);
#205=B_SPLINE_CURVE_WITH_KNOTS('',3,(#16359,#16360,#16361,#16362,#16363,
#16364,#16365,#16366,#16367,#16368,#16369,#16370,#16371,#16372,#16373,#16374,
#16375,#16376,#16377,#16378,#16379,#16380,#16381,#16382,#16383,#16384,#16385,
#16386,#16387,#16388,#16389,#16390,#16391,#16392,#16393,#16394,#16395,#16396,
#16397,#16398,#16399,#16400,#16401,#16402,#16403,#16404,#16405,#16406,#16407,
#16408,#16409,#16410,#16411,#16412,#16413,#16414,#16415,#16416,#16417,#16418,
#16419,#16420,#16421,#16422,#16423,#16424,#16425,#16426,#16427,#16428,#16429,
#16430,#16431,#16432,#16433,#16434,#16435,#16436,#16437,#16438,#16439,#16440,
#16441,#16442,#16443,#16444,#16445,#16446,#16447,#16448,#16449,#16450,#16451,
#16452,#16453,#16454,#16455,#16456,#16457,#16458,#16459,#16460,#16461,#16462,
#16463,#16464,#16465,#16466,#16467,#16468,#16469,#16470,#16471,#16472,#16473,
#16474,#16475,#16476,#16477,#16478,#16479,#16480,#16481,#16482,#16483,#16484,
#16485,#16486,#16487,#16488,#16489,#16490,#16491,#16492,#16493,#16494,#16495,
#16496,#16497,#16498,#16499,#16500,#16501,#16502,#16503,#16504,#16505,#16506,
#16507,#16508,#16509,#16510,#16511,#16512,#16513,#16514,#16515,#16516,#16517,
#16518,#16519,#16520,#16521,#16522,#16523,#16524,#16525,#16526,#16527,#16528,
#16529,#16530,#16531,#16532,#16533,#16534,#16535,#16536,#16537,#16538,#16539,
#16540,#16541,#16542,#16543,#16544,#16545,#16546,#16547,#16548,#16549,#16550,
#16551,#16552,#16553,#16554,#16555,#16556,#16557,#16558),.UNSPECIFIED.,
 .F.,.F.,(4,2,2,2,2,2,2,2,2,2,2,2,2,2,2,2,2,2,2,2,2,2,2,2,2,2,2,2,2,2,2,
2,2,2,2,2,2,2,2,2,2,2,2,2,2,2,2,2,2,2,2,2,2,2,2,2,2,2,2,2,2,2,2,2,2,2,2,
2,2,2,2,2,2,2,2,2,2,2,2,2,2,2,2,2,2,2,2,2,2,2,2,2,2,2,2,2,2,2,2,4),(-1.96108238987861,
-1.95962527398827,-1.95805600276329,-1.95670126082934,-1.95536452789458,
-1.95403545240248,-1.95179028303077,-1.94573147315617,-1.89863151775104,
-1.88663302728454,-1.8804379472618,-1.87892792299045,-1.87804862810209,
-1.8772699012373,-1.87626932856835,-1.87461606059931,-1.86478964781739,
-1.86249101981947,-1.83467772864677,-1.80872771981097,-1.80518064403458,
-1.80309568869222,-1.80122435588287,-1.79983924839755,-1.7985360549032,
-1.79642785598399,-1.79125080324649,-1.75458124763867,-1.72651427561873,
-1.72391824403796,-1.72282505883563,-1.72203495360458,-1.72129401263089,
-1.72003831269686,-1.71664860811503,-1.68426485737966,-1.65367330149517,
-1.64983793789101,-1.64763652277233,-1.64610884268141,-1.64463554055501,
-1.64327458345385,-1.64147264707135,-1.63849017037257,-1.61893317628298,
-1.58744910862982,-1.57537346873885,-1.56915179643041,-1.56763960712186,
-1.56675979845136,-1.5659811184105,-1.56498125237321,-1.56333048592694,
-1.55355650504723,-1.53725460120878,-1.51293280581748,-1.50054908094957,
-1.49290054874344,-1.49052835258819,-1.48902368985411,-1.48762186672719,
-1.48579585723203,-1.48273133872076,-1.46016500993314,-1.45185120721396,
-1.43676378281074,-1.41517637294027,-1.41264483764011,-1.41156273648884,
-1.41077452782028,-1.41003046971386,-1.40875891710535,-1.40526558237236,
-1.37906847406862,-1.35114080388952,-1.33814455470387,-1.33532057144844,
-1.33371613596061,-1.33247240823027,-1.33084606811697,-1.32800042268292,
-1.31618089301717,-1.31021173080889,-1.26615238992651,-1.25810335186605,
-1.25646657315324,-1.25555929725335,-1.25478441994791,-1.25380871743035,
-1.25190851572126,-1.24021399338478,-1.23658494020635,-1.19187905017021,
-1.18199292865903,-1.17939963839018,-1.17784600162827,-1.17645725159261,
-1.17469856550342,-1.17125510381233,-1.16001003225657),.UNSPECIFIED.);
#206=B_SPLINE_CURVE_WITH_KNOTS('',3,(#16564,#16565,#16566,#16567,#16568,
#16569,#16570,#16571,#16572,#16573,#16574,#16575,#16576,#16577,#16578,#16579,
#16580,#16581,#16582,#16583,#16584,#16585,#16586,#16587,#16588,#16589,#16590,
#16591,#16592,#16593,#16594,#16595,#16596,#16597,#16598,#16599,#16600,#16601,
#16602,#16603,#16604,#16605,#16606,#16607,#16608,#16609,#16610,#16611,#16612,
#16613,#16614,#16615,#16616,#16617,#16618,#16619,#16620,#16621,#16622,#16623,
#16624,#16625,#16626,#16627,#16628,#16629,#16630,#16631,#16632,#16633,#16634,
#16635,#16636,#16637,#16638,#16639,#16640,#16641,#16642,#16643,#16644,#16645,
#16646,#16647,#16648,#16649,#16650,#16651,#16652,#16653,#16654,#16655,#16656,
#16657,#16658,#16659,#16660,#16661,#16662,#16663,#16664,#16665,#16666,#16667,
#16668,#16669,#16670,#16671,#16672,#16673,#16674,#16675,#16676,#16677,#16678,
#16679,#16680,#16681,#16682,#16683,#16684,#16685,#16686,#16687,#16688,#16689,
#16690,#16691,#16692,#16693,#16694,#16695,#16696,#16697,#16698,#16699,#16700,
#16701,#16702,#16703,#16704,#16705,#16706,#16707,#16708,#16709,#16710,#16711,
#16712,#16713,#16714,#16715,#16716,#16717,#16718,#16719,#16720,#16721,#16722,
#16723,#16724,#16725,#16726,#16727,#16728,#16729,#16730,#16731,#16732,#16733,
#16734,#16735,#16736,#16737,#16738,#16739,#16740,#16741,#16742,#16743,#16744,
#16745,#16746,#16747,#16748,#16749,#16750,#16751),.UNSPECIFIED.,.F.,.F.,
(4,2,2,2,2,2,2,2,2,2,2,2,2,2,2,2,2,2,2,2,2,2,2,2,2,2,2,2,2,2,2,2,2,2,2,
2,2,2,2,2,2,2,2,2,2,2,2,2,2,2,2,2,2,2,2,2,2,2,2,2,2,2,2,2,2,2,2,2,2,2,2,
2,2,2,2,2,2,2,2,2,2,2,2,2,2,2,2,2,2,2,2,2,2,4),(-0.801648158832126,-0.78213823686765,
-0.781014765677329,-0.770306567636845,-0.768611249732307,-0.767598142695125,
-0.766817552819496,-0.765944911392444,-0.76446572093286,-0.758651079336189,
-0.747735441952474,-0.726495051199371,-0.695357700750936,-0.691931669929365,
-0.690176460432175,-0.68878778941575,-0.687231444709382,-0.684626985824291,
-0.674616138217384,-0.629561927187327,-0.626701306196766,-0.624390725327106,
-0.614561649852437,-0.612907690563772,-0.611906674151297,-0.611127581383509,
-0.610247829361824,-0.608736920519546,-0.602536551650829,-0.590526830318372,
-0.559015781156644,-0.539444088903777,-0.536451899042796,-0.534646702930499,
-0.53324768945808,-0.531732962470556,-0.529316803763471,-0.521272795872992,
-0.507989875744357,-0.470701058912443,-0.459048226596414,-0.45714918610198,
-0.456173552892839,-0.455398452048785,-0.454490574492869,-0.452851847420105,
-0.44477535977028,-0.400742970753238,-0.394662428765651,-0.38297186749627,
-0.380135974334613,-0.378511493532836,-0.377267234426126,-0.375659796446321,
-0.372823799876876,-0.359648317775045,-0.331011393757186,-0.303577241885318,
-0.301518493494147,-0.300523512882973,-0.299769524916084,-0.29889802404045,
-0.297972817000706,-0.29656526584481,-0.293955182604191,-0.267935405277803,
-0.230946648362081,-0.225781533148655,-0.223677629722732,-0.222374841617613,
-0.220960079590524,-0.219026489731675,-0.214527177807558,-0.195082563635142,
-0.167455048587957,-0.147993955374993,-0.145887426004711,-0.144883128266496,
-0.144136091225494,-0.143276738016289,-0.141859162851745,-0.140120958147904,
-0.136611646115393,-0.127135950678105,-0.0934422327538317,-0.0725036106061738,
-0.0694773029840937,-0.0676621500206694,-0.0662616758716257,-0.0647515672106966,
-0.0623560866390103,-0.0545021128486099,-0.0416542836801877,-0.000460315519253413),
 .UNSPECIFIED.);
#207=B_SPLINE_CURVE_WITH_KNOTS('',3,(#16752,#16753,#16754,#16755,#16756,
#16757,#16758,#16759,#16760,#16761,#16762,#16763,#16764,#16765,#16766,#16767,
#16768,#16769,#16770,#16771,#16772,#16773),.UNSPECIFIED.,.F.,.F.,(4,3,3,
3,3,3,3,4),(133.939161505613,134.015028132872,134.213570423742,134.413348424854,
134.611433963615,134.812058195903,135.012682428191,135.088484104361),
 .UNSPECIFIED.);
#208=B_SPLINE_CURVE_WITH_KNOTS('',3,(#16774,#16775,#16776,#16777,#16778,
#16779,#16780,#16781,#16782,#16783,#16784,#16785,#16786,#16787,#16788,#16789,
#16790,#16791,#16792,#16793,#16794,#16795,#16796,#16797,#16798,#16799,#16800,
#16801,#16802,#16803,#16804,#16805,#16806,#16807,#16808,#16809,#16810,#16811,
#16812,#16813,#16814,#16815,#16816,#16817,#16818,#16819,#16820,#16821,#16822,
#16823,#16824,#16825,#16826,#16827,#16828,#16829,#16830,#16831,#16832,#16833,
#16834,#16835,#16836,#16837,#16838,#16839,#16840,#16841,#16842,#16843,#16844,
#16845,#16846,#16847,#16848,#16849,#16850,#16851,#16852,#16853,#16854,#16855,
#16856,#16857,#16858,#16859,#16860,#16861,#16862,#16863,#16864,#16865,#16866,
#16867,#16868,#16869,#16870,#16871,#16872,#16873,#16874,#16875,#16876,#16877,
#16878,#16879,#16880,#16881,#16882,#16883,#16884,#16885,#16886,#16887,#16888,
#16889,#16890,#16891,#16892,#16893,#16894,#16895,#16896,#16897,#16898,#16899,
#16900,#16901,#16902,#16903,#16904,#16905,#16906,#16907,#16908,#16909,#16910,
#16911,#16912,#16913,#16914,#16915,#16916,#16917,#16918,#16919,#16920,#16921,
#16922,#16923,#16924,#16925,#16926,#16927,#16928,#16929,#16930,#16931,#16932,
#16933,#16934,#16935,#16936,#16937,#16938,#16939,#16940,#16941,#16942,#16943,
#16944,#16945,#16946,#16947,#16948,#16949,#16950,#16951,#16952,#16953,#16954,
#16955,#16956,#16957,#16958,#16959,#16960,#16961,#16962,#16963,#16964,#16965,
#16966,#16967,#16968,#16969,#16970,#16971,#16972,#16973,#16974,#16975,#16976,
#16977,#16978,#16979,#16980,#16981,#16982,#16983,#16984,#16985,#16986,#16987,
#16988,#16989,#16990,#16991,#16992,#16993,#16994,#16995,#16996,#16997,#16998,
#16999,#17000,#17001,#17002,#17003),.UNSPECIFIED.,.F.,.F.,(4,2,2,2,2,2,
2,2,2,2,2,2,2,2,2,2,2,2,2,2,2,2,2,2,2,2,2,2,2,2,2,2,2,2,2,2,2,2,2,2,2,2,
2,2,2,2,2,2,2,2,2,2,2,2,2,2,2,2,2,2,2,2,2,2,2,2,2,2,2,2,2,2,2,2,2,2,2,2,
2,2,2,2,2,2,2,2,2,2,2,2,2,2,2,2,2,2,2,2,2,2,2,2,2,2,2,2,2,2,2,2,2,2,2,2,
4),(-1.16001003225657,-1.1429307201912,-1.11889769922653,-1.10795658489296,
-1.10213363116416,-1.100653952482,-1.09978133247617,-1.09900097538504,-1.0979884743361,
-1.09629482640386,-1.08561871277599,-1.07936970935277,-1.04801404557703,
-1.02930305097426,-1.02489588234255,-1.02297868676905,-1.02156711054281,
-1.02026104238578,-1.01813792674338,-1.01285694873877,-0.980611544930864,
-0.973858585284931,-0.972027388600992,-0.959198144127172,-0.956755689781633,
-0.94710621148281,-0.945461516435653,-0.944463421923748,-0.943684927527861,
-0.942803973204306,-0.941286746692366,-0.935001344956756,-0.922741110165887,
-0.891421398550156,-0.872000821566398,-0.869013212815021,-0.867209697584171,
-0.86581134765867,-0.864296703570325,-0.861879307230727,-0.853818588799811,
-0.840495630159603,-0.803368759929907,-0.791622190722028,-0.789719971468083,
-0.788743860607362,-0.787968987763851,-0.787062092534455,-0.785426957310112,
-0.777404578436029,-0.733351016303359,-0.72741551957575,-0.715565766575734,
-0.712717676802668,-0.711090760529626,-0.709847025642558,-0.708243086832567,
-0.705421453421397,-0.6924633077725,-0.664682568163185,-0.638259582356622,
-0.634763846556083,-0.633491891371915,-0.632747731985936,-0.631959527595578,
-0.630877613907926,-0.62834731644099,-0.607257023549327,-0.584930046436624,
-0.560871674365034,-0.557777652939642,-0.55594301500481,-0.554539756196093,
-0.553038607257348,-0.550682569759479,-0.543177185660699,-0.531109851804377,
-0.507025749923546,-0.480562605538079,-0.47848221045133,-0.477483180014358,
-0.476706386907004,-0.475815594023372,-0.474253922615354,-0.467369805234921,
-0.424439493958543,-0.405008167397624,-0.40202037573363,-0.400216842870063,
-0.398818534341326,-0.397303990073394,-0.394886872118563,-0.386828189232162,
-0.373509729466546,-0.336365544703593,-0.33220204331563,-0.32428963198472,
-0.322741395169118,-0.321761706255257,-0.321005178755623,-0.320128252130178,
-0.319189324392779,-0.317748381396495,-0.31505010845968,-0.287025516163436,
-0.252339164762221,-0.247086932824349,-0.244968773037614,-0.243663660612136,
-0.242251475578793,-0.240330533807881,-0.235901744386162,-0.217016213327319,
-0.186955256986825,-0.179694752014396),.UNSPECIFIED.);
#209=B_SPLINE_CURVE_WITH_KNOTS('',3,(#17008,#17009,#17010,#17011,#17012,
#17013,#17014,#17015,#17016,#17017,#17018,#17019,#17020,#17021,#17022,#17023,
#17024,#17025,#17026,#17027,#17028,#17029,#17030,#17031,#17032,#17033,#17034,
#17035,#17036,#17037,#17038,#17039,#17040,#17041,#17042,#17043,#17044,#17045,
#17046,#17047,#17048,#17049,#17050,#17051,#17052,#17053,#17054,#17055,#17056,
#17057,#17058,#17059,#17060,#17061,#17062,#17063,#17064,#17065,#17066,#17067,
#17068,#17069,#17070,#17071,#17072,#17073,#17074,#17075,#17076,#17077,#17078,
#17079,#17080,#17081,#17082,#17083,#17084,#17085,#17086,#17087,#17088,#17089,
#17090,#17091,#17092,#17093,#17094,#17095,#17096,#17097,#17098,#17099,#17100,
#17101,#17102,#17103,#17104,#17105,#17106,#17107,#17108,#17109,#17110,#17111,
#17112,#17113,#17114,#17115,#17116,#17117,#17118,#17119,#17120,#17121,#17122,
#17123,#17124,#17125,#17126,#17127,#17128,#17129,#17130,#17131,#17132,#17133,
#17134,#17135,#17136,#17137,#17138,#17139,#17140,#17141,#17142,#17143,#17144,
#17145,#17146,#17147,#17148,#17149,#17150,#17151,#17152,#17153,#17154,#17155,
#17156,#17157,#17158,#17159,#17160,#17161,#17162,#17163,#17164,#17165,#17166,
#17167,#17168,#17169,#17170,#17171,#17172,#17173,#17174,#17175,#17176,#17177,
#17178,#17179,#17180,#17181,#17182,#17183,#17184,#17185,#17186,#17187,#17188,
#17189,#17190,#17191,#17192,#17193,#17194,#17195,#17196,#17197,#17198,#17199,
#17200,#17201,#17202,#17203,#17204,#17205,#17206,#17207,#17208,#17209,#17210,
#17211,#17212,#17213,#17214,#17215,#17216,#17217,#17218,#17219,#17220,#17221,
#17222,#17223,#17224,#17225,#17226,#17227,#17228,#17229,#17230,#17231,#17232,
#17233,#17234,#17235,#17236,#17237,#17238,#17239,#17240,#17241,#17242,#17243,
#17244,#17245,#17246,#17247,#17248,#17249,#17250,#17251,#17252,#17253,#17254,
#17255,#17256,#17257,#17258,#17259,#17260,#17261,#17262,#17263),
 .UNSPECIFIED.,.F.,.F.,(4,2,2,2,2,2,2,2,2,2,2,2,2,2,2,2,2,2,2,2,2,2,2,2,
2,2,2,2,2,2,2,2,2,2,2,2,2,2,2,2,2,2,2,2,2,2,2,2,2,2,2,2,2,2,2,2,2,2,2,2,
2,2,2,2,2,2,2,2,2,2,2,2,2,2,2,2,2,2,2,2,2,2,2,2,2,2,2,2,2,2,2,2,2,2,2,2,
2,2,2,2,2,2,2,2,2,2,2,2,2,2,2,2,2,2,2,2,2,2,2,2,2,2,2,2,2,2,2,4),(-1.78189016740401,
-1.78097762397856,-1.7793868830838,-1.77937825793148,-1.77936932347904,
-1.77936006788285,-1.77935047755204,-1.7793405383494,-1.7793302395449,-1.77931956715433,
-1.779308506606,-1.7792970427107,-1.77928515963152,-1.77927284135281,-1.7778882946397,
-1.77617212134381,-1.77353599926515,-1.76107718639576,-1.75568937526266,
-1.71117029652588,-1.70374008738545,-1.70211528874888,-1.70121071634051,
-1.7004357291812,-1.69945677749505,-1.69791082421215,-1.69003288258165,
-1.68584165643759,-1.68215848393462,-1.63753630787342,-1.63104399407679,
-1.62784095298482,-1.62519509499241,-1.62364044872693,-1.62225638809367,
-1.62054783360161,-1.61793650478277,-1.60584462045305,-1.59889974118267,
-1.55509820923944,-1.54800473144218,-1.54642858847634,-1.54553464041386,
-1.54475834997213,-1.54376420841648,-1.54170856799923,-1.5142139133888,
-1.48566929350021,-1.47251844714414,-1.46968473067084,-1.46807814025253,
-1.46683432537117,-1.46521012818052,-1.46237396633077,-1.45067204613949,
-1.44460146148795,-1.4005529965357,-1.39248476217533,-1.39084683611567,
-1.38993929508306,-1.38916441346297,-1.38818897412444,-1.38629006814448,
-1.37462850018787,-1.33739622727743,-1.32411976353444,-1.31607816499716,
-1.31366267372027,-1.31214834641487,-1.31074968885041,-1.30894493243135,
-1.30595340432594,-1.28639492673917,-1.25490722278886,-1.24285582497432,
-1.23664232804476,-1.23513061408447,-1.23425081626536,-1.23347196268052,
-1.23247162349808,-1.23081955340855,-1.22102261221577,-1.1848116113587,
-1.16952034496615,-1.16063618711611,-1.15813474793616,-1.15660138114605,
-1.15520815376355,-1.15341233308467,-1.15051622761162,-1.13335023638649,
-1.08933178059441,-1.08121658028887,-1.07957576491946,-1.07866752615317,
-1.07789259797486,-1.07691779955488,-1.07502220146438,-1.063449218963,-1.02596396727725,
-1.0079534196037,-1.00363555404761,-1.00173389192165,-1.0003247311448,-0.999014467137427,
-0.996869909828757,-0.991465201524918,-0.990221588073983,-0.985796184932943,
-0.980827381378573,-0.945955797577871,-0.926334582089454,-0.924227244646424,
-0.923222828785436,-0.922445329923792,-0.921557606157399,-0.920010413397297,
-0.913331328182177,-0.871037532483332,-0.850785719417413,-0.847777190640499,
-0.845967354780583,-0.844567828470549,-0.843055611742428,-0.840650064235996,
-0.832702091163431,-0.819639154923715,-0.801648158832126),.UNSPECIFIED.);
#210=B_SPLINE_CURVE_WITH_KNOTS('',3,(#17265,#17266,#17267,#17268,#17269,
#17270,#17271,#17272,#17273,#17274,#17275,#17276,#17277,#17278,#17279,#17280,
#17281,#17282,#17283,#17284,#17285,#17286,#17287,#17288,#17289,#17290,#17291,
#17292,#17293,#17294,#17295,#17296,#17297,#17298,#17299,#17300,#17301,#17302,
#17303,#17304,#17305,#17306,#17307,#17308,#17309,#17310,#17311,#17312,#17313,
#17314,#17315,#17316,#17317,#17318,#17319,#17320,#17321,#17322,#17323,#17324,
#17325,#17326,#17327,#17328,#17329,#17330,#17331,#17332,#17333,#17334,#17335,
#17336,#17337,#17338,#17339,#17340,#17341,#17342,#17343,#17344),
 .UNSPECIFIED.,.F.,.F.,(4,2,2,2,2,2,2,2,2,2,2,2,2,2,2,2,2,2,2,2,2,2,2,2,
2,2,2,2,2,2,2,2,2,2,2,2,2,2,2,4),(-0.179694752014396,-0.169232971543531,
-0.167146791452086,-0.16614665326122,-0.16539187472898,-0.165389478319393,
-0.165387101742208,-0.165384730808494,-0.16538237492749,-0.1653800340132,
-0.165377707927058,-0.165375396557726,-0.165373099830874,-0.165370817625747,
-0.165368549846061,-0.164499024789559,-0.162997007392346,-0.161151599734927,
-0.157336229071969,-0.146618052698146,-0.102467342342709,-0.0977535951278928,
-0.0963818512050153,-0.0913313288327745,-0.0892469330705607,-0.0879480189146197,
-0.0865309304732562,-0.0845823123318504,-0.0799933255352574,-0.0598141466092381,
-0.0212971210955963,-0.0157234450070977,-0.0121263351176517,-0.010839559275635,
-0.0100924296425617,-0.00934771185438471,-0.0085762850858009,-0.00755523319220333,
-0.00487600720888848,-0.000459481853183011),.UNSPECIFIED.);
#211=B_SPLINE_CURVE_WITH_KNOTS('',3,(#17345,#17346,#17347,#17348,#17349,
#17350,#17351,#17352,#17353,#17354,#17355,#17356,#17357,#17358,#17359,#17360,
#17361,#17362,#17363,#17364,#17365,#17366,#17367,#17368,#17369,#17370,#17371,
#17372,#17373,#17374,#17375,#17376,#17377,#17378,#17379,#17380,#17381,#17382,
#17383,#17384,#17385,#17386,#17387,#17388,#17389,#17390,#17391,#17392,#17393,
#17394,#17395,#17396,#17397,#17398,#17399,#17400,#17401,#17402,#17403,#17404,
#17405,#17406,#17407,#17408,#17409,#17410,#17411,#17412,#17413,#17414,#17415,
#17416,#17417,#17418,#17419,#17420,#17421,#17422,#17423,#17424,#17425,#17426,
#17427,#17428,#17429,#17430,#17431,#17432,#17433,#17434,#17435,#17436,#17437,
#17438,#17439,#17440,#17441,#17442,#17443,#17444,#17445,#17446,#17447,#17448,
#17449,#17450,#17451,#17452,#17453,#17454,#17455,#17456,#17457,#17458,#17459,
#17460,#17461,#17462,#17463,#17464,#17465,#17466,#17467,#17468,#17469,#17470,
#17471,#17472,#17473,#17474,#17475,#17476,#17477,#17478,#17479,#17480,#17481,
#17482,#17483,#17484,#17485,#17486,#17487,#17488,#17489,#17490,#17491,#17492,
#17493,#17494,#17495,#17496,#17497,#17498,#17499,#17500,#17501,#17502,#17503,
#17504,#17505,#17506,#17507,#17508,#17509,#17510,#17511,#17512,#17513,#17514,
#17515,#17516,#17517,#17518,#17519,#17520,#17521,#17522,#17523,#17524,#17525,
#17526,#17527,#17528,#17529,#17530),.UNSPECIFIED.,.F.,.F.,(4,2,2,2,2,2,
2,2,2,2,2,2,2,2,2,2,2,2,2,2,2,2,2,2,2,2,2,2,2,2,2,2,2,2,2,2,2,2,2,2,2,2,
2,2,2,2,2,2,2,2,2,2,2,2,2,2,2,2,2,2,2,2,2,2,2,2,2,2,2,2,2,2,2,2,2,2,2,2,
2,2,2,2,2,2,2,2,2,2,2,2,2,2,4),(-1.96178823063968,-1.92015699406122,-1.90104139823297,
-1.89658339907792,-1.89465740191917,-1.89324437179041,-1.89194049343592,
-1.88982885555551,-1.88461498903075,-1.84869964983826,-1.83327427643038,
-1.82348284810212,-1.81989464023885,-1.81812876418854,-1.81669536810835,
-1.81583137222111,-1.81507790016888,-1.81407815074661,-1.81199389798747,
-1.79436181259743,-1.76411834203387,-1.74534114677007,-1.74092567319364,
-1.73900706389289,-1.73759528314338,-1.73628961625884,-1.73416848131252,
-1.72889877204048,-1.69502507656166,-1.66623881527138,-1.66350831021409,
-1.66205520395792,-1.66111123142317,-1.66021681130518,-1.65946299734386,
-1.65848227298375,-1.65649435351309,-1.6431401767911,-1.59861881564175,
-1.58694975974644,-1.58421546658385,-1.58263072343693,-1.58124634635177,
-1.5795352612272,-1.57691608073556,-1.56471176216921,-1.55908942658897,
-1.51480330668824,-1.5070408173816,-1.50542125590241,-1.50451773517547,
-1.50374250353335,-1.50276178788567,-1.50077407465394,-1.48739112055412,
-1.44282019076947,-1.43121612435183,-1.42848642732634,-1.42690264174766,
-1.42551808233169,-1.4238054566201,-1.4211814603269,-1.40891309222829,-1.40334741525865,
-1.35901717229993,-1.35130564644038,-1.34968916141231,-1.34878628134226,
-1.34801093431948,-1.34702921827301,-1.34510110748023,-1.33270418476113,
-1.31888114158313,-1.29467058921394,-1.28242488009734,-1.27483782931146,
-1.27247227047646,-1.27096887426272,-1.26956618003006,-1.26773610090895,
-1.2646582394983,-1.24147854779099,-1.21236935210413,-1.20129373442427,
-1.19542203295883,-1.19393806266891,-1.19306438676141,-1.19228410124699,
-1.19127301784116,-1.18958454059045,-1.17903123747843,-1.16454368588016,
-1.16053736820673),.UNSPECIFIED.);
#212=B_SPLINE_CURVE_WITH_KNOTS('',3,(#17536,#17537,#17538,#17539,#17540,
#17541,#17542,#17543,#17544,#17545,#17546,#17547,#17548,#17549,#17550,#17551,
#17552,#17553,#17554,#17555,#17556,#17557,#17558,#17559,#17560,#17561,#17562,
#17563,#17564,#17565,#17566,#17567,#17568,#17569,#17570,#17571,#17572,#17573,
#17574,#17575,#17576,#17577,#17578,#17579,#17580,#17581,#17582,#17583,#17584,
#17585,#17586,#17587,#17588,#17589,#17590,#17591,#17592,#17593,#17594,#17595,
#17596,#17597,#17598,#17599,#17600,#17601,#17602,#17603,#17604,#17605,#17606,
#17607,#17608,#17609,#17610,#17611,#17612,#17613,#17614,#17615,#17616,#17617,
#17618,#17619,#17620,#17621,#17622,#17623,#17624,#17625,#17626,#17627,#17628,
#17629,#17630,#17631,#17632,#17633,#17634,#17635,#17636,#17637,#17638,#17639,
#17640,#17641,#17642,#17643,#17644,#17645,#17646,#17647,#17648,#17649,#17650,
#17651,#17652,#17653,#17654,#17655,#17656,#17657,#17658,#17659,#17660,#17661,
#17662,#17663,#17664,#17665,#17666,#17667,#17668,#17669,#17670,#17671,#17672,
#17673,#17674,#17675,#17676,#17677,#17678,#17679,#17680,#17681,#17682,#17683,
#17684,#17685,#17686,#17687,#17688,#17689,#17690,#17691,#17692,#17693,#17694,
#17695,#17696,#17697,#17698,#17699,#17700,#17701,#17702,#17703,#17704,#17705,
#17706,#17707,#17708,#17709,#17710,#17711,#17712,#17713,#17714,#17715,#17716,
#17717,#17718,#17719,#17720,#17721,#17722,#17723,#17724,#17725,#17726,#17727,
#17728,#17729,#17730,#17731,#17732,#17733),.UNSPECIFIED.,.F.,.F.,(4,2,2,
2,2,2,2,2,2,2,2,2,2,2,2,2,2,2,2,2,2,2,2,2,2,2,2,2,2,2,2,2,2,2,2,2,2,2,2,
2,2,2,2,2,2,2,2,2,2,2,2,2,2,2,2,2,2,2,2,2,2,2,2,2,2,2,2,2,2,2,2,2,2,2,2,
2,2,2,2,2,2,2,2,2,2,2,2,2,2,2,2,2,2,2,2,2,2,2,4),(-0.801672621689487,-0.775144182679054,
-0.769558497734334,-0.75732586504302,-0.754704200883258,-0.752992228277144,
-0.751607626219412,-0.750023163594684,-0.747290707428512,-0.735650342531249,
-0.691076411964111,-0.677723443498291,-0.675736537216563,-0.674755920727979,
-0.673980620461586,-0.67307683269042,-0.67145632385569,-0.663679860789934,
-0.619421328508415,-0.613711974726309,-0.601616336646214,-0.599004287325825,
-0.597295252096799,-0.595910804465792,-0.594324076968803,-0.591581530517489,
-0.579801835198178,-0.535324611137639,-0.522027055396067,-0.52004190189089,
-0.519061611475709,-0.518286304966448,-0.517382206407886,-0.515760382976406,
-0.507963239039879,-0.463719149825019,-0.457985908889692,-0.445916111521329,
-0.443305741762336,-0.441597187556258,-0.440212718384911,-0.438625513623674,
-0.435880993582319,-0.424074757022352,-0.37961391895947,-0.366326410313487,
-0.364341521434044,-0.363361258732845,-0.36258592368456,-0.361681733838776,
-0.36005960183359,-0.352258220424035,-0.308015335822943,-0.302277287353168,
-0.290212044304654,-0.287601906750548,-0.285893385271818,-0.284508863239945,
-0.284505233120815,-0.284501622843,-0.284498032687251,-0.284494462499623,
-0.284490912124095,-0.284487381397944,-0.284483870163517,-0.284480378246844,
-0.28291413008154,-0.280241645731619,-0.27698387756458,-0.270338009310462,
-0.225060705621588,-0.222075040441391,-0.210493825268747,-0.208597380244882,
-0.207622216437789,-0.206847034817886,-0.2059385375939,-0.204297361303713,
-0.196295979583224,-0.152205410590055,-0.146209464900609,-0.134423586151869,
-0.131579679617832,-0.129953211020496,-0.128708796484505,-0.127401460849067,
-0.125044302867417,-0.117092862636708,-0.103964735537841,-0.0903323947878016,
-0.0570799980975347,-0.0536073648076114,-0.0523386097532334,-0.0515948163220773,
-0.050805735689954,-0.0497205564985315,-0.0471733757100796,-0.0436217126386154,
-0.00046026236518319),.UNSPECIFIED.);
#213=B_SPLINE_CURVE_WITH_KNOTS('',3,(#17734,#17735,#17736,#17737,#17738,
#17739,#17740,#17741,#17742,#17743,#17744,#17745,#17746,#17747,#17748,#17749,
#17750,#17751,#17752,#17753,#17754,#17755,#17756,#17757,#17758,#17759,#17760,
#17761,#17762,#17763,#17764,#17765,#17766,#17767,#17768,#17769,#17770,#17771,
#17772,#17773,#17774,#17775,#17776,#17777,#17778,#17779,#17780,#17781),
 .UNSPECIFIED.,.F.,.F.,(4,2,2,2,2,2,2,2,2,2,2,2,2,2,2,2,2,2,2,2,2,2,2,4),
(-1.96112458302763,-1.94650977042956,-1.93972955151073,-1.93754441074125,
-1.9360235449391,-1.93472568696693,-1.93333684428161,-1.93157344354963,
-1.92878304301402,-1.91379416887626,-1.90485058299271,-1.87332820087799,
-1.86113603460614,-1.85833953920825,-1.85721326624138,-1.85641730739077,
-1.85568487705038,-1.85447230686389,-1.85135806380523,-1.81512123989301,
-1.79437839984539,-1.78721392420322,-1.78377585719125,-1.78189016740401),
 .UNSPECIFIED.);
#214=B_SPLINE_CURVE_WITH_KNOTS('',3,(#17782,#17783,#17784,#17785,#17786,
#17787,#17788,#17789,#17790,#17791,#17792,#17793,#17794,#17795,#17796,#17797,
#17798,#17799,#17800,#17801,#17802,#17803,#17804,#17805,#17806,#17807,#17808,
#17809,#17810,#17811,#17812,#17813,#17814,#17815,#17816,#17817,#17818,#17819,
#17820,#17821,#17822,#17823,#17824,#17825,#17826,#17827,#17828,#17829,#17830,
#17831,#17832,#17833,#17834,#17835,#17836,#17837,#17838,#17839,#17840,#17841,
#17842,#17843,#17844,#17845,#17846,#17847,#17848,#17849,#17850,#17851,#17852,
#17853,#17854,#17855,#17856,#17857,#17858,#17859,#17860,#17861,#17862,#17863,
#17864,#17865,#17866,#17867,#17868,#17869,#17870,#17871,#17872,#17873,#17874,
#17875,#17876,#17877,#17878,#17879,#17880,#17881,#17882,#17883,#17884,#17885,
#17886,#17887,#17888,#17889,#17890,#17891,#17892,#17893,#17894,#17895,#17896,
#17897,#17898,#17899,#17900,#17901,#17902,#17903,#17904,#17905,#17906,#17907,
#17908,#17909,#17910,#17911,#17912,#17913,#17914,#17915,#17916,#17917,#17918,
#17919,#17920,#17921,#17922,#17923,#17924,#17925,#17926,#17927,#17928,#17929,
#17930,#17931,#17932,#17933,#17934,#17935,#17936,#17937,#17938,#17939,#17940,
#17941,#17942,#17943,#17944,#17945,#17946,#17947,#17948,#17949,#17950,#17951,
#17952,#17953,#17954,#17955,#17956,#17957,#17958,#17959,#17960,#17961,#17962,
#17963,#17964,#17965,#17966,#17967,#17968,#17969,#17970,#17971,#17972,#17973,
#17974,#17975,#17976,#17977,#17978,#17979,#17980,#17981,#17982,#17983,#17984,
#17985,#17986,#17987,#17988,#17989,#17990,#17991,#17992,#17993,#17994,#17995,
#17996,#17997,#17998,#17999,#18000,#18001,#18002,#18003,#18004,#18005,#18006,
#18007,#18008,#18009,#18010,#18011,#18012,#18013,#18014,#18015,#18016,#18017,
#18018,#18019,#18020,#18021,#18022,#18023,#18024,#18025,#18026,#18027,#18028,
#18029,#18030,#18031,#18032,#18033,#18034,#18035,#18036,#18037,#18038,#18039,
#18040,#18041,#18042,#18043,#18044,#18045,#18046,#18047,#18048,#18049,#18050,
#18051,#18052,#18053,#18054,#18055,#18056,#18057,#18058,#18059,#18060,#18061,
#18062,#18063,#18064,#18065,#18066,#18067,#18068,#18069,#18070,#18071,#18072,
#18073,#18074,#18075,#18076,#18077,#18078,#18079,#18080,#18081,#18082,#18083,
#18084,#18085,#18086,#18087,#18088,#18089,#18090,#18091,#18092,#18093,#18094,
#18095),.UNSPECIFIED.,.F.,.F.,(4,2,2,2,2,2,2,2,2,2,2,2,2,2,2,2,2,2,2,2,
2,2,2,2,2,2,2,2,2,2,2,2,2,2,2,2,2,2,2,2,2,2,2,2,2,2,2,2,2,2,2,2,2,2,2,2,
2,2,2,2,2,2,2,2,2,2,2,2,2,2,2,2,2,2,2,2,2,2,2,2,2,2,2,2,2,2,2,2,2,2,2,2,
2,2,2,2,2,2,2,2,2,2,2,2,2,2,2,2,2,2,2,2,2,2,2,2,2,2,2,2,2,2,2,2,2,2,2,2,
2,2,2,2,2,2,2,2,2,2,2,2,2,2,2,2,2,2,2,2,2,2,2,2,2,2,2,2,4),(-1.16053736820673,
-1.14155815964385,-1.12262370826275,-1.11818787834328,-1.11626542160771,
-1.1148527039373,-1.11354750528723,-1.11143012648783,-1.10618429468265,
-1.07115027688277,-1.04338728244901,-1.03937817628469,-1.03808178962915,
-1.03724980244178,-1.03646175234525,-1.03551255964686,-1.03314070731746,
-1.03074109444545,-0.981266927380947,-0.964910049662874,-0.962050028113323,
-0.960265031946295,-0.958873087586267,-0.957333903794165,-0.954806484486732,
-0.945651907420497,-0.902262580384309,-0.900879376749887,-0.896366698843762,
-0.884722707525326,-0.882824190943104,-0.881848758487983,-0.881073783782946,
-0.880166028795487,-0.878527470302939,-0.870450963910527,-0.826429064686011,
-0.820424586876839,-0.808646563137754,-0.805803843465067,-0.804177951625829,
-0.802933927440493,-0.801328349738844,-0.798500164359894,-0.785445033080755,
-0.757288914631586,-0.756182832547103,-0.729242380066489,-0.727174744855765,
-0.726178112915842,-0.725401437698846,-0.724508811973903,-0.722939242715166,
-0.715944819510251,-0.672590954487486,-0.663571659366365,-0.663214084012877,
-0.661994174597095,-0.6525600816973,-0.649893889702218,-0.648323991814367,
-0.647076235546957,-0.645407525343655,-0.642285890848176,-0.623144525344255,
-0.58850660682205,-0.585022630618363,-0.573311684574237,-0.571410687320906,
-0.570434775373894,-0.569659836240935,-0.568752604340327,-0.567116207485564,
-0.559074637616738,-0.515030380572884,-0.509070757387959,-0.497245384464062,
-0.494399036238392,-0.492772408113018,-0.491528522966139,-0.48992395340734,
-0.487099945201931,-0.47410791847647,-0.446197570720464,-0.419931568170017,
-0.416437416087385,-0.415165626904609,-0.414421444616375,-0.413633116021297,
-0.412550870143094,-0.41001907495101,-0.388318914107292,-0.372381273155706,
-0.342596675566372,-0.339162386234467,-0.337405528570271,-0.336016823750962,
-0.336013415619075,-0.336010035654314,-0.336006683876058,-0.336003360004943,
-0.336000063797418,-0.33599679501583,-0.335993553405864,-0.335991052557717,
-0.335988556945046,-0.335986066159208,-0.335983580167727,-0.335981098972663,
-0.335978622572367,-0.3359761509534,-0.335973684074507,-0.335971221928687,
-0.335968764492674,-0.335966311772249,-0.335963863778011,-0.335961420468532,
-0.335958981821319,-0.335956547844142,-0.335954118517713,-0.335951693815784,
-0.335949273735142,-0.33594685825989,-0.335944447374503,-0.335942041076944,
-0.335939639347168,-0.335937242169554,-0.335934849532215,-0.335932461432634,
-0.335930077845004,-0.335927698773454,-0.335925324174456,-0.334370672665213,
-0.331724708510753,-0.328522327768988,-0.322032194702877,-0.277400704373564,
-0.273687125657739,-0.261924110268713,-0.260021026873319,-0.259044641389193,
-0.258269638856414,-0.257362693855451,-0.255727726428632,-0.247711272327178,
-0.203645198076067,-0.197717935825418,-0.185856273980575,-0.183006933107235,
-0.181379578020498,-0.180135652199593,-0.180125392469073,-0.180115487169854,
-0.180105926541083,-0.180096699279647,-0.180087790648967,-0.179857088658834),
 .UNSPECIFIED.);
#215=B_SPLINE_CURVE_WITH_KNOTS('',3,(#18100,#18101,#18102,#18103,#18104,
#18105,#18106,#18107,#18108,#18109,#18110,#18111,#18112,#18113,#18114,#18115,
#18116,#18117,#18118,#18119,#18120,#18121,#18122,#18123,#18124,#18125,#18126,
#18127,#18128,#18129,#18130,#18131,#18132,#18133,#18134,#18135,#18136,#18137,
#18138,#18139,#18140,#18141,#18142,#18143,#18144,#18145,#18146,#18147,#18148,
#18149,#18150,#18151,#18152,#18153,#18154,#18155,#18156,#18157,#18158,#18159,
#18160,#18161,#18162,#18163,#18164,#18165,#18166,#18167,#18168,#18169,#18170,
#18171,#18172,#18173,#18174,#18175,#18176,#18177,#18178,#18179,#18180,#18181,
#18182,#18183,#18184,#18185,#18186,#18187,#18188,#18189,#18190,#18191,#18192,
#18193,#18194,#18195,#18196,#18197,#18198,#18199,#18200,#18201,#18202,#18203,
#18204,#18205,#18206,#18207,#18208,#18209,#18210,#18211,#18212,#18213,#18214,
#18215,#18216,#18217,#18218,#18219,#18220,#18221,#18222,#18223,#18224,#18225,
#18226,#18227,#18228,#18229,#18230,#18231,#18232,#18233,#18234,#18235,#18236,
#18237,#18238,#18239,#18240,#18241,#18242,#18243,#18244,#18245,#18246,#18247,
#18248,#18249,#18250,#18251,#18252,#18253,#18254,#18255,#18256,#18257,#18258,
#18259,#18260,#18261,#18262,#18263,#18264,#18265,#18266,#18267,#18268,#18269,
#18270,#18271,#18272,#18273,#18274,#18275,#18276,#18277,#18278,#18279,#18280,
#18281,#18282,#18283,#18284,#18285,#18286,#18287,#18288,#18289,#18290,#18291,
#18292,#18293,#18294,#18295,#18296,#18297,#18298,#18299,#18300,#18301,#18302,
#18303,#18304,#18305,#18306,#18307,#18308,#18309,#18310,#18311,#18312,#18313,
#18314,#18315,#18316,#18317,#18318,#18319,#18320,#18321,#18322,#18323,#18324,
#18325,#18326,#18327,#18328,#18329,#18330,#18331,#18332,#18333,#18334,#18335,
#18336,#18337,#18338,#18339,#18340,#18341),.UNSPECIFIED.,.F.,.F.,(4,2,2,
2,2,2,2,2,2,2,2,2,2,2,2,2,2,2,2,2,2,2,2,2,2,2,2,2,2,2,2,2,2,2,2,2,2,2,2,
2,2,2,2,2,2,2,2,2,2,2,2,2,2,2,2,2,2,2,2,2,2,2,2,2,2,2,2,2,2,2,2,2,2,2,2,
2,2,2,2,2,2,2,2,2,2,2,2,2,2,2,2,2,2,2,2,2,2,2,2,2,2,2,2,2,2,2,2,2,2,2,2,
2,2,2,2,2,2,2,2,2,4),(-1.78172815281824,-1.77253372019698,-1.76631370808231,
-1.76480570691446,-1.7639201043268,-1.76314274020048,-1.76213622478509,
-1.76049885300652,-1.75098779831253,-1.74641201713466,-1.74269643920981,
-1.69942310822093,-1.69342224665427,-1.68904750588581,-1.68713860201849,
-1.6857220330961,-1.68442354327318,-1.68267268132171,-1.67839240588933,
-1.67456158001473,-1.670979313909,-1.67029906550083,-1.66125482516073,-1.61780714154226,
-1.61079304046626,-1.6092225582893,-1.60832996284903,-1.60755365809344,
-1.6065579439109,-1.60449371496109,-1.577463354171,-1.54857547056023,-1.53534094091444,
-1.53250242558939,-1.53089498173639,-1.52965138168029,-1.52802871193439,
-1.52519838164536,-1.51356354338677,-1.50743475020068,-1.46342973770787,
-1.45531820383914,-1.45367798002095,-1.45277004835105,-1.45199536982876,
-1.45102086970807,-1.44912580534688,-1.43755455489337,-1.40007365989095,
-1.38690550936001,-1.37891137868578,-1.37650129676547,-1.37498836004355,
-1.37358962189756,-1.37178284693218,-1.36878381809816,-1.34890082833157,
-1.30631432665826,-1.29953938942786,-1.29798547850884,-1.29709639563306,
-1.29631932470044,-1.29531760128442,-1.29369671814283,-1.28451322332276,
-1.2816370041638,-1.24423088930667,-1.2312006579526,-1.22326641013149,-1.22086263665544,
-1.21935098716401,-1.21795161020848,-1.21614143787634,-1.21313117111143,
-1.19280221892162,-1.1505455793434,-1.14388510284953,-1.14233938100341,
-1.14145204825295,-1.14067459181924,-1.13966984225465,-1.13756041877337,
-1.11792532820679,-1.08985518461517,-1.07097999978118,-1.06655189688075,
-1.06463088112568,-1.06321849438777,-1.06191308656034,-1.05979420877457,
-1.05453894974272,-1.01993907672026,-1.00403900251007,-0.993713453888721,
-0.989993277386549,-0.987353145567405,-0.986252355937933,-0.985460789879611,
-0.984721658564797,-0.983683318547428,-0.980930955099377,-0.967258431406432,
-0.949810773628827,-0.916692347775683,-0.911416131731427,-0.909293675577322,
-0.90798761113116,-0.906575718096371,-0.904657524327172,-0.900245519868065,
-0.88149482297644,-0.851082879833142,-0.845864837668614,-0.833362401812989,
-0.831430138514274,-0.830447532049146,-0.829672110324767,-0.828769845520952,
-0.827156202273705,-0.819490080623062,-0.801672621689487),.UNSPECIFIED.);
#216=B_SPLINE_CURVE_WITH_KNOTS('',3,(#18343,#18344,#18345,#18346,#18347,
#18348,#18349,#18350,#18351,#18352,#18353,#18354,#18355,#18356,#18357,#18358,
#18359,#18360,#18361,#18362,#18363,#18364,#18365,#18366,#18367,#18368,#18369,
#18370,#18371,#18372,#18373,#18374,#18375,#18376,#18377,#18378,#18379,#18380,
#18381,#18382,#18383,#18384,#18385,#18386,#18387,#18388,#18389,#18390),
 .UNSPECIFIED.,.F.,.F.,(4,2,2,2,2,2,2,2,2,2,2,2,2,2,2,2,2,2,2,2,2,2,2,4),
(-0.179857088658834,-0.178497778536323,-0.17570120334603,-0.172268087202898,
-0.165118744853604,-0.144450508006672,-0.108014815567082,-0.104902711334605,
-0.103690147151367,-0.10295747702479,-0.102161045916296,-0.101033764902274,
-0.0982330428526651,-0.0859987301545725,-0.0519637944323866,-0.0431570796128006,
-0.03031520294166,-0.0276534749732519,-0.0259290526584936,-0.0245433855940571,
-0.0232415172836668,-0.0216956360921947,-0.0194501360584109,-0.000459478261909778),
 .UNSPECIFIED.);
#217=B_SPLINE_CURVE_WITH_KNOTS('',3,(#18391,#18392,#18393,#18394,#18395,
#18396,#18397,#18398,#18399,#18400,#18401,#18402,#18403,#18404,#18405,#18406,
#18407,#18408,#18409,#18410,#18411,#18412,#18413,#18414,#18415,#18416,#18417,
#18418,#18419,#18420,#18421,#18422,#18423,#18424,#18425,#18426,#18427,#18428,
#18429,#18430,#18431,#18432,#18433,#18434,#18435,#18436,#18437,#18438,#18439,
#18440,#18441,#18442,#18443,#18444,#18445,#18446,#18447,#18448,#18449,#18450,
#18451,#18452,#18453,#18454,#18455,#18456,#18457,#18458,#18459,#18460,#18461,
#18462,#18463,#18464,#18465,#18466,#18467,#18468,#18469,#18470,#18471,#18472,
#18473,#18474,#18475,#18476,#18477,#18478,#18479,#18480,#18481,#18482,#18483,
#18484,#18485,#18486,#18487,#18488,#18489,#18490,#18491,#18492,#18493,#18494,
#18495,#18496,#18497,#18498,#18499,#18500,#18501,#18502,#18503,#18504,#18505,
#18506,#18507,#18508,#18509,#18510,#18511,#18512,#18513,#18514,#18515,#18516,
#18517,#18518,#18519,#18520,#18521,#18522,#18523,#18524,#18525,#18526,#18527,
#18528,#18529,#18530,#18531,#18532,#18533,#18534,#18535,#18536,#18537,#18538,
#18539,#18540,#18541,#18542,#18543,#18544,#18545,#18546,#18547,#18548,#18549,
#18550,#18551,#18552,#18553,#18554,#18555,#18556,#18557,#18558,#18559,#18560,
#18561,#18562,#18563,#18564,#18565,#18566,#18567,#18568,#18569,#18570,#18571,
#18572,#18573,#18574,#18575,#18576,#18577,#18578,#18579,#18580,#18581,#18582,
#18583,#18584,#18585,#18586,#18587,#18588,#18589,#18590,#18591,#18592,#18593,
#18594,#18595,#18596,#18597,#18598,#18599,#18600),.UNSPECIFIED.,.F.,.F.,
(4,2,2,2,2,2,2,2,2,2,2,2,2,2,2,2,2,2,2,2,2,2,2,2,2,2,2,2,2,2,2,2,2,2,2,
2,2,2,2,2,2,2,2,2,2,2,2,2,2,2,2,2,2,2,2,2,2,2,2,2,2,2,2,2,2,2,2,2,2,2,2,
2,2,2,2,2,2,2,2,2,2,2,2,2,2,2,2,2,2,2,2,2,2,2,2,2,2,2,2,2,2,2,2,2,4),(-1.96079121561173,
-1.91694482162004,-1.91024146039047,-1.90869345153882,-1.90780605107279,
-1.90702935167909,-1.90602667259015,-1.90392545789794,-1.88480510825376,
-1.86489414423652,-1.84667203000836,-1.83880113263009,-1.83512296427284,
-1.83217578327906,-1.83054790398943,-1.83053360022794,-1.83051903681914,
-1.83050420539703,-1.83048909725358,-1.83047370331781,-1.83045801352482,
-1.83044201745044,-1.830425706684,-1.83041455064203,-1.83040235418818,-1.83038901082079,
-1.83037440138794,-1.83035839225484,-1.82897501105994,-1.82726802395791,
-1.82466045321368,-1.81261263536704,-1.80685955812779,-1.76269065445403,
-1.7548171464742,-1.75319147251431,-1.75228692665544,-1.75151228166359,
-1.75053418571882,-1.74899038080902,-1.7411403549141,-1.70476034992802,
-1.68236974208065,-1.67906858564697,-1.6763664185471,-1.67479487218404,
-1.67355170692737,-1.67192590954822,-1.66908072181032,-1.65725628704226,
-1.65129912473464,-1.60725393172834,-1.5992157412494,-1.59758012270399,
-1.59667334666993,-1.59589880898111,-1.59492342274383,-1.59302350816615,
-1.58131972043172,-1.57766139359075,-1.53300710403504,-1.52313826341641,
-1.52054725289542,-1.51899456060461,-1.51760638917655,-1.51584807551323,
-1.51240420339761,-1.48353506331741,-1.46648374147773,-1.44500197000472,
-1.44247165961581,-1.44139003310733,-1.44060215146508,-1.43985838708379,
-1.43858730386408,-1.43509507960738,-1.40894868923879,-1.38100156106593,
-1.36800274037116,-1.365179410787,-1.36357552072257,-1.36233229776347,-1.36070673491446,
-1.35786274847095,-1.34605424190649,-1.34008185195058,-1.29604389366619,
-1.28799375367975,-1.28635738497572,-1.28545042308891,-1.2846758668287,
-1.28370063596442,-1.28180155177318,-1.27012057123348,-1.25369578333642,
-1.22547135538671,-1.21240125801682,-1.2095731164756,-1.20796801724572,
-1.2067245741268,-1.20509974776509,-1.20225965961727,-1.19050327604798,
-1.1844805867176,-1.1601095629489),.UNSPECIFIED.);
#218=B_SPLINE_CURVE_WITH_KNOTS('',3,(#18606,#18607,#18608,#18609,#18610,
#18611,#18612,#18613,#18614,#18615,#18616,#18617,#18618,#18619,#18620,#18621,
#18622,#18623,#18624,#18625,#18626,#18627,#18628,#18629,#18630,#18631,#18632,
#18633,#18634,#18635,#18636,#18637,#18638,#18639,#18640,#18641,#18642,#18643,
#18644,#18645,#18646,#18647,#18648,#18649,#18650,#18651,#18652,#18653,#18654,
#18655,#18656,#18657,#18658,#18659,#18660,#18661,#18662,#18663,#18664,#18665,
#18666,#18667,#18668,#18669,#18670,#18671,#18672,#18673,#18674,#18675,#18676,
#18677,#18678,#18679,#18680,#18681,#18682,#18683,#18684,#18685,#18686,#18687,
#18688,#18689,#18690,#18691,#18692,#18693,#18694,#18695,#18696,#18697,#18698,
#18699,#18700,#18701,#18702,#18703,#18704,#18705,#18706,#18707,#18708,#18709,
#18710,#18711,#18712,#18713,#18714,#18715,#18716,#18717,#18718,#18719,#18720,
#18721,#18722,#18723,#18724,#18725,#18726,#18727,#18728,#18729,#18730,#18731,
#18732,#18733,#18734,#18735,#18736,#18737,#18738,#18739,#18740,#18741,#18742,
#18743,#18744,#18745,#18746,#18747,#18748,#18749,#18750,#18751,#18752,#18753,
#18754,#18755,#18756,#18757,#18758,#18759,#18760,#18761,#18762,#18763,#18764,
#18765,#18766,#18767,#18768,#18769,#18770,#18771,#18772,#18773,#18774,#18775,
#18776,#18777,#18778,#18779,#18780,#18781,#18782,#18783,#18784,#18785,#18786,
#18787,#18788,#18789,#18790,#18791),.UNSPECIFIED.,.F.,.F.,(4,2,2,2,2,2,
2,2,2,2,2,2,2,2,2,2,2,2,2,2,2,2,2,2,2,2,2,2,2,2,2,2,2,2,2,2,2,2,2,2,2,2,
2,2,2,2,2,2,2,2,2,2,2,2,2,2,2,2,2,2,2,2,2,2,2,2,2,2,2,2,2,2,2,2,2,2,2,2,
2,2,2,2,2,2,2,2,2,2,2,2,2,2,4),(-0.801883478262616,-0.796942743005185,-0.767998750680466,
-0.740967488840241,-0.738901381511447,-0.737904955494984,-0.737128189429027,
-0.73623516297459,-0.734664170188142,-0.727651551007394,-0.684215617767987,
-0.675179910689682,-0.674564397621058,-0.671555310128778,-0.664859244302258,
-0.662179926777577,-0.660449958259594,-0.659063645598381,-0.657491113644681,
-0.654813712089845,-0.643911738186813,-0.598774695165539,-0.585139571457424,
-0.583143321661039,-0.582160704583504,-0.581385095862041,-0.580482408693454,
-0.578867502150835,-0.571185944167539,-0.526839180605354,-0.521237384782666,
-0.509017953759545,-0.506396687844682,-0.504684598640432,-0.503299652438316,
-0.501714521962304,-0.498980221802812,-0.487321310764517,-0.442746563208531,
-0.429396212262029,-0.427408978772931,-0.42642814162249,-0.425652637927385,
-0.424748579728398,-0.423127503005166,-0.415346742533404,-0.371078218393625,
-0.365364769018602,-0.353268784117248,-0.350656234532991,-0.348946804686762,
-0.347561992616929,-0.345974798180025,-0.343231319709185,-0.331445659475355,
-0.286958584810694,-0.273658640608339,-0.271672996516007,-0.270692452684378,
-0.269916940281395,-0.26901259534087,-0.267499299905258,-0.264587039832033,
-0.243056010195007,-0.205262123477829,-0.198898661972958,-0.195178796563468,
-0.19338813349005,-0.191995136447937,-0.190458203953769,-0.187973943304827,
-0.179263845213553,-0.164341118946122,-0.142633057238069,-0.130097698415107,
-0.126991715461381,-0.117705944672987,-0.116079246282222,-0.115075574035733,
-0.114298036772574,-0.113409582779292,-0.112474952353912,-0.109114061319104,
-0.0875220680580351,-0.0700306888754584,-0.0428956979680085,-0.0394556561690335,
-0.0376972505485617,-0.0363080017449152,-0.0347530512650087,-0.0331437931308085,
-0.0307454907072447,-0.000459705691028188),.UNSPECIFIED.);
#219=B_SPLINE_CURVE_WITH_KNOTS('',3,(#18792,#18793,#18794,#18795,#18796,
#18797,#18798,#18799,#18800,#18801,#18802,#18803,#18804,#18805,#18806,#18807,
#18808,#18809,#18810,#18811,#18812,#18813,#18814,#18815,#18816,#18817,#18818,
#18819,#18820,#18821,#18822,#18823,#18824,#18825,#18826,#18827,#18828,#18829,
#18830,#18831,#18832,#18833,#18834,#18835),.UNSPECIFIED.,.F.,.F.,(4,2,2,
2,2,2,2,2,2,2,2,2,2,2,2,2,2,2,2,2,2,4),(-1.96072017599113,-1.92534306313198,
-1.92268432270731,-1.92125856958759,-1.92032606841099,-1.91943931152633,
-1.91866220733764,-1.91765771170252,-1.91554810917444,-1.89601694840939,
-1.88267789013014,-1.86761833902883,-1.84962034927292,-1.84481937820509,
-1.84327215882423,-1.84176054561153,-1.84036174603569,-1.83855308551815,
-1.83554699819581,-1.81535510840621,-1.78465470035516,-1.78172815281824),
 .UNSPECIFIED.);
#220=B_SPLINE_CURVE_WITH_KNOTS('',3,(#18836,#18837,#18838,#18839,#18840,
#18841,#18842,#18843,#18844,#18845,#18846,#18847,#18848,#18849,#18850,#18851,
#18852,#18853,#18854,#18855,#18856,#18857,#18858,#18859,#18860,#18861,#18862,
#18863,#18864,#18865,#18866,#18867,#18868,#18869,#18870,#18871,#18872,#18873,
#18874,#18875,#18876,#18877,#18878,#18879,#18880,#18881,#18882,#18883,#18884,
#18885,#18886,#18887,#18888,#18889,#18890,#18891,#18892,#18893,#18894,#18895,
#18896,#18897,#18898,#18899,#18900,#18901,#18902,#18903,#18904,#18905,#18906,
#18907,#18908,#18909,#18910,#18911,#18912,#18913,#18914,#18915,#18916,#18917,
#18918,#18919,#18920,#18921,#18922,#18923,#18924,#18925,#18926,#18927,#18928,
#18929,#18930,#18931,#18932,#18933,#18934,#18935,#18936,#18937,#18938,#18939,
#18940,#18941,#18942,#18943,#18944,#18945,#18946,#18947,#18948,#18949,#18950,
#18951,#18952,#18953,#18954,#18955,#18956,#18957,#18958,#18959,#18960,#18961,
#18962,#18963,#18964,#18965,#18966,#18967,#18968,#18969,#18970,#18971,#18972,
#18973,#18974,#18975,#18976,#18977,#18978,#18979,#18980,#18981,#18982,#18983,
#18984,#18985,#18986,#18987,#18988,#18989,#18990,#18991,#18992,#18993,#18994,
#18995,#18996,#18997,#18998,#18999,#19000,#19001,#19002,#19003,#19004,#19005,
#19006,#19007,#19008,#19009,#19010,#19011,#19012,#19013,#19014,#19015,#19016,
#19017,#19018,#19019,#19020,#19021,#19022,#19023,#19024,#19025,#19026,#19027,
#19028,#19029,#19030,#19031,#19032,#19033,#19034,#19035,#19036,#19037,#19038,
#19039,#19040,#19041,#19042,#19043,#19044,#19045,#19046,#19047,#19048,#19049,
#19050,#19051,#19052,#19053,#19054,#19055,#19056,#19057,#19058,#19059,#19060,
#19061,#19062,#19063,#19064,#19065,#19066,#19067,#19068,#19069),
 .UNSPECIFIED.,.F.,.F.,(4,2,2,2,2,2,2,2,2,2,2,2,2,2,2,2,2,2,2,2,2,2,2,2,
2,2,2,2,2,2,2,2,2,2,2,2,2,2,2,2,2,2,2,2,2,2,2,2,2,2,2,2,2,2,2,2,2,2,2,2,
2,2,2,2,2,2,2,2,2,2,2,2,2,2,2,2,2,2,2,2,2,2,2,2,2,2,2,2,2,2,2,2,2,2,2,2,
2,2,2,2,2,2,2,2,2,2,2,2,2,2,2,2,2,2,2,2,4),(-1.1601095629489,-1.1404650525258,
-1.13237572786878,-1.13073687955802,-1.12982929081243,-1.12905465409522,
-1.12807990159606,-1.12618345773339,-1.11457559580012,-1.07724042304681,
-1.06399017827743,-1.0559603656158,-1.05354655589803,-1.0520328730841,-1.05063453424885,
-1.04882980490709,-1.04583749899097,-1.02622801104323,-0.988594891105816,
-0.980809613121384,-0.976307668925648,-0.974900345686425,-0.974043914980851,
-0.973258842803546,-0.972195847416052,-0.96977273851594,-0.966440876724249,
-0.957653145476374,-0.93386959672387,-0.902178664417379,-0.8987606748163,
-0.897007533974661,-0.895619493901943,-0.894062802945646,-0.891455262193384,
-0.881401582164383,-0.83623703230447,-0.833815652136543,-0.830211896673024,
-0.821308612170261,-0.819702646049156,-0.818705428116093,-0.81792881779091,
-0.817036853937235,-0.815469847794772,-0.808509526507781,-0.765294850933047,
-0.756303361201351,-0.745360590599289,-0.742585852902515,-0.740975784205431,
-0.739593272782693,-0.737914597473864,-0.734744894894185,-0.714184409329306,
-0.681456569453589,-0.677682987468375,-0.665875346229079,-0.66397087699806,
-0.662994326133177,-0.662219477553941,-0.66131304202802,-0.65967982366322,
-0.65168835055567,-0.607614474778559,-0.60171790077584,-0.589826837129825,
-0.58722925799045,-0.585524905486244,-0.5841410598657,-0.582551501768166,
-0.579795101873942,-0.567813626543313,-0.523489243444557,-0.510254944092308,
-0.50827216886184,-0.507292484226493,-0.506517380365583,-0.505613213491227,
-0.503990517728597,-0.496175082211189,-0.451959363234099,-0.446276300213773,
-0.434147243186193,-0.431533199351003,-0.429823705313632,-0.42843945163138,
-0.426853570902119,-0.424114079079006,-0.412372813868788,-0.367878219018491,
-0.354544155891085,-0.352558011656175,-0.351577625690443,-0.350802438795201,
-0.349898717316991,-0.348278174251431,-0.340498829097557,-0.296251868475326,
-0.290610397590587,-0.278433967463194,-0.275816638929641,-0.274106088301622,
-0.272721703927525,-0.271136469616492,-0.268542479953017,-0.258023075418503,
-0.212615783939347,-0.207825182258011,-0.198525129652494,-0.196898032232426,
-0.195894403735116,-0.195117087540541,-0.194229108190455,-0.19271151804396,
-0.186361782024664,-0.17958692698941),.UNSPECIFIED.);
#221=B_SPLINE_CURVE_WITH_KNOTS('',3,(#19074,#19075,#19076,#19077,#19078,
#19079,#19080,#19081,#19082,#19083,#19084,#19085,#19086,#19087,#19088,#19089,
#19090,#19091,#19092,#19093,#19094,#19095,#19096,#19097,#19098,#19099,#19100,
#19101,#19102,#19103,#19104,#19105,#19106,#19107,#19108,#19109,#19110,#19111,
#19112,#19113,#19114,#19115,#19116,#19117,#19118,#19119,#19120,#19121,#19122,
#19123,#19124,#19125,#19126,#19127,#19128,#19129,#19130,#19131,#19132,#19133,
#19134,#19135,#19136,#19137,#19138,#19139,#19140,#19141,#19142,#19143,#19144,
#19145,#19146,#19147,#19148,#19149,#19150,#19151,#19152,#19153,#19154,#19155,
#19156,#19157,#19158,#19159,#19160,#19161,#19162,#19163,#19164,#19165,#19166,
#19167,#19168,#19169,#19170,#19171,#19172,#19173,#19174,#19175,#19176,#19177,
#19178,#19179,#19180,#19181,#19182,#19183,#19184,#19185,#19186,#19187,#19188,
#19189,#19190,#19191,#19192,#19193,#19194,#19195,#19196,#19197,#19198,#19199,
#19200,#19201,#19202,#19203,#19204,#19205,#19206,#19207,#19208,#19209,#19210,
#19211,#19212,#19213,#19214,#19215,#19216,#19217,#19218,#19219,#19220,#19221,
#19222,#19223,#19224,#19225,#19226,#19227,#19228,#19229,#19230,#19231,#19232,
#19233,#19234,#19235,#19236,#19237,#19238,#19239,#19240,#19241,#19242,#19243,
#19244,#19245,#19246,#19247,#19248,#19249,#19250,#19251,#19252,#19253,#19254,
#19255,#19256,#19257,#19258,#19259,#19260,#19261,#19262,#19263,#19264,#19265,
#19266,#19267,#19268,#19269,#19270,#19271,#19272,#19273,#19274,#19275,#19276,
#19277,#19278,#19279,#19280,#19281,#19282,#19283,#19284,#19285,#19286,#19287,
#19288,#19289,#19290,#19291,#19292,#19293,#19294,#19295,#19296,#19297,#19298,
#19299,#19300,#19301,#19302,#19303,#19304,#19305,#19306,#19307),
 .UNSPECIFIED.,.F.,.F.,(4,2,2,2,2,2,2,2,2,2,2,2,2,2,2,2,2,2,2,2,2,2,2,2,
2,2,2,2,2,2,2,2,2,2,2,2,2,2,2,2,2,2,2,2,2,2,2,2,2,2,2,2,2,2,2,2,2,2,2,2,
2,2,2,2,2,2,2,2,2,2,2,2,2,2,2,2,2,2,2,2,2,2,2,2,2,2,2,2,2,2,2,2,2,2,2,2,
2,2,2,2,2,2,2,2,2,2,2,2,2,2,2,2,2,2,2,2,4),(-1.78228100909597,-1.77482955259016,
-1.76157546457646,-1.75354358706471,-1.75112915374112,-1.74961507015703,
-1.7482163518803,-1.74641111671003,-1.74341792728819,-1.72379216544428,
-1.68947185549358,-1.6794652988586,-1.67582352152111,-1.6740387294826,-1.67259712934658,
-1.67177662526936,-1.67100141119668,-1.67002134291365,-1.66803697625781,
-1.65475604767349,-1.61032158914733,-1.59852215776555,-1.59577836884746,
-1.59419143958521,-1.59280712252757,-1.59109864274847,-1.58848815611925,
-1.57641409994712,-1.57068026443617,-1.52641496850095,-1.5186174267709,
-1.51699561896725,-1.51609155444831,-1.51531628971783,-1.51433607356715,
-1.51235113356259,-1.49905549291884,-1.45459439368868,-1.4428285298906,
-1.44008702689787,-1.43850054537812,-1.43711609897054,-1.43540679081641,
-1.43279379356419,-1.42068428332079,-1.41498128613184,-1.37069185440041,
-1.36292075724331,-1.36130050259736,-1.36039674581166,-1.35962140073622,
-1.35864064130474,-1.35665315594087,-1.34328254864858,-1.29868694333994,
-1.28710534855124,-1.28437702223952,-1.2827933875441,-1.28140857209393,
-1.27969512548769,-1.27706892124057,-1.26477079262898,-1.22692422924379,
-1.21370679142639,-1.20710371764126,-1.20556213949451,-1.20467568102094,
-1.20389800485231,-1.20289166686687,-1.20077428181155,-1.17844643690694,
-1.17286361932347,-1.1447137165688,-1.13166047816908,-1.12883237806385,
-1.12722676967467,-1.12598267923159,-1.1243566432211,-1.12151350519676,
-1.10973115048512,-1.10373000261349,-1.05962806983969,-1.05161239979747,
-1.04997727646066,-1.04907020788959,-1.04829507054251,-1.04731846816782,
-1.04541481254306,-1.03364046047982,-1.02758303927016,-0.991002810217955,
-0.981222835820473,-0.980013101003812,-0.974617734268927,-0.972474588927608,
-0.971164473639897,-0.969754916993157,-0.967851749691,-0.963526260266344,
-0.945456019528111,-0.907997699949179,-0.896421646754376,-0.894525635184769,
-0.893550654997816,-0.892775598715743,-0.891867224511571,-0.890226209906355,
-0.88211049886817,-0.838108542293483,-0.831975987186352,-0.820342143876954,
-0.817510873882053,-0.815887452833581,-0.814643168161072,-0.813034705308378,
-0.810194011031848,-0.801883478262616),.UNSPECIFIED.);
#222=B_SPLINE_CURVE_WITH_KNOTS('',3,(#19309,#19310,#19311,#19312,#19313,
#19314,#19315,#19316,#19317,#19318,#19319,#19320,#19321,#19322,#19323,#19324,
#19325,#19326,#19327,#19328,#19329,#19330,#19331,#19332,#19333,#19334,#19335,
#19336,#19337,#19338,#19339,#19340,#19341,#19342,#19343,#19344,#19345,#19346,
#19347,#19348,#19349,#19350),.UNSPECIFIED.,.F.,.F.,(4,2,2,2,2,2,2,2,2,2,
2,2,2,2,2,2,2,2,2,2,4),(-0.17958692698941,-0.17386743549034,-0.145639157150684,
-0.123567275624923,-0.120513468693085,-0.118690452328767,-0.117288958496497,
-0.115782718022685,-0.114243576408732,-0.109533175038598,-0.0901174104874177,
-0.0748291750643691,-0.045346741968868,-0.0418850008757082,-0.0406182111285593,
-0.0398750029645828,-0.0390860743667612,-0.0380003577072798,-0.0367873172160553,
-0.0346756350602518,-0.000459986905719233),.UNSPECIFIED.);
#223=B_SPLINE_CURVE_WITH_KNOTS('',3,(#19351,#19352,#19353,#19354,#19355,
#19356,#19357,#19358,#19359,#19360,#19361,#19362,#19363,#19364,#19365,#19366,
#19367,#19368,#19369,#19370,#19371,#19372,#19373,#19374,#19375,#19376,#19377,
#19378,#19379,#19380,#19381,#19382,#19383,#19384,#19385,#19386,#19387,#19388,
#19389,#19390,#19391,#19392,#19393,#19394,#19395,#19396,#19397,#19398,#19399,
#19400,#19401,#19402,#19403,#19404,#19405,#19406,#19407,#19408,#19409,#19410,
#19411,#19412,#19413,#19414,#19415,#19416,#19417,#19418,#19419,#19420,#19421,
#19422,#19423,#19424,#19425,#19426,#19427,#19428,#19429,#19430,#19431,#19432,
#19433,#19434,#19435,#19436,#19437,#19438,#19439,#19440,#19441,#19442,#19443,
#19444,#19445,#19446,#19447,#19448,#19449,#19450,#19451,#19452,#19453,#19454,
#19455,#19456,#19457,#19458,#19459,#19460,#19461,#19462,#19463,#19464,#19465,
#19466,#19467,#19468,#19469,#19470,#19471,#19472,#19473,#19474,#19475,#19476,
#19477,#19478,#19479,#19480,#19481,#19482,#19483,#19484,#19485,#19486,#19487,
#19488,#19489,#19490,#19491,#19492,#19493,#19494,#19495,#19496,#19497,#19498,
#19499,#19500,#19501,#19502,#19503,#19504,#19505,#19506,#19507,#19508,#19509,
#19510,#19511,#19512,#19513,#19514,#19515,#19516,#19517,#19518,#19519,#19520,
#19521,#19522,#19523,#19524,#19525,#19526,#19527,#19528,#19529,#19530,#19531,
#19532,#19533,#19534),.UNSPECIFIED.,.F.,.F.,(4,2,2,2,2,2,2,2,2,2,2,2,2,
2,2,2,2,2,2,2,2,2,2,2,2,2,2,2,2,2,2,2,2,2,2,2,2,2,2,2,2,2,2,2,2,2,2,2,2,
2,2,2,2,2,2,2,2,2,2,2,2,2,2,2,2,2,2,2,2,2,2,2,2,2,2,2,2,2,2,2,2,2,2,2,2,
2,2,2,2,2,2,4),(-1.96151746922958,-1.93727845031055,-1.92898480844812,-1.92659162702624,
-1.92498491993979,-1.92343202148895,-1.92204358143207,-1.92028481312109,
-1.9168396885906,-1.88785898840766,-1.87113312630283,-1.85057292507077,
-1.84724551398873,-1.84631416469784,-1.84542819473164,-1.84465087947126,
-1.84364493379295,-1.84152811838242,-1.81932918197427,-1.79790337945429,
-1.78131157110743,-1.7719381670023,-1.76945230339913,-1.76788739961022,
-1.76650086025616,-1.76476139471517,-1.76204965271811,-1.74840992452315,
-1.7105047322141,-1.69842384303046,-1.69228729026909,-1.69077507009605,
-1.68987164801956,-1.68909662644185,-1.68811633747501,-1.68613001591616,
-1.67277769161369,-1.62826703898947,-1.61659762481968,-1.61386368015248,
-1.61227920804905,-1.61089510891462,-1.60918442042709,-1.60656594615312,
-1.5943668329289,-1.58874312157041,-1.54446754366595,-1.53670437923497,
-1.53508500239637,-1.5341816307481,-1.53340655545089,-1.53242607407969,
-1.53043895517707,-1.51706483565853,-1.47251392379055,-1.46089657373112,
-1.45816628659279,-1.45658256525736,-1.45519830481026,-1.45348636239918,
-1.45086399889714,-1.43861481869602,-1.43303537697942,-1.38872491425792,
-1.38100135470469,-1.37938435144635,-1.37848146701998,-1.37770629255487,
-1.37672502146537,-1.37473412349328,-1.3612453916283,-1.31647811126868,
-1.30515290239546,-1.30244399942862,-1.30086493780993,-1.29948009596275,
-1.2977613937601,-1.29511732468393,-1.28254011330064,-1.27724753366755,
-1.23269855765341,-1.22525982519969,-1.22366073654916,-1.22276173770474,
-1.22198607821221,-1.22099925600954,-1.21942760138736,-1.21113209034205,
-1.2067489935596,-1.20136265316979,-1.17191730528522,-1.16031565334655),
 .UNSPECIFIED.);
#224=B_SPLINE_CURVE_WITH_KNOTS('',3,(#19540,#19541,#19542,#19543,#19544,
#19545,#19546,#19547,#19548,#19549,#19550,#19551,#19552,#19553,#19554,#19555,
#19556,#19557,#19558,#19559,#19560,#19561,#19562,#19563,#19564,#19565,#19566,
#19567,#19568,#19569,#19570,#19571,#19572,#19573,#19574,#19575,#19576,#19577,
#19578,#19579,#19580,#19581,#19582,#19583,#19584,#19585,#19586,#19587,#19588,
#19589,#19590,#19591,#19592,#19593,#19594,#19595,#19596,#19597,#19598,#19599,
#19600,#19601,#19602,#19603,#19604,#19605,#19606,#19607,#19608,#19609,#19610,
#19611,#19612,#19613,#19614,#19615,#19616,#19617,#19618,#19619,#19620,#19621,
#19622,#19623,#19624,#19625,#19626,#19627,#19628,#19629,#19630,#19631,#19632,
#19633,#19634,#19635,#19636,#19637,#19638,#19639,#19640,#19641,#19642,#19643,
#19644,#19645,#19646,#19647,#19648,#19649,#19650,#19651,#19652,#19653,#19654,
#19655,#19656,#19657,#19658,#19659,#19660,#19661,#19662,#19663,#19664,#19665,
#19666,#19667,#19668,#19669,#19670,#19671,#19672,#19673,#19674,#19675,#19676,
#19677,#19678,#19679,#19680,#19681,#19682,#19683,#19684,#19685,#19686,#19687,
#19688,#19689,#19690,#19691,#19692,#19693,#19694,#19695,#19696,#19697,#19698,
#19699,#19700,#19701,#19702,#19703,#19704,#19705,#19706,#19707,#19708,#19709,
#19710,#19711,#19712,#19713,#19714,#19715,#19716,#19717,#19718,#19719,#19720,
#19721,#19722,#19723,#19724,#19725,#19726,#19727,#19728,#19729,#19730,#19731,
#19732,#19733,#19734,#19735,#19736,#19737),.UNSPECIFIED.,.F.,.F.,(4,2,2,
2,2,2,2,2,2,2,2,2,2,2,2,2,2,2,2,2,2,2,2,2,2,2,2,2,2,2,2,2,2,2,2,2,2,2,2,
2,2,2,2,2,2,2,2,2,2,2,2,2,2,2,2,2,2,2,2,2,2,2,2,2,2,2,2,2,2,2,2,2,2,2,2,
2,2,2,2,2,2,2,2,2,2,2,2,2,2,2,2,2,2,2,2,2,2,2,4),(-0.801569876662303,-0.801463858289568,
-0.800482425275218,-0.799707068486446,-0.798803891038373,-0.797186160095882,
-0.789454757931817,-0.745160175146095,-0.739502265562737,-0.727349256919827,
-0.724733330520345,-0.723023101294776,-0.721638578695533,-0.720052745901819,
-0.717314230398579,-0.705590694732003,-0.661074136886435,-0.647753922838687,
-0.645768034199026,-0.644787600629747,-0.644012288598972,-0.643108307384019,
-0.641487003347999,-0.633698223197594,-0.589447778114414,-0.583724261980592,
-0.571643756383663,-0.569032671005808,-0.567323901723564,-0.565939426837225,
-0.564352401042487,-0.561608661341011,-0.549813191712586,-0.505345166819569,
-0.492053390125155,-0.490068371466816,-0.489088086999237,-0.488312755477423,
-0.487408593589715,-0.485786571273855,-0.477986849676421,-0.433743001442838,
-0.428006870141869,-0.415939625547551,-0.413329364783807,-0.411620811727912,
-0.410236296770244,-0.408648988088626,-0.405904157778154,-0.394094529716444,
-0.349634163397666,-0.336347385742434,-0.334362465036885,-0.333382174855872,
-0.332606812307873,-0.33172075121546,-0.330158873001522,-0.328220012042088,
-0.324132738076345,-0.31225309554124,-0.270088997756828,-0.26714277861644,
-0.260278105308956,-0.25764832486264,-0.255933680916197,-0.25454865805872,
-0.252965617884811,-0.250240411818147,-0.239304301113367,-0.194252412631134,
-0.180656367313936,-0.178661400890362,-0.177679064473676,-0.176903506177318,
-0.176018823753888,-0.17447154027809,-0.17254943680273,-0.16851145891962,
-0.156847167086858,-0.137828617482657,-0.105499170228988,-0.102082215881069,
-0.100328809719274,-0.0989401639124942,-0.0973823753025414,-0.094771990863102,
-0.0846944940112641,-0.0462381770388969,-0.0391970233454014,-0.036003345961913,
-0.0248449281017594,-0.023131075511108,-0.022112466437153,-0.0213310021061866,
-0.0206041548507821,-0.0197442688011261,-0.0184954649651884,-0.013736546252949,
-0.000459443335965334),.UNSPECIFIED.);
#225=B_SPLINE_CURVE_WITH_KNOTS('',3,(#19738,#19739,#19740,#19741,#19742,
#19743,#19744,#19745,#19746,#19747,#19748,#19749,#19750,#19751,#19752,#19753,
#19754,#19755,#19756,#19757,#19758,#19759,#19760,#19761,#19762,#19763,#19764,
#19765,#19766,#19767,#19768,#19769,#19770,#19771,#19772,#19773,#19774,#19775,
#19776,#19777),.UNSPECIFIED.,.F.,.F.,(4,2,2,2,2,2,2,2,2,2,2,2,2,2,2,2,2,
2,2,4),(-1.9616930950669,-1.91882405866371,-1.91264227358543,-1.90812554288186,
-1.90618919366793,-1.90477417343448,-1.9034723736324,-1.90137279507223,
-1.89623193052963,-1.85877429407012,-1.84271434581574,-1.8343410922473,
-1.82952531234533,-1.82814087505396,-1.82740855395721,-1.82663312178802,
-1.82565027240673,-1.82409189630884,-1.81601648426919,-1.78228100909597),
 .UNSPECIFIED.);
#226=B_SPLINE_CURVE_WITH_KNOTS('',3,(#19778,#19779,#19780,#19781,#19782,
#19783,#19784,#19785,#19786,#19787,#19788,#19789,#19790,#19791,#19792,#19793,
#19794,#19795,#19796,#19797,#19798,#19799,#19800,#19801,#19802,#19803,#19804,
#19805,#19806,#19807,#19808,#19809,#19810,#19811,#19812,#19813,#19814,#19815,
#19816,#19817,#19818,#19819,#19820,#19821,#19822,#19823,#19824,#19825,#19826,
#19827,#19828,#19829,#19830,#19831,#19832,#19833,#19834,#19835,#19836,#19837,
#19838,#19839,#19840,#19841,#19842,#19843,#19844,#19845,#19846,#19847,#19848,
#19849,#19850,#19851,#19852,#19853,#19854,#19855,#19856,#19857,#19858,#19859,
#19860,#19861,#19862,#19863,#19864,#19865,#19866,#19867,#19868,#19869,#19870,
#19871,#19872,#19873,#19874,#19875,#19876,#19877,#19878,#19879,#19880,#19881,
#19882,#19883,#19884,#19885,#19886,#19887,#19888,#19889,#19890,#19891,#19892,
#19893,#19894,#19895,#19896,#19897,#19898,#19899,#19900,#19901,#19902,#19903,
#19904,#19905,#19906,#19907,#19908,#19909,#19910,#19911,#19912,#19913,#19914,
#19915,#19916,#19917,#19918,#19919,#19920,#19921,#19922,#19923,#19924,#19925,
#19926,#19927,#19928,#19929,#19930,#19931,#19932,#19933,#19934,#19935,#19936,
#19937,#19938,#19939,#19940,#19941,#19942,#19943,#19944,#19945,#19946,#19947,
#19948,#19949,#19950,#19951,#19952,#19953,#19954,#19955,#19956,#19957,#19958,
#19959,#19960,#19961,#19962,#19963,#19964,#19965,#19966,#19967,#19968,#19969,
#19970,#19971,#19972,#19973,#19974,#19975,#19976,#19977,#19978,#19979,#19980,
#19981,#19982,#19983,#19984,#19985,#19986,#19987,#19988,#19989,#19990,#19991,
#19992,#19993,#19994,#19995,#19996,#19997,#19998,#19999,#20000,#20001,#20002,
#20003,#20004,#20005,#20006,#20007,#20008,#20009,#20010,#20011,#20012,#20013,
#20014,#20015,#20016,#20017,#20018,#20019,#20020,#20021,#20022,#20023,#20024,
#20025),.UNSPECIFIED.,.F.,.F.,(4,2,2,2,2,2,2,2,2,2,2,2,2,2,2,2,2,2,2,2,
2,2,2,2,2,2,2,2,2,2,2,2,2,2,2,2,2,2,2,2,2,2,2,2,2,2,2,2,2,2,2,2,2,2,2,2,
2,2,2,2,2,2,2,2,2,2,2,2,2,2,2,2,2,2,2,2,2,2,2,2,2,2,2,2,2,2,2,2,2,2,2,2,
2,2,2,2,2,2,2,2,2,2,2,2,2,2,2,2,2,2,2,2,2,2,2,2,2,2,2,2,2,2,2,4),(-1.16031565334655,
-1.1523673019911,-1.14785507366041,-1.14591960065616,-1.14450483217052,
-1.14320299451157,-1.14110276182394,-1.13595736912939,-1.13460617764447,
-1.12997769923691,-1.12915159021155,-1.1288777943079,-1.08582161433698,
-1.07510385683424,-1.06936172998066,-1.06788882347475,-1.06701764560893,
-1.06623680838649,-1.06522136664119,-1.06351787069468,-1.05260983184458,
-1.04675761591003,-1.01355437678732,-0.996263279450873,-0.992039456976342,
-0.990154732372975,-0.988748474761843,-0.987433959098141,-0.985621800596761,
-0.980984198074936,-0.959588741131954,-0.92576208051337,-0.914449902568713,
-0.912564864604286,-0.911592393020659,-0.910817679489454,-0.909907804202454,
-0.908259241851401,-0.90000757724465,-0.856125099040339,-0.849884600885847,
-0.838365541213197,-0.835544122640188,-0.833923202066467,-0.832679172460978,
-0.831069068772479,-0.828219726257148,-0.814819825257841,-0.785260983898237,
-0.775814978572803,-0.759029000198427,-0.756952758562451,-0.755954511199894,
-0.75517776137945,-0.754286382142591,-0.752722173486889,-0.7458027557844,
-0.702743196561065,-0.693781739159207,-0.682632497009242,-0.679842214769354,
-0.678228514269354,-0.676859329700738,-0.67519055587507,-0.672068055233415,
-0.652894887063777,-0.617891491203387,-0.615207746475259,-0.61253423219707,
-0.602937515005818,-0.601295399164744,-0.600298043200082,-0.599519607036988,
-0.598638133757354,-0.597118680723868,-0.590805287070827,-0.578462765474866,
-0.547112847724725,-0.538152799437653,-0.526991399645208,-0.524200014558887,
-0.522586024766068,-0.52121680016192,-0.519548229843057,-0.516426866112247,
-0.497287482406008,-0.462657118186587,-0.459167059164731,-0.447458225940103,
-0.445557429421433,-0.444581607127788,-0.443806732168894,-0.442899567288428,
-0.441263270823624,-0.433221786600635,-0.389181586661826,-0.383221713536389,
-0.371398118994128,-0.368552069041258,-0.366925589097279,-0.36568180558335,
-0.364077353349327,-0.361253511728051,-0.348261525455421,-0.320349458563087,
-0.294096609446201,-0.290598350985114,-0.289325978397033,-0.288581721547749,
-0.287839004420659,-0.286880814434218,-0.284802913401485,-0.282006636755118,
-0.251607225783504,-0.219524941223758,-0.214244036214387,-0.21212093211589,
-0.210814870378466,-0.209403295591622,-0.207486098587411,-0.203078922671946,
-0.197086732289873,-0.181309345770682,-0.179896456144152),.UNSPECIFIED.);
#227=B_SPLINE_CURVE_WITH_KNOTS('',3,(#20030,#20031,#20032,#20033,#20034,
#20035,#20036,#20037,#20038,#20039,#20040,#20041,#20042,#20043,#20044,#20045,
#20046,#20047,#20048,#20049,#20050,#20051,#20052,#20053,#20054,#20055,#20056,
#20057,#20058,#20059,#20060,#20061,#20062,#20063,#20064,#20065,#20066,#20067,
#20068,#20069,#20070,#20071,#20072,#20073,#20074,#20075,#20076,#20077,#20078,
#20079,#20080,#20081,#20082,#20083,#20084,#20085,#20086,#20087,#20088,#20089,
#20090,#20091,#20092,#20093,#20094,#20095,#20096,#20097,#20098,#20099,#20100,
#20101,#20102,#20103,#20104,#20105,#20106,#20107,#20108,#20109,#20110,#20111,
#20112,#20113,#20114,#20115,#20116,#20117,#20118,#20119,#20120,#20121,#20122,
#20123,#20124,#20125,#20126,#20127,#20128,#20129,#20130,#20131,#20132,#20133,
#20134,#20135,#20136,#20137,#20138,#20139,#20140,#20141,#20142,#20143,#20144,
#20145,#20146,#20147,#20148,#20149,#20150,#20151,#20152,#20153,#20154,#20155,
#20156,#20157,#20158,#20159,#20160,#20161,#20162,#20163,#20164,#20165,#20166,
#20167,#20168,#20169,#20170,#20171,#20172,#20173,#20174,#20175,#20176,#20177,
#20178,#20179,#20180,#20181,#20182,#20183,#20184,#20185,#20186,#20187,#20188,
#20189,#20190,#20191,#20192,#20193,#20194,#20195,#20196,#20197,#20198,#20199,
#20200,#20201,#20202,#20203,#20204,#20205,#20206,#20207,#20208,#20209,#20210,
#20211,#20212,#20213,#20214,#20215,#20216,#20217,#20218,#20219,#20220,#20221,
#20222,#20223,#20224,#20225,#20226,#20227,#20228,#20229,#20230,#20231,#20232,
#20233,#20234,#20235,#20236,#20237,#20238,#20239,#20240,#20241,#20242,#20243,
#20244,#20245,#20246,#20247,#20248,#20249,#20250,#20251,#20252,#20253,#20254,
#20255,#20256,#20257,#20258,#20259,#20260,#20261,#20262,#20263,#20264,#20265,
#20266,#20267,#20268,#20269,#20270,#20271,#20272,#20273,#20274,#20275,#20276,
#20277,#20278,#20279,#20280,#20281,#20282,#20283,#20284,#20285,#20286,#20287,
#20288,#20289,#20290,#20291,#20292,#20293,#20294,#20295,#20296,#20297),
 .UNSPECIFIED.,.F.,.F.,(4,2,2,2,2,2,2,2,2,2,2,2,2,2,2,2,2,2,2,2,2,2,2,2,
2,2,2,2,2,2,2,2,2,2,2,2,2,2,2,2,2,2,2,2,2,2,2,2,2,2,2,2,2,2,2,2,2,2,2,2,
2,2,2,2,2,2,2,2,2,2,2,2,2,2,2,2,2,2,2,2,2,2,2,2,2,2,2,2,2,2,2,2,2,2,2,2,
2,2,2,2,2,2,2,2,2,2,2,2,2,2,2,2,2,2,2,2,2,2,2,2,2,2,2,2,2,2,2,2,2,2,2,2,
2,4),(-1.78157392576435,-1.77703986719531,-1.75183319619201,-1.73827487711637,
-1.73547815848269,-1.73435161834043,-1.73355540911073,-1.73282270068874,
-1.73160957411766,-1.72849339879885,-1.69230500609923,-1.66219518654377,
-1.65966339436276,-1.65799877502422,-1.65642827813615,-1.65642456312669,
-1.65642083260329,-1.65641708641202,-1.65641332439903,-1.6564095464009,
-1.65640575226783,-1.65640194184385,-1.65639811496712,-1.65639427145904,
-1.65639041116129,-1.65638653391513,-1.65638263954875,-1.65637872789209,
-1.65637479876522,-1.65637085199926,-1.65636688740295,-1.65636290480605,
-1.65635890402627,-1.65635488486844,-1.65635084714899,-1.65634679068422,
-1.65634271542142,-1.6549889433836,-1.65327486426759,-1.6500997041622,-1.63238876722318,
-1.59967144067176,-1.58709227218365,-1.58070072137787,-1.57917549504868,
-1.57829288112802,-1.5775148975866,-1.57651998720862,-1.57440499194861,
-1.55123771017638,-1.54690886626453,-1.51845272167325,-1.50532498054874,
-1.50249305163127,-1.50088702121455,-1.49964342687909,-1.49801921388676,
-1.4951822520972,-1.48346647742908,-1.47741146468242,-1.43336194169185,
-1.42530617929179,-1.42366918431813,-1.42276194033454,-1.42198717902635,
-1.42101172114954,-1.41911227748877,-1.40743063973138,-1.37024355756011,
-1.35695941054654,-1.34891487615597,-1.34649933647858,-1.34498516636977,
-1.3435867816907,-1.34178255619808,-1.33879229544754,-1.31926699010906,
-1.28785312968101,-1.27573233182799,-1.26949544208271,-1.26798205969689,
-1.26710198542805,-1.26632335330376,-1.26532389880708,-1.26367452719552,
-1.2539283386789,-1.2515770057581,-1.21423149008515,-1.20122448856538,-1.19330057924157,
-1.19089805402565,-1.18938675998721,-1.1879874178821,-1.18617687638681,
-1.18316509291153,-1.16276749776549,-1.12056606932057,-1.11392545846318,
-1.11238128001053,-1.11149433284049,-1.11071688691739,-1.10971171822844,
-1.10759988313139,-1.08728518949668,-1.05781589971924,-1.04532672323364,
-1.03763111015008,-1.03525351936236,-1.03374758284089,-1.03234606024005,
-1.03052255846313,-1.02746691316668,-1.00530609355621,-0.980688863891826,
-0.959290533031398,-0.957173317188728,-0.956177821375156,-0.955399592326297,
-0.954516932260381,-0.952992170219633,-0.946610153339468,-0.934063253638346,
-0.901712058815225,-0.895695800147351,-0.883098238582525,-0.880452551544035,
-0.878733159612078,-0.877348005872783,-0.875768851224845,-0.873060438659509,
-0.861746850641419,-0.816934939181304,-0.803454861381081,-0.801569876662303),
 .UNSPECIFIED.);
#228=B_SPLINE_CURVE_WITH_KNOTS('',3,(#20299,#20300,#20301,#20302,#20303,
#20304,#20305,#20306,#20307,#20308,#20309,#20310,#20311,#20312,#20313,#20314,
#20315,#20316,#20317,#20318,#20319,#20320,#20321,#20322,#20323,#20324,#20325,
#20326,#20327,#20328,#20329,#20330,#20331,#20332,#20333,#20334,#20335,#20336,
#20337,#20338),.UNSPECIFIED.,.F.,.F.,(4,2,2,2,2,2,2,2,2,2,2,2,2,2,2,2,2,
2,2,4),(-0.179896456144152,-0.145985047401615,-0.135982032119122,-0.13431993856968,
-0.133316680841151,-0.132537509157973,-0.131809685279224,-0.130494634624559,
-0.126340778320527,-0.119504086046154,-0.101385875338663,-0.0636422736938331,
-0.0585183563700689,-0.056421716430441,-0.05512054055286,-0.0537052463391859,
-0.0517668127261477,-0.0472374260604156,-0.0410328162612283,-0.000460268800049601),
 .UNSPECIFIED.);
#229=B_SPLINE_CURVE_WITH_KNOTS('',3,(#20339,#20340,#20341,#20342,#20343,
#20344,#20345,#20346,#20347),.UNSPECIFIED.,.F.,.F.,(4,1,1,1,1,1,4),(179.070781254618,
179.221343132621,180.218997427939,181.216651723258,182.214306018576,183.211960313895,
184.204982640327),.UNSPECIFIED.);
#230=B_SPLINE_CURVE_WITH_KNOTS('',3,(#20353,#20354,#20355,#20356,#20357,
#20358,#20359,#20360,#20361,#20362,#20363,#20364,#20365,#20366,#20367,#20368,
#20369,#20370,#20371,#20372,#20373,#20374,#20375,#20376,#20377,#20378,#20379,
#20380,#20381,#20382,#20383,#20384,#20385,#20386,#20387,#20388,#20389,#20390,
#20391,#20392,#20393,#20394,#20395,#20396,#20397,#20398,#20399,#20400,#20401,
#20402,#20403,#20404,#20405,#20406,#20407,#20408,#20409,#20410,#20411,#20412,
#20413,#20414,#20415,#20416,#20417,#20418,#20419,#20420,#20421,#20422,#20423,
#20424,#20425,#20426,#20427,#20428,#20429,#20430,#20431,#20432,#20433,#20434,
#20435,#20436,#20437,#20438,#20439,#20440,#20441,#20442,#20443,#20444,#20445,
#20446,#20447,#20448,#20449,#20450,#20451,#20452,#20453,#20454,#20455,#20456,
#20457,#20458,#20459,#20460,#20461,#20462,#20463,#20464,#20465,#20466,#20467,
#20468,#20469,#20470,#20471,#20472,#20473,#20474,#20475,#20476,#20477,#20478,
#20479,#20480,#20481,#20482,#20483,#20484,#20485,#20486,#20487,#20488,#20489,
#20490,#20491,#20492,#20493,#20494,#20495,#20496,#20497,#20498,#20499,#20500,
#20501,#20502,#20503,#20504,#20505,#20506,#20507,#20508,#20509,#20510,#20511,
#20512,#20513,#20514,#20515,#20516,#20517,#20518,#20519,#20520,#20521,#20522,
#20523,#20524,#20525,#20526,#20527,#20528,#20529,#20530,#20531,#20532,#20533,
#20534,#20535,#20536,#20537,#20538,#20539,#20540,#20541,#20542,#20543,#20544,
#20545,#20546,#20547,#20548),.UNSPECIFIED.,.F.,.F.,(4,2,2,2,2,2,2,2,2,2,
2,2,2,2,2,2,2,2,2,2,2,2,2,2,2,2,2,2,2,2,2,2,2,2,2,2,2,2,2,2,2,2,2,2,2,2,
2,2,2,2,2,2,2,2,2,2,2,2,2,2,2,2,2,2,2,2,2,2,2,2,2,2,2,2,2,2,2,2,2,2,2,2,
2,2,2,2,2,2,2,2,2,2,2,2,2,2,2,4),(-0.801804981179806,-0.791195181952112,
-0.78820379362701,-0.78639864088365,-0.784999399902408,-0.783484166028639,
-0.781066634915162,-0.773012825789302,-0.759708368143552,-0.722486014975232,
-0.710788191922156,-0.708887092198146,-0.707910898492826,-0.707135613048346,
-0.706227820637099,-0.704590009597872,-0.696533258951253,-0.652475124541805,
-0.646421413217755,-0.63469777726604,-0.631858809355539,-0.630233423006621,
-0.628988920467047,-0.627381700427813,-0.624547636466169,-0.611409824376443,
-0.582929094133007,-0.57659321994821,-0.555382330138853,-0.553264718573913,
-0.552258140865215,-0.551480221862471,-0.550593415458993,-0.549051077822034,
-0.542442194165679,-0.500328073024698,-0.479809619561363,-0.476793655627731,
-0.474981375070188,-0.473581154106954,-0.472069373104979,-0.469667067488223,
-0.461752996108073,-0.448769074051514,-0.411484258891166,-0.408773200682247,
-0.39919795411811,-0.397556381805616,-0.396558940683188,-0.395780175377634,
-0.394898019913743,-0.393376673005521,-0.387045155925027,-0.374651345922992,
-0.343224652481315,-0.324051009245048,-0.321080607647489,-0.319281669821315,
-0.31792080664303,-0.316445009591454,-0.314913905802875,-0.312705023756506,
-0.3088518933673,-0.277970702210061,-0.245813850415554,-0.242456681833825,
-0.241205466117216,-0.240465088819104,-0.239673803790103,-0.238576055805226,
-0.235955587474011,-0.208002316387905,-0.171261442735374,-0.166086824696459,
-0.163978234720007,-0.162674368778266,-0.161288209928795,-0.159415023700057,
-0.157327606071686,-0.153775409699347,-0.127761519786595,-0.100451926709456,
-0.0880266345113613,-0.0860968103046999,-0.0851144928007718,-0.0843388085831969,
-0.0834356757270043,-0.0818190833842118,-0.0741129438788946,-0.0297790823181762,
-0.017138014229754,-0.0107741459344145,-0.00848312639086696,-0.0071444586676528,
-0.00580070256809082,-0.0044503611599955,-0.00251092333097463,-0.000459684857462615),
 .UNSPECIFIED.);
#231=B_SPLINE_CURVE_WITH_KNOTS('',3,(#20549,#20550,#20551,#20552,#20553,
#20554,#20555,#20556,#20557,#20558,#20559,#20560,#20561,#20562,#20563,#20564,
#20565,#20566,#20567,#20568,#20569,#20570,#20571,#20572,#20573,#20574,#20575,
#20576,#20577,#20578,#20579,#20580,#20581,#20582,#20583,#20584,#20585,#20586,
#20587,#20588,#20589,#20590,#20591,#20592,#20593,#20594,#20595,#20596,#20597,
#20598,#20599,#20600,#20601,#20602,#20603,#20604,#20605,#20606,#20607,#20608,
#20609,#20610,#20611,#20612,#20613,#20614,#20615,#20616,#20617,#20618,#20619,
#20620,#20621,#20622,#20623,#20624,#20625,#20626,#20627,#20628,#20629,#20630),
 .UNSPECIFIED.,.F.,.F.,(4,2,2,2,2,2,2,2,2,2,2,2,2,2,2,2,2,2,2,2,2,2,2,2,
2,2,2,2,2,2,2,2,2,2,2,2,2,2,2,2,4),(-1.96076531947618,-1.94084069828309,
-1.89859390740446,-1.89193598296996,-1.89039057645452,-1.88950337962962,
-1.8887260128179,-1.8877213401337,-1.88609061961138,-1.87671706757189,-1.87374154668446,
-1.83654431366111,-1.82357963776505,-1.81834047535616,-1.81559441560497,
-1.81384023680584,-1.81220579194079,-1.81219072987945,-1.81217546787841,
-1.81215999766016,-1.81214431057571,-1.81212839757627,-1.81211224918606,
-1.81209585547706,-1.81208474088437,-1.81207280521556,-1.81205997335984,
-1.81204616119084,-1.8120312741524,-1.81201520556063,-1.81199783454238,
-1.81197902354186,-1.81195861526728,-1.81193642849298,-1.81191225379885,
-1.8118858491898,-1.81185693010414,-1.81049833731243,-1.80873027082396,
-1.8053131326592,-1.78157392576435),.UNSPECIFIED.);
#232=B_SPLINE_CURVE_WITH_KNOTS('',3,(#20632,#20633,#20634,#20635,#20636,
#20637),.UNSPECIFIED.,.F.,.F.,(4,1,1,4),(184.204982640327,184.209614609213,
185.207268904532,185.353966561798),.UNSPECIFIED.);
#233=B_SPLINE_CURVE_WITH_KNOTS('',3,(#20638,#20639,#20640,#20641,#20642,
#20643,#20644,#20645,#20646,#20647,#20648,#20649,#20650,#20651,#20652,#20653,
#20654,#20655,#20656,#20657,#20658,#20659,#20660,#20661,#20662,#20663,#20664,
#20665,#20666,#20667,#20668,#20669,#20670,#20671,#20672,#20673,#20674,#20675,
#20676,#20677,#20678,#20679,#20680,#20681,#20682,#20683,#20684,#20685,#20686,
#20687,#20688,#20689,#20690,#20691,#20692,#20693,#20694,#20695,#20696,#20697,
#20698,#20699,#20700,#20701,#20702,#20703,#20704,#20705,#20706,#20707,#20708,
#20709,#20710,#20711,#20712,#20713,#20714,#20715,#20716,#20717,#20718,#20719,
#20720,#20721,#20722,#20723,#20724,#20725,#20726,#20727,#20728,#20729,#20730,
#20731,#20732,#20733,#20734,#20735,#20736,#20737,#20738,#20739,#20740,#20741,
#20742,#20743,#20744,#20745,#20746,#20747,#20748,#20749,#20750,#20751,#20752,
#20753,#20754,#20755,#20756,#20757,#20758,#20759,#20760,#20761,#20762,#20763,
#20764,#20765,#20766,#20767,#20768,#20769,#20770,#20771,#20772,#20773,#20774,
#20775,#20776,#20777,#20778,#20779,#20780,#20781,#20782,#20783,#20784,#20785,
#20786,#20787,#20788,#20789,#20790,#20791,#20792,#20793,#20794,#20795,#20796,
#20797,#20798,#20799,#20800,#20801,#20802,#20803,#20804,#20805,#20806,#20807,
#20808,#20809,#20810,#20811,#20812,#20813,#20814,#20815,#20816,#20817,#20818,
#20819,#20820,#20821,#20822,#20823),.UNSPECIFIED.,.F.,.F.,(4,2,2,2,2,2,
2,2,2,2,2,2,2,2,2,2,2,2,2,2,2,2,2,2,2,2,2,2,2,2,2,2,2,2,2,2,2,2,2,2,2,2,
2,2,2,2,2,2,2,2,2,2,2,2,2,2,2,2,2,2,2,2,2,2,2,2,2,2,2,2,2,2,2,2,2,2,2,2,
2,2,2,2,2,2,2,2,2,2,2,2,2,2,4),(-1.96154615893119,-1.9204301144835,-1.91421112519999,
-1.90967349501717,-1.90773406611444,-1.90631898335972,-1.90501865184091,
-1.90292481837855,-1.89781502448428,-1.85984841609893,-1.84188976150091,
-1.83507397559582,-1.83092965281337,-1.82961639162936,-1.8288888845317,
-1.82810988983151,-1.82710620718605,-1.82544205879453,-1.81538722150474,
-1.77627551365403,-1.76309687074975,-1.75509850389648,-1.75268831831728,
-1.7511755908826,-1.74977723604173,-1.74797122575642,-1.74497406136101,
-1.72515117763501,-1.69090606373307,-1.68099351808462,-1.67737544669124,
-1.67559918847939,-1.67416313343874,-1.67334463311578,-1.67256962720246,
-1.67158833532593,-1.66959662616788,-1.65607040342538,-1.61123318159724,
-1.60001893629797,-1.59731881511132,-1.59574192996661,-1.59435722115097,
-1.59263637003297,-1.58998462886248,-1.57728267596355,-1.571417884776,-1.52729146054624,
-1.52013006658682,-1.51854954888397,-1.51765475940199,-1.51687878551326,
-1.51588642844732,-1.51383919085038,-1.48594169652985,-1.4576946664555,
-1.44461852412824,-1.44178988638511,-1.44018462139884,-1.43894110435512,
-1.43731625918759,-1.43447633623332,-1.4227233563749,-1.41669657975516,
-1.37268069735914,-1.36458805425462,-1.36294894452887,-1.36204126695385,
-1.36126658844729,-1.36029182671763,-1.35839549260358,-1.34679253028865,
-1.34225651823929,-1.30852822021364,-1.29120857661103,-1.28698143329094,
-1.28509636693623,-1.2836903049292,-1.28237629743356,-1.28056535202266,
-1.27593362407305,-1.23290256833061,-1.22479443634851,-1.21428031910573,
-1.20861311665486,-1.20714683633494,-1.20627721677358,-1.20549612938089,
-1.20447819929962,-1.20276590325398,-1.19163256212389,-1.18843259486761,
-1.1604089144409),.UNSPECIFIED.);
#234=B_SPLINE_CURVE_WITH_KNOTS('',3,(#20828,#20829,#20830,#20831,#20832,
#20833,#20834,#20835,#20836,#20837,#20838,#20839,#20840,#20841,#20842,#20843,
#20844,#20845,#20846,#20847,#20848,#20849,#20850,#20851,#20852,#20853,#20854,
#20855,#20856,#20857,#20858,#20859,#20860,#20861,#20862,#20863,#20864,#20865,
#20866,#20867,#20868,#20869,#20870,#20871,#20872,#20873,#20874,#20875,#20876,
#20877,#20878,#20879,#20880,#20881,#20882,#20883,#20884,#20885,#20886,#20887,
#20888,#20889,#20890,#20891,#20892,#20893,#20894,#20895,#20896,#20897,#20898,
#20899,#20900,#20901,#20902,#20903,#20904,#20905,#20906,#20907,#20908,#20909,
#20910,#20911,#20912,#20913,#20914,#20915,#20916,#20917,#20918,#20919,#20920,
#20921,#20922,#20923,#20924,#20925,#20926,#20927,#20928,#20929,#20930,#20931,
#20932,#20933,#20934,#20935,#20936,#20937,#20938,#20939,#20940,#20941,#20942,
#20943,#20944,#20945,#20946,#20947,#20948,#20949,#20950,#20951,#20952,#20953,
#20954,#20955,#20956,#20957,#20958,#20959,#20960,#20961,#20962,#20963,#20964,
#20965,#20966,#20967,#20968,#20969,#20970,#20971,#20972,#20973,#20974,#20975,
#20976,#20977,#20978,#20979,#20980,#20981,#20982,#20983,#20984,#20985,#20986,
#20987,#20988,#20989,#20990,#20991,#20992,#20993,#20994,#20995,#20996,#20997,
#20998,#20999,#21000,#21001,#21002,#21003,#21004,#21005,#21006,#21007,#21008,
#21009,#21010,#21011,#21012,#21013,#21014,#21015,#21016,#21017,#21018,#21019,
#21020,#21021,#21022,#21023,#21024,#21025,#21026,#21027,#21028,#21029,#21030,
#21031,#21032,#21033,#21034,#21035,#21036,#21037,#21038,#21039,#21040,#21041,
#21042,#21043,#21044,#21045,#21046,#21047,#21048,#21049),.UNSPECIFIED.,
 .F.,.F.,(4,2,2,2,2,2,2,2,2,2,2,2,2,2,2,2,2,2,2,2,2,2,2,2,2,2,2,2,2,2,2,
2,2,2,2,2,2,2,2,2,2,2,2,2,2,2,2,2,2,2,2,2,2,2,2,2,2,2,2,2,2,2,2,2,2,2,2,
2,2,2,2,2,2,2,2,2,2,2,2,2,2,2,2,2,2,2,2,2,2,2,2,2,2,2,2,2,2,2,2,2,2,2,2,
2,2,2,2,2,2,2,4),(-1.78229182699827,-1.77770006527103,-1.74728035674964,
-1.72722535303527,-1.72265056195955,-1.72070401254425,-1.71928696319564,
-1.71798706378127,-1.71589885047568,-1.71082762541292,-1.67223444044944,
-1.64752983476097,-1.64498095721691,-1.64359685769358,-1.64268136183101,
-1.64182077443158,-1.64106521535437,-1.64006101330455,-1.63843247151083,
-1.62910925449238,-1.6243756754617,-1.5789882557114,-1.56843404951485,-1.56578431027004,
-1.56421790544764,-1.56283077099427,-1.56109153229788,-1.55838201035786,
-1.54479651559656,-1.51216480444941,-1.49015262721293,-1.48761968100296,
-1.48653711254194,-1.48574861367651,-1.48500431351154,-1.48373240483364,
-1.48023838775766,-1.45413407404517,-1.42613534393613,-1.41312006270762,
-1.4102942149044,-1.40868902900732,-1.40744486278802,-1.40581815150025,
-1.40297236355887,-1.3911587623582,-1.38518496978347,-1.34106294051767,
-1.33306838337939,-1.33143442686769,-1.33052757310081,-1.32975235514613,
-1.32877531391351,-1.32686980440679,-1.31505008398384,-1.27760856441345,
-1.26456380318881,-1.25662228690092,-1.25421709163038,-1.25270472569067,
-1.2513048071232,-1.24949410535442,-1.24648333099836,-1.22617519094581,
-1.18387963955269,-1.17720850620729,-1.17566157010041,-1.17477374504427,
-1.1739959910329,-1.17299103360034,-1.17136027695541,-1.16199793714452,
-1.14540186853179,-1.12375086261623,-1.10437341472612,-1.09988152441872,
-1.09794891733958,-1.0965340458668,-1.09523057379023,-1.09312427935216,
-1.08794685017318,-1.05113546407829,-1.0232122483063,-1.02059167294599,
-1.0194938696369,-1.01870254272551,-1.01796212380633,-1.01671083342138,
-1.01335343759903,-0.981228689407384,-0.947011206645786,-0.943932276143987,
-0.942101488150138,-0.940698213617958,-0.939194157648731,-0.936827476357734,
-0.929236059216975,-0.916980174939113,-0.892734951719288,-0.878430304643932,
-0.876064713121345,-0.866322573478264,-0.864672646487258,-0.863672714249389,
-0.86289361929424,-0.862012911520759,-0.860498201068073,-0.854252320692013,
-0.84211098432762,-0.810714702698044,-0.801804981179806),.UNSPECIFIED.);
#235=B_SPLINE_CURVE_WITH_KNOTS('',3,(#21050,#21051,#21052,#21053,#21054,
#21055,#21056,#21057,#21058,#21059,#21060,#21061,#21062,#21063,#21064,#21065,
#21066,#21067,#21068,#21069,#21070,#21071,#21072,#21073,#21074,#21075,#21076,
#21077,#21078,#21079,#21080,#21081,#21082,#21083,#21084,#21085,#21086,#21087,
#21088,#21089,#21090,#21091,#21092,#21093,#21094,#21095,#21096,#21097,#21098,
#21099,#21100,#21101,#21102,#21103,#21104,#21105,#21106,#21107,#21108,#21109,
#21110,#21111,#21112,#21113,#21114,#21115,#21116,#21117,#21118,#21119,#21120,
#21121,#21122,#21123,#21124,#21125,#21126,#21127,#21128,#21129,#21130,#21131,
#21132,#21133,#21134,#21135,#21136,#21137,#21138,#21139,#21140,#21141,#21142,
#21143,#21144,#21145,#21146,#21147,#21148,#21149,#21150,#21151,#21152,#21153,
#21154,#21155,#21156,#21157,#21158,#21159,#21160,#21161,#21162,#21163,#21164,
#21165,#21166,#21167,#21168,#21169,#21170,#21171,#21172,#21173,#21174,#21175,
#21176,#21177,#21178,#21179,#21180,#21181,#21182,#21183,#21184,#21185,#21186,
#21187,#21188,#21189,#21190,#21191,#21192,#21193,#21194,#21195,#21196,#21197,
#21198,#21199,#21200,#21201,#21202,#21203,#21204,#21205,#21206,#21207,#21208,
#21209,#21210,#21211,#21212,#21213,#21214,#21215,#21216,#21217,#21218,#21219,
#21220,#21221,#21222,#21223,#21224,#21225,#21226,#21227,#21228,#21229,#21230,
#21231,#21232,#21233,#21234,#21235,#21236,#21237,#21238,#21239,#21240,#21241,
#21242,#21243,#21244,#21245,#21246,#21247,#21248,#21249,#21250,#21251,#21252,
#21253,#21254,#21255,#21256,#21257,#21258,#21259,#21260,#21261,#21262,#21263,
#21264,#21265,#21266,#21267,#21268,#21269,#21270,#21271,#21272,#21273,#21274,
#21275,#21276,#21277,#21278,#21279,#21280,#21281),.UNSPECIFIED.,.F.,.F.,
(4,2,2,2,2,2,2,2,2,2,2,2,2,2,2,2,2,2,2,2,2,2,2,2,2,2,2,2,2,2,2,2,2,2,2,
2,2,2,2,2,2,2,2,2,2,2,2,2,2,2,2,2,2,2,2,2,2,2,2,2,2,2,2,2,2,2,2,2,2,2,2,
2,2,2,2,2,2,2,2,2,2,2,2,2,2,2,2,2,2,2,2,2,2,2,2,2,2,2,2,2,2,2,2,2,2,2,2,
2,2,2,2,2,2,2,2,4),(-1.1604089144409,-1.15301712491792,-1.1338042420669,
-1.13068051289322,-1.12901153209055,-1.12764240662223,-1.12602904408292,
-1.12324001000303,-1.11210442569331,-1.10313057710444,-1.07175088106854,
-1.05939417886841,-1.05307681964018,-1.05155711810077,-1.05067562963774,
-1.04989726168839,-1.04890010709256,-1.04725856324169,-1.03767102385391,
-1.00635729547857,-0.981218835397845,-0.976166204963473,-0.974081488014664,
-0.972782535873951,-0.971365535445268,-0.969417273943396,-0.964830224656248,
-0.944666579985529,-0.913243095579635,-0.909871213480826,-0.905759400379418,
-0.897797095538855,-0.896245785835583,-0.895265171617205,-0.894490021105889,
-0.893586591162298,-0.89196719186132,-0.884205084181735,-0.839948068302154,
-0.834325866530686,-0.822129237122471,-0.819510681777071,-0.817799820056214,
-0.816415509602126,-0.81483071742641,-0.812096024767854,-0.800420722036785,
-0.755880920441822,-0.742520864445167,-0.740533919546976,-0.739553391857166,
-0.73877821697435,-0.737874652047628,-0.736254745129661,-0.728485182119267,
-0.684231961683498,-0.678601482084515,-0.666413324999779,-0.663795262389957,
-0.66208451356173,-0.660700155690935,-0.659115156918223,-0.656379722577751,
-0.644695280675613,-0.600159672584616,-0.586802488947652,-0.584815569613071,
-0.583835021420027,-0.583059814118981,-0.582156192782227,-0.580536138305966,
-0.572764989251016,-0.528510824957319,-0.522878689857053,-0.510691575115682,
-0.508073503859469,-0.506362712727791,-0.504978296292453,-0.503393203756708,
-0.500657540041379,-0.488971070219121,-0.444434581289266,-0.431077417471671,
-0.429090430541218,-0.42810984317089,-0.427334602049022,-0.426430938017126,
-0.424810798837877,-0.417039089136524,-0.372783153470298,-0.367150523091922,
-0.354963149405569,-0.352344981651356,-0.350634121020652,-0.349249644068411,
-0.347664477549055,-0.344928674273935,-0.333241424026262,-0.288703164602155,
-0.275345519732835,-0.273358448839536,-0.27237781901006,-0.271602543819682,
-0.270698839500287,-0.269186179378965,-0.263391821277015,-0.252166053312491,
-0.213302891610325,-0.199460213040507,-0.1967331721054,-0.19498869811307,
-0.193601263172659,-0.192038634393199,-0.189552228995395,-0.180241678035301,
-0.179869993025475),.UNSPECIFIED.);
#236=B_SPLINE_CURVE_WITH_KNOTS('',3,(#21287,#21288,#21289,#21290,#21291,
#21292,#21293,#21294,#21295),.UNSPECIFIED.,.F.,.F.,(4,1,1,1,1,1,4),(197.920343780393,
198.862557328576,199.860211623894,200.857865919213,201.855520214531,202.85317450985,
203.05545769227),.UNSPECIFIED.);
#237=B_SPLINE_CURVE_WITH_KNOTS('',3,(#21296,#21297,#21298,#21299,#21300,
#21301,#21302,#21303,#21304,#21305,#21306,#21307,#21308,#21309,#21310,#21311,
#21312,#21313,#21314,#21315,#21316,#21317,#21318,#21319,#21320,#21321,#21322,
#21323,#21324,#21325,#21326,#21327,#21328,#21329,#21330,#21331,#21332,#21333,
#21334,#21335,#21336,#21337,#21338,#21339,#21340,#21341,#21342,#21343,#21344,
#21345,#21346,#21347,#21348,#21349,#21350,#21351,#21352,#21353),
 .UNSPECIFIED.,.F.,.F.,(4,2,2,2,2,2,2,2,2,2,2,2,2,2,2,2,2,2,2,2,2,2,2,2,
2,2,2,2,4),(-1.9615148801207,-1.95785930310038,-1.95543652480846,-1.95436909446081,
-1.95358068958562,-1.95284838445205,-1.95211996770514,-1.95093027299669,
-1.94795677294164,-1.94237790205886,-1.90140356101455,-1.88263440278567,
-1.87821944696884,-1.87630059519408,-1.87488845379201,-1.87358232287792,
-1.87146013636454,-1.86618634365039,-1.83259983769925,-1.80945080302022,
-1.8032887874351,-1.80068993723764,-1.79928673563025,-1.79836335709454,
-1.79749796900988,-1.79674322859053,-1.79574856420446,-1.79369123295163,
-1.78229182699827),.UNSPECIFIED.);
#238=B_SPLINE_CURVE_WITH_KNOTS('',3,(#21355,#21356,#21357,#21358,#21359,
#21360,#21361,#21362,#21363,#21364,#21365,#21366,#21367,#21368,#21369,#21370,
#21371,#21372,#21373,#21374,#21375,#21376,#21377,#21378,#21379,#21380,#21381,
#21382,#21383,#21384,#21385,#21386,#21387,#21388,#21389,#21390,#21391,#21392,
#21393,#21394),.UNSPECIFIED.,.F.,.F.,(4,2,2,2,2,2,2,2,2,2,2,2,2,2,2,2,2,
2,2,4),(-0.179869993025475,-0.163811595497955,-0.142530502780673,-0.119886253534804,
-0.117769196411936,-0.116762987487965,-0.115985403780305,-0.115099048419803,
-0.114167300882653,-0.1108377978002,-0.0899917403801816,-0.0730740043608321,
-0.0445831457109489,-0.0411392387991886,-0.0393803473849921,-0.0379914470417024,
-0.0364376543779964,-0.0348298470050013,-0.0324345490511391,-0.000459757364235491),
 .UNSPECIFIED.);
#239=B_SPLINE_CURVE_WITH_KNOTS('',3,(#21395,#21396,#21397,#21398,#21399,
#21400,#21401,#21402,#21403,#21404,#21405,#21406,#21407,#21408,#21409,#21410,
#21411,#21412,#21413,#21414,#21415,#21416,#21417,#21418,#21419,#21420,#21421,
#21422,#21423,#21424,#21425,#21426,#21427,#21428,#21429,#21430,#21431,#21432,
#21433,#21434,#21435,#21436,#21437,#21438,#21439,#21440,#21441,#21442,#21443,
#21444,#21445,#21446,#21447,#21448,#21449,#21450,#21451,#21452,#21453,#21454,
#21455,#21456,#21457,#21458,#21459,#21460,#21461,#21462,#21463,#21464,#21465,
#21466,#21467,#21468,#21469,#21470,#21471,#21472,#21473,#21474,#21475,#21476,
#21477,#21478,#21479,#21480,#21481,#21482,#21483,#21484,#21485,#21486,#21487,
#21488,#21489,#21490,#21491,#21492,#21493,#21494,#21495,#21496,#21497,#21498,
#21499,#21500,#21501,#21502,#21503,#21504,#21505,#21506,#21507,#21508,#21509,
#21510,#21511,#21512,#21513,#21514,#21515,#21516,#21517,#21518,#21519,#21520,
#21521,#21522,#21523,#21524,#21525,#21526,#21527,#21528,#21529,#21530,#21531,
#21532,#21533,#21534,#21535,#21536,#21537,#21538,#21539,#21540,#21541,#21542,
#21543,#21544,#21545,#21546,#21547,#21548,#21549,#21550,#21551,#21552,#21553,
#21554,#21555,#21556,#21557,#21558,#21559,#21560,#21561,#21562,#21563,#21564,
#21565,#21566,#21567,#21568,#21569,#21570,#21571,#21572,#21573,#21574,#21575,
#21576,#21577,#21578,#21579,#21580,#21581,#21582),.UNSPECIFIED.,.F.,.F.,
(4,2,2,2,2,2,2,2,2,2,2,2,2,2,2,2,2,2,2,2,2,2,2,2,2,2,2,2,2,2,2,2,2,2,2,
2,2,2,2,2,2,2,2,2,2,2,2,2,2,2,2,2,2,2,2,2,2,2,2,2,2,2,2,2,2,2,2,2,2,2,2,
2,2,2,2,2,2,2,2,2,2,2,2,2,2,2,2,2,2,2,2,2,2,4),(-1.96082658239079,-1.92602912275097,
-1.92391265918641,-1.9226980023526,-1.9216113461444,-1.92082269324694,-1.92008050876462,
-1.91881711121155,-1.91537410270121,-1.88549619304636,-1.87029251594664,
-1.85123746030756,-1.84653828417131,-1.84500099645138,-1.84349630338714,
-1.84209558600681,-1.84027263360582,-1.83721681887257,-1.81498141790064,
-1.78387566150072,-1.7735473936807,-1.76796809773533,-1.76651269513947,
-1.76563914191328,-1.76485956308448,-1.76385017322892,-1.7621661638449,
-1.75169513583186,-1.75143077427964,-1.74526404675889,-1.71116843487286,
-1.69922104241752,-1.69179772305969,-1.68950304768023,-1.6882005043922,
-1.68681692635051,-1.68510822134661,-1.68249527967644,-1.67037002298248,
-1.66468534211715,-1.62046716655693,-1.61265153424839,-1.61102929622464,
-1.61012546600139,-1.60935069797371,-1.60837150360438,-1.60638992851264,
-1.59316982774372,-1.54889067676612,-1.53690975383071,-1.53415416904679,
-1.5325651748407,-1.53118187495095,-1.52947826479315,-1.5268819275384,-1.51499890060777,
-1.50909516957812,-1.46501732898557,-1.45702103002851,-1.45538788533665,
-1.45448164846656,-1.45370706322193,-1.45273096851452,-1.45082775571268,
-1.43903885429282,-1.43503553418016,-1.42284034116326,-1.39453250422579,
-1.38144163821978,-1.37861227308363,-1.37700694565556,-1.37576354494997,
-1.37413908691075,-1.37130043900867,-1.3595609458052,-1.35352347109607,
-1.30951854092663,-1.3014181039286,-1.29977865386854,-1.29887095626339,
-1.29809636308121,-1.29712183918595,-1.29522635196791,-1.28364126863433,
-1.24625480834406,-1.23302398021995,-1.22500268161307,-1.22258984808002,
-1.22107642036994,-1.21967807384737,-1.21787299353315,-1.21487936627816,
-1.19521268181508,-1.16013501283535),.UNSPECIFIED.);
#240=B_SPLINE_CURVE_WITH_KNOTS('',3,(#21588,#21589,#21590,#21591,#21592,
#21593,#21594,#21595,#21596,#21597,#21598,#21599,#21600,#21601,#21602,#21603,
#21604,#21605,#21606,#21607,#21608,#21609,#21610,#21611,#21612,#21613,#21614,
#21615,#21616,#21617,#21618,#21619,#21620,#21621,#21622,#21623,#21624,#21625,
#21626,#21627,#21628,#21629,#21630,#21631,#21632,#21633,#21634,#21635,#21636,
#21637,#21638,#21639,#21640,#21641,#21642,#21643,#21644,#21645,#21646,#21647,
#21648,#21649,#21650,#21651,#21652,#21653,#21654,#21655,#21656,#21657,#21658,
#21659,#21660,#21661,#21662,#21663,#21664,#21665,#21666,#21667,#21668,#21669),
 .UNSPECIFIED.,.F.,.F.,(4,3,3,3,3,3,3,3,3,3,3,3,3,3,3,3,3,3,3,3,3,3,3,3,
3,3,3,4),(204.203522483337,204.4022267974,204.600944713539,204.800173276778,
204.848483100487,205.047025400352,205.246803399215,205.444888946928,205.645513171366,
205.846137395805,206.044679670632,206.244457675755,206.442543198879,206.643167445002,
206.843791691124,207.042333982541,207.242111983516,207.440197522141,207.640821754292,
207.841445986442,208.039988334246,208.239766321125,208.437851916756,208.638476099258,
208.839100281761,209.037642471706,209.235805250642,209.337753800715),
 .UNSPECIFIED.);
#241=B_SPLINE_CURVE_WITH_KNOTS('',3,(#21670,#21671,#21672,#21673,#21674),
 .UNSPECIFIED.,.F.,.F.,(4,1,4),(203.05545769227,203.850828805168,204.203515180604),
 .UNSPECIFIED.);
#242=B_SPLINE_CURVE_WITH_KNOTS('',3,(#21675,#21676,#21677,#21678,#21679,
#21680,#21681,#21682,#21683,#21684,#21685,#21686,#21687,#21688,#21689,#21690,
#21691,#21692,#21693,#21694,#21695,#21696,#21697,#21698,#21699,#21700,#21701,
#21702,#21703,#21704,#21705,#21706,#21707,#21708,#21709,#21710,#21711,#21712,
#21713,#21714,#21715,#21716,#21717,#21718,#21719,#21720,#21721,#21722,#21723,
#21724,#21725,#21726,#21727,#21728,#21729,#21730,#21731,#21732,#21733,#21734,
#21735,#21736,#21737,#21738,#21739,#21740,#21741,#21742,#21743,#21744,#21745,
#21746,#21747,#21748,#21749,#21750,#21751,#21752,#21753,#21754,#21755,#21756,
#21757,#21758,#21759,#21760,#21761,#21762,#21763,#21764,#21765,#21766,#21767,
#21768,#21769,#21770,#21771,#21772,#21773,#21774,#21775,#21776,#21777,#21778,
#21779,#21780,#21781,#21782,#21783,#21784,#21785,#21786,#21787,#21788,#21789,
#21790,#21791,#21792,#21793,#21794,#21795,#21796,#21797,#21798,#21799,#21800,
#21801,#21802,#21803,#21804,#21805,#21806,#21807,#21808,#21809,#21810,#21811,
#21812,#21813,#21814,#21815,#21816,#21817,#21818,#21819,#21820,#21821,#21822,
#21823,#21824,#21825,#21826,#21827,#21828,#21829,#21830,#21831,#21832,#21833,
#21834,#21835,#21836,#21837,#21838,#21839,#21840,#21841,#21842,#21843,#21844,
#21845,#21846,#21847,#21848,#21849,#21850,#21851,#21852,#21853,#21854,#21855,
#21856,#21857,#21858,#21859,#21860,#21861,#21862,#21863,#21864,#21865,#21866,
#21867,#21868,#21869,#21870,#21871,#21872,#21873,#21874,#21875,#21876,#21877,
#21878,#21879,#21880,#21881,#21882,#21883,#21884,#21885,#21886,#21887,#21888,
#21889,#21890,#21891,#21892,#21893,#21894,#21895,#21896,#21897,#21898,#21899,
#21900,#21901,#21902,#21903,#21904,#21905,#21906,#21907,#21908,#21909,#21910,
#21911,#21912,#21913,#21914,#21915,#21916,#21917,#21918,#21919,#21920,#21921,
#21922,#21923,#21924,#21925,#21926,#21927,#21928,#21929,#21930),
 .UNSPECIFIED.,.F.,.F.,(4,2,2,2,2,2,2,2,2,2,2,2,2,2,2,2,2,2,2,2,2,2,2,2,
2,2,2,2,2,2,2,2,2,2,2,2,2,2,2,2,2,2,2,2,2,2,2,2,2,2,2,2,2,2,2,2,2,2,2,2,
2,2,2,2,2,2,2,2,2,2,2,2,2,2,2,2,2,2,2,2,2,2,2,2,2,2,2,2,2,2,2,2,2,2,2,2,
2,2,2,2,2,2,2,2,2,2,2,2,2,2,2,2,2,2,2,2,2,2,2,2,2,2,2,2,2,2,2,4),(-1.16013501283535,
-1.15244795152998,-1.14561574671098,-1.14405785862302,-1.14316796281657,
-1.14239113281632,-1.14139098574942,-1.13930453000753,-1.12155879054906,
-1.09167128973203,-1.07269589882701,-1.06825554410622,-1.06633264804388,
-1.06492018332803,-1.06361562372442,-1.06150018992778,-1.0562636372972,
-1.02098865865973,-1.00498955056935,-0.99517620192596,-0.991582552993478,
-0.989012495185446,-0.987923765088775,-0.987134443174618,-0.986392295414844,
-0.985342381568503,-0.982508762486278,-0.980953553527101,-0.952012391238002,
-0.918350586309311,-0.913079577190366,-0.910958308611932,-0.909652689997913,
-0.908241058428202,-0.906322830921879,-0.90190904444032,-0.883141086531339,
-0.853124549737448,-0.845103438767711,-0.834863311384136,-0.833189896800554,
-0.832183388219915,-0.831403900133244,-0.830528054587987,-0.829033612197652,
-0.823031946695105,-0.811591119013575,-0.780653141438465,-0.759778577490916,
-0.756754755791123,-0.754940706370542,-0.753540859388188,-0.7520312076194,
-0.74963598827415,-0.741778826998395,-0.728922166577821,-0.692375048878608,
-0.679419274860688,-0.677470427286,-0.676484403497884,-0.675708852049611,
-0.674809380282094,-0.673207993034462,-0.665732235130786,-0.62124138524943,
-0.615914951783187,-0.60338383301454,-0.600742799493143,-0.599025021989373,
-0.59764024315472,-0.596060510556278,-0.593348600081016,-0.581983521160895,
-0.537220440924614,-0.523739574703585,-0.521748787742838,-0.520767512871396,
-0.519992308623926,-0.519089353841843,-0.517472144703771,-0.509745723692276,
-0.465459555989856,-0.459877296554102,-0.447636426779179,-0.445014459664544,
-0.44330253723789,-0.441918143321858,-0.440334105199491,-0.437602859622623,
-0.425975414710597,-0.381401070394554,-0.368021802137539,-0.366034222576292,
-0.365053564513879,-0.364278375918171,-0.363374897577985,-0.361755401947534,
-0.353992651323872,-0.309733627887707,-0.304110693997192,-0.291913970427097,
-0.289295319536869,-0.287584383497084,-0.286200005011609,-0.286196352880906,
-0.286192720827022,-0.286189109127128,-0.286185517613882,-0.286181946115099,
-0.286178394471249,-0.286174862517547,-0.286171350091802,-0.286167857030312,
-0.286164383175913,-0.284598023349195,-0.281922495827144,-0.27866106761613,
-0.272004267093479,-0.226684740495946,-0.223551865373127,-0.212159378920945,
-0.210270804662788,-0.209297472368981,-0.208522581740232,-0.207613088393781,
-0.205966721704878,-0.197756983940576,-0.179683013393011),.UNSPECIFIED.);
#243=B_SPLINE_CURVE_WITH_KNOTS('',3,(#21936,#21937,#21938,#21939,#21940,
#21941,#21942,#21943,#21944,#21945,#21946,#21947,#21948,#21949,#21950,#21951,
#21952,#21953,#21954,#21955,#21956,#21957,#21958,#21959,#21960,#21961,#21962,
#21963,#21964,#21965,#21966,#21967,#21968,#21969,#21970,#21971,#21972,#21973,
#21974,#21975,#21976,#21977,#21978,#21979,#21980,#21981,#21982,#21983,#21984,
#21985,#21986,#21987,#21988,#21989,#21990,#21991,#21992,#21993,#21994,#21995,
#21996,#21997,#21998,#21999,#22000,#22001,#22002,#22003,#22004,#22005,#22006,
#22007,#22008,#22009,#22010,#22011,#22012,#22013,#22014,#22015,#22016,#22017,
#22018,#22019,#22020,#22021,#22022,#22023,#22024,#22025,#22026,#22027,#22028,
#22029,#22030,#22031,#22032,#22033,#22034,#22035,#22036,#22037,#22038,#22039,
#22040,#22041,#22042,#22043,#22044,#22045,#22046,#22047,#22048,#22049,#22050,
#22051,#22052,#22053,#22054,#22055,#22056,#22057,#22058,#22059,#22060,#22061,
#22062,#22063,#22064,#22065,#22066,#22067,#22068,#22069,#22070,#22071,#22072,
#22073,#22074,#22075,#22076,#22077,#22078,#22079,#22080,#22081,#22082,#22083,
#22084,#22085,#22086,#22087,#22088,#22089,#22090,#22091,#22092,#22093,#22094,
#22095,#22096,#22097,#22098,#22099,#22100,#22101,#22102,#22103,#22104,#22105,
#22106,#22107,#22108,#22109,#22110,#22111,#22112,#22113,#22114,#22115,#22116,
#22117),.UNSPECIFIED.,.F.,.F.,(4,2,2,2,2,2,2,2,2,2,2,2,2,2,2,2,2,2,2,2,
2,2,2,2,2,2,2,2,2,2,2,2,2,2,2,2,2,2,2,2,2,2,2,2,2,2,2,2,2,2,2,2,2,2,2,2,
2,2,2,2,2,2,2,2,2,2,2,2,2,2,2,2,2,2,2,2,2,2,2,2,2,2,2,2,2,2,2,2,2,2,4),
(-0.801755247281622,-0.78086201411725,-0.761282731388872,-0.758289959061391,
-0.756484478492026,-0.755085286016964,-0.75357040783494,-0.751154103284936,
-0.743110564267746,-0.729829646726836,-0.69250539174903,-0.680862109261831,
-0.678963244350437,-0.677987581088989,-0.677212339088328,-0.676304133469897,
-0.674664643021354,-0.666580951608885,-0.622539809537711,-0.616439439894876,
-0.604762977396565,-0.601927603904639,-0.600302913425538,-0.599058225915042,
-0.597449916624031,-0.594611455031511,-0.581407033654533,-0.552659239739768,
-0.525359636983343,-0.523297617902993,-0.522301774821857,-0.521524832642854,
-0.520630910515257,-0.519056561998955,-0.511999749847502,-0.46836910385605,
-0.459292426077767,-0.457929708764234,-0.448646406687241,-0.445996975423015,
-0.444430373126496,-0.443181592086351,-0.441506830318308,-0.438358562770144,
-0.418488401102963,-0.380968651225515,-0.369399812699514,-0.367503822308947,
-0.366528744988159,-0.365753554817715,-0.364844959510768,-0.363203384903601,
-0.355081681308867,-0.311075568993249,-0.304943900381447,-0.293305699768569,
-0.290473727609101,-0.288849967611286,-0.287605456890989,-0.286028835564392,
-0.283307911589251,-0.27997955813019,-0.25723037982761,-0.243289374138446,
-0.216010296347387,-0.212519401424734,-0.211247820435019,-0.210503472899165,
-0.20971470939341,-0.208631451720734,-0.206095448663128,-0.178171937163344,
-0.140901328534064,-0.135997095718667,-0.13414214919743,-0.132816039415444,
-0.131480976478667,-0.129707507675679,-0.126058957312403,-0.12127959948803,
-0.10991348618691,-0.0949394951243235,-0.0599704736272973,-0.0567348544962777,
-0.0555022377686479,-0.0547654854864833,-0.053971680163666,-0.0528598336409613,
-0.0501551366038624,-0.0463178883774756,-0.000462826290749375),
 .UNSPECIFIED.);
#244=B_SPLINE_CURVE_WITH_KNOTS('',3,(#22118,#22119,#22120,#22121,#22122,
#22123,#22124,#22125,#22126,#22127,#22128,#22129,#22130,#22131,#22132,#22133,
#22134,#22135,#22136,#22137,#22138,#22139),.UNSPECIFIED.,.F.,.F.,(4,3,3,
3,3,3,3,4),(209.337753800715,209.535821987683,209.734362197183,209.836754577079,
210.035772951847,210.23433093735,210.432737935524,210.486707790516),
 .UNSPECIFIED.);
#245=B_SPLINE_CURVE_WITH_KNOTS('',3,(#22141,#22142,#22143,#22144,#22145,
#22146,#22147,#22148,#22149,#22150,#22151,#22152,#22153,#22154,#22155,#22156,
#22157,#22158,#22159,#22160,#22161,#22162,#22163,#22164,#22165,#22166,#22167,
#22168,#22169,#22170,#22171,#22172,#22173,#22174,#22175,#22176,#22177,#22178,
#22179,#22180,#22181,#22182,#22183,#22184,#22185,#22186,#22187,#22188,#22189,
#22190,#22191,#22192,#22193,#22194,#22195,#22196,#22197,#22198,#22199,#22200),
 .UNSPECIFIED.,.F.,.F.,(4,2,2,2,2,2,2,2,2,2,2,2,2,2,2,2,2,2,2,2,2,2,2,2,
2,2,2,2,2,4),(-0.179683013393011,-0.153833929778708,-0.147651743902397,
-0.136066129701737,-0.133238916153645,-0.131616500613473,-0.130372292347068,
-0.130361163143912,-0.130344843018896,-0.13032883620451,-0.130313134155593,
-0.130297727819773,-0.130282606547122,-0.130267761318402,-0.130253183474055,
-0.130238864690741,-0.128608632247454,-0.125657092723767,-0.121971128085402,
-0.114079103967532,-0.0957409663085824,-0.0797737773767086,-0.056779181564577,
-0.0546625224908131,-0.0536563157597635,-0.052878648238301,-0.0519921021928767,
-0.0504501672964389,-0.0438423698564559,-0.000460287074351403),
 .UNSPECIFIED.);
#246=B_SPLINE_CURVE_WITH_KNOTS('',3,(#22201,#22202,#22203,#22204,#22205,
#22206,#22207,#22208,#22209,#22210,#22211,#22212,#22213,#22214,#22215,#22216,
#22217,#22218,#22219,#22220,#22221,#22222,#22223,#22224,#22225,#22226,#22227,
#22228,#22229,#22230,#22231,#22232,#22233,#22234,#22235,#22236,#22237,#22238,
#22239,#22240,#22241,#22242,#22243,#22244,#22245,#22246,#22247,#22248,#22249,
#22250,#22251,#22252,#22253,#22254,#22255,#22256,#22257,#22258,#22259,#22260,
#22261,#22262,#22263,#22264,#22265,#22266,#22267,#22268,#22269,#22270,#22271,
#22272,#22273,#22274,#22275,#22276,#22277,#22278,#22279,#22280,#22281,#22282),
 .UNSPECIFIED.,.F.,.F.,(4,3,3,3,3,3,3,3,3,3,3,3,3,3,3,3,3,3,3,3,3,3,3,3,
3,3,3,4),(210.486707790516,210.684874749739,210.88302187909,211.081668186406,
211.146280582813,211.344822930682,211.544600917545,211.74268651324,211.943310695686,
212.143934878132,212.34247704944,212.542255080443,212.740340502248,212.940964837849,
213.14158917345,213.340131504725,213.539909495736,213.737995069762,213.938619269265,
214.139243468769,214.337786108943,214.537564022729,214.735649911972,214.93627383803,
215.136897764087,215.335440942814,215.533590738744,215.620984071508),
 .UNSPECIFIED.);
#247=B_SPLINE_CURVE_WITH_KNOTS('',3,(#22287,#22288,#22289,#22290,#22291,
#22292,#22293,#22294,#22295,#22296,#22297,#22298,#22299,#22300,#22301,#22302,
#22303,#22304,#22305,#22306,#22307,#22308,#22309,#22310,#22311,#22312,#22313,
#22314,#22315,#22316,#22317,#22318,#22319,#22320,#22321,#22322,#22323,#22324,
#22325,#22326,#22327,#22328,#22329,#22330,#22331,#22332,#22333,#22334,#22335,
#22336,#22337,#22338,#22339,#22340,#22341,#22342,#22343,#22344,#22345,#22346,
#22347,#22348,#22349,#22350,#22351,#22352,#22353,#22354,#22355,#22356,#22357,
#22358,#22359,#22360,#22361,#22362,#22363,#22364,#22365,#22366,#22367,#22368,
#22369,#22370,#22371,#22372,#22373,#22374,#22375,#22376,#22377,#22378,#22379,
#22380,#22381,#22382,#22383,#22384,#22385,#22386,#22387,#22388,#22389,#22390,
#22391,#22392,#22393,#22394,#22395,#22396,#22397,#22398,#22399,#22400,#22401,
#22402,#22403,#22404,#22405,#22406,#22407,#22408,#22409,#22410,#22411,#22412,
#22413,#22414,#22415,#22416,#22417,#22418,#22419,#22420,#22421,#22422,#22423,
#22424,#22425,#22426,#22427,#22428,#22429,#22430,#22431,#22432,#22433,#22434,
#22435,#22436,#22437,#22438,#22439,#22440,#22441,#22442,#22443,#22444,#22445,
#22446,#22447,#22448,#22449,#22450,#22451,#22452,#22453,#22454,#22455,#22456,
#22457,#22458,#22459,#22460,#22461,#22462,#22463,#22464,#22465,#22466,#22467,
#22468,#22469,#22470,#22471,#22472,#22473,#22474,#22475,#22476,#22477,#22478,
#22479,#22480,#22481,#22482,#22483,#22484,#22485,#22486,#22487,#22488,#22489,
#22490,#22491,#22492,#22493,#22494,#22495,#22496,#22497,#22498,#22499,#22500,
#22501,#22502,#22503,#22504,#22505,#22506,#22507,#22508,#22509,#22510,#22511,
#22512,#22513,#22514,#22515,#22516,#22517,#22518,#22519,#22520),
 .UNSPECIFIED.,.F.,.F.,(4,2,2,2,2,2,2,2,2,2,2,2,2,2,2,2,2,2,2,2,2,2,2,2,
2,2,2,2,2,2,2,2,2,2,2,2,2,2,2,2,2,2,2,2,2,2,2,2,2,2,2,2,2,2,2,2,2,2,2,2,
2,2,2,2,2,2,2,2,2,2,2,2,2,2,2,2,2,2,2,2,2,2,2,2,2,2,2,2,2,2,2,2,2,2,2,2,
2,2,2,2,2,2,2,2,2,2,2,2,2,2,2,2,2,2,2,2,4),(-1.78243981456369,-1.77781910849269,
-1.77045667882715,-1.76886762186785,-1.76796289004524,-1.76718965527803,
-1.76621499263851,-1.764240560818,-1.751023706825,-1.7496780453941,-1.70453298226282,
-1.6944549873362,-1.69190889410289,-1.69034169332121,-1.6889664160694,-1.68725857376783,
-1.68462953443928,-1.67211062151324,-1.66595586433131,-1.62259226068631,
-1.61451420740382,-1.61288487756901,-1.61198374080067,-1.61121066848732,
-1.61023637536237,-1.60834470707781,-1.59689176458797,-1.59404751390318,
-1.59069275844223,-1.54734791285111,-1.53820385320524,-1.53567261217881,
-1.53412964097899,-1.53273329188368,-1.53094123994273,-1.52806686633859,
-1.51152490377523,-1.4667479288529,-1.45895712885065,-1.45733025785726,
-1.45642232404805,-1.45564445933202,-1.45466112995711,-1.45266603575424,
-1.43913436595251,-1.39384131902477,-1.38304352560909,-1.38037318429321,
-1.37880157066246,-1.37741408958584,-1.37568005264275,-1.37298943766206,
-1.35971748488825,-1.35515658228287,-1.31091107188864,-1.30315587089286,
-1.30153643728556,-1.30063280390261,-1.29985770089437,-1.29887732508598,
-1.29689000238447,-1.28350173658133,-1.23902096997954,-1.22732632743332,
-1.2245910241943,-1.22300652779084,-1.22162286985777,-1.21991333101168,
-1.21729776680558,-1.20513637915205,-1.16702814691573,-1.15384258508155,
-1.14725040957389,-1.14571042103203,-1.144824739813,-1.14404699333597,-1.1430400854616,
-1.14092126462828,-1.11907332751573,-1.09149667020153,-1.07875250813313,
-1.07094167312938,-1.0685498218238,-1.06703978132904,-1.06563783603358,
-1.06381859648723,-1.06078064219458,-1.03944602358168,-1.013296717493,-0.992392256212847,
-0.990390079119862,-0.989405759764212,-0.988703228678187,-0.987827985072771,
-0.986338397977094,-0.981110592730136,-0.971501591535719,-0.937451337526512,
-0.917028200318629,-0.914014410714383,-0.912202653056938,-0.910802372715922,
-0.909290067798029,-0.906885942408039,-0.898956932868385,-0.885939901310233,
-0.848547469404808,-0.846257713720262,-0.836421630151211,-0.834767107765206,
-0.833765838297843,-0.832986616635607,-0.832106820659761,-0.830596005665425,
-0.824398396726793,-0.812397727156659,-0.801755247281622),.UNSPECIFIED.);
#248=B_SPLINE_CURVE_WITH_KNOTS('',3,(#22522,#22523,#22524,#22525,#22526,
#22527,#22528,#22529,#22530,#22531,#22532,#22533,#22534,#22535,#22536,#22537,
#22538,#22539,#22540,#22541,#22542,#22543),.UNSPECIFIED.,.F.,.F.,(4,3,3,
3,3,3,3,4),(215.620984071508,215.819050588149,216.017592804227,216.134552059406,
216.334181857737,216.533339860188,216.732307834584,216.769893097696),
 .UNSPECIFIED.);
#249=B_SPLINE_CURVE_WITH_KNOTS('',3,(#22544,#22545,#22546,#22547,#22548,
#22549,#22550,#22551,#22552,#22553,#22554,#22555,#22556,#22557,#22558,#22559,
#22560,#22561,#22562,#22563,#22564,#22565,#22566,#22567,#22568,#22569,#22570,
#22571,#22572,#22573,#22574,#22575,#22576,#22577,#22578,#22579,#22580,#22581,
#22582,#22583,#22584,#22585,#22586,#22587,#22588,#22589,#22590,#22591,#22592,
#22593,#22594,#22595,#22596,#22597,#22598,#22599,#22600,#22601,#22602,#22603,
#22604,#22605,#22606,#22607,#22608,#22609,#22610,#22611,#22612,#22613,#22614,
#22615,#22616,#22617,#22618,#22619,#22620,#22621,#22622,#22623,#22624,#22625,
#22626,#22627,#22628,#22629,#22630,#22631,#22632,#22633,#22634,#22635,#22636,
#22637,#22638,#22639,#22640,#22641,#22642,#22643,#22644,#22645,#22646,#22647,
#22648,#22649,#22650,#22651,#22652,#22653,#22654,#22655,#22656,#22657,#22658,
#22659,#22660,#22661,#22662,#22663,#22664,#22665,#22666,#22667,#22668,#22669,
#22670,#22671,#22672,#22673,#22674,#22675,#22676,#22677,#22678,#22679,#22680,
#22681,#22682,#22683,#22684,#22685,#22686,#22687,#22688,#22689,#22690,#22691,
#22692,#22693,#22694,#22695,#22696,#22697,#22698,#22699,#22700,#22701,#22702,
#22703,#22704,#22705,#22706,#22707,#22708,#22709,#22710,#22711,#22712,#22713,
#22714,#22715,#22716,#22717,#22718,#22719,#22720,#22721,#22722,#22723,#22724,
#22725,#22726,#22727,#22728,#22729,#22730,#22731,#22732,#22733,#22734,#22735,
#22736,#22737,#22738,#22739,#22740,#22741,#22742,#22743,#22744,#22745,#22746,
#22747,#22748,#22749,#22750,#22751,#22752,#22753,#22754,#22755,#22756,#22757,
#22758,#22759,#22760,#22761,#22762,#22763,#22764,#22765,#22766,#22767,#22768,
#22769,#22770,#22771,#22772,#22773,#22774,#22775,#22776,#22777),
 .UNSPECIFIED.,.F.,.F.,(4,2,2,2,2,2,2,2,2,2,2,2,2,2,2,2,2,2,2,2,2,2,2,2,
2,2,2,2,2,2,2,2,2,2,2,2,2,2,2,2,2,2,2,2,2,2,2,2,2,2,2,2,2,2,2,2,2,2,2,2,
2,2,2,2,2,2,2,2,2,2,2,2,2,2,2,2,2,2,2,2,2,2,2,2,2,2,2,2,2,2,2,2,2,2,2,2,
2,2,2,2,2,2,2,2,2,2,2,2,2,2,2,2,2,2,2,2,4),(0.801779048931175,0.837019428551869,
0.842251000008229,0.844364256943249,0.8456674029493,0.847078273207283,0.848998871291302,
0.85343323992529,0.872375231227022,0.89536395452256,0.909893793462966,0.920405701387156,
0.922090746550154,0.923100051204982,0.923879420356136,0.924753001182252,
0.926237117106791,0.932113343220088,0.943202918540473,0.965286187621122,
0.972061840758756,0.995440331953748,0.998522268183578,1.00035364490514,
1.00175668521912,1.00325982405532,1.00562366804595,1.01319424345447,1.02540428513485,
1.04958762899285,1.06292102961666,1.07579436658856,1.07774089166114,1.07872675105735,
1.07950254252534,1.08040261592641,1.08200663665984,1.08952253460432,1.13401090295301,
1.13943419408526,1.15185317753889,1.1544865534054,1.15620179683352,1.15758615787785,
1.1591671869967,1.16188577149141,1.17334577260415,1.21798985728666,1.23144976926967,
1.23343934169617,1.23442017684465,1.2351950966167,1.2360977685617,1.237714661135,
1.24544267181117,1.28973072566158,1.30704293533181,1.3099400120814,1.31173552938767,
1.31312796223201,1.31460743893859,1.31697911193565,1.31979298365672,1.32521473453014,
1.33884041088381,1.37251068040171,1.37494023736084,1.37837826462356,1.38740059305954,
1.38901232829137,1.39001100327299,1.39078742466878,1.39167772253962,1.3932381313028,
1.40011014733151,1.4430052825361,1.46248832628739,1.46547466519161,1.46727738229634,
1.46867510415258,1.46871509302788,1.46873895559707,1.46876950891625,1.46879713079223,
1.46882214224099,1.46884482211883,1.46886541544488,1.4688841372923,1.46890117672574,
1.46891670076855,1.46893085740554,1.46894377812929,1.46895558008434,1.46897201594382,
1.46898812916944,1.46900392876709,1.46901942553776,1.46903462989518,1.4690495512811,
1.46906419875769,1.46907858102038,1.47070128375678,1.47363365309485,1.47728287114657,
1.48506720671879,1.50317813768614,1.52863612831214,1.53221362698308,1.54282936168681,
1.54451980939672,1.54553112896458,1.54631100333078,1.54718353029088,1.5486641556082,
1.55450486038028,1.56549818412402,1.60250354857828),.UNSPECIFIED.);
#250=B_SPLINE_CURVE_WITH_KNOTS('',3,(#22781,#22782,#22783,#22784,#22785,
#22786,#22787,#22788,#22789,#22790,#22791,#22792,#22793,#22794,#22795,#22796,
#22797,#22798,#22799,#22800,#22801,#22802,#22803,#22804,#22805,#22806,#22807,
#22808,#22809,#22810,#22811,#22812,#22813,#22814,#22815,#22816,#22817),
 .UNSPECIFIED.,.F.,.F.,(4,3,3,3,3,3,3,3,3,3,3,3,4),(-4.0925417488383,-3.99061718127404,
-3.80271607511609,-3.61521129929871,-3.42774226886674,-3.24028946643165,
-3.0524192190311,-2.99296288595553,-2.80713361459988,-2.62153830198906,
-2.43611803811621,-2.25027574028768,-2.0654894469632),.UNSPECIFIED.);
#251=B_SPLINE_CURVE_WITH_KNOTS('',3,(#22821,#22822,#22823,#22824,#22825,
#22826,#22827,#22828,#22829,#22830,#22831,#22832,#22833,#22834,#22835,#22836,
#22837,#22838,#22839,#22840,#22841,#22842),.UNSPECIFIED.,.F.,.F.,(4,3,3,
3,3,3,3,4),(0.,0.192029026907948,0.393435344010587,0.58555661568393,0.777819410374763,
0.970607640201115,0.997654295318505,1.11419103802989),.UNSPECIFIED.);
#252=B_SPLINE_CURVE_WITH_KNOTS('',3,(#22844,#22845,#22846,#22847,#22848,
#22849,#22850,#22851,#22852,#22853,#22854,#22855,#22856,#22857,#22858,#22859,
#22860,#22861,#22862,#22863,#22864,#22865,#22866,#22867,#22868,#22869,#22870,
#22871,#22872,#22873,#22874,#22875,#22876,#22877,#22878,#22879,#22880,#22881,
#22882,#22883,#22884,#22885,#22886,#22887,#22888,#22889,#22890,#22891,#22892,
#22893,#22894,#22895,#22896,#22897,#22898,#22899,#22900,#22901,#22902,#22903,
#22904,#22905,#22906,#22907,#22908,#22909,#22910,#22911,#22912,#22913,#22914,
#22915,#22916,#22917,#22918,#22919,#22920,#22921,#22922,#22923,#22924,#22925,
#22926,#22927,#22928,#22929,#22930,#22931,#22932,#22933,#22934,#22935,#22936,
#22937,#22938,#22939,#22940,#22941,#22942,#22943,#22944,#22945,#22946,#22947,
#22948,#22949,#22950,#22951,#22952,#22953,#22954,#22955),.UNSPECIFIED.,
 .F.,.F.,(4,3,3,3,3,3,3,3,3,3,3,3,3,3,3,3,3,3,3,3,3,3,3,3,3,3,3,3,3,3,3,
3,3,3,3,3,3,4),(1.11419103844207,1.29729781656767,1.48020848463403,1.6629748443953,
1.84617221538369,1.99530859063702,2.18313685847596,2.37057148514672,2.55797502099778,
2.74536494778383,2.93317706372225,2.99296288595553,3.18083272060202,3.3683199864994,
3.55579169057548,3.74325886950682,3.93116039865387,3.99061718127404,4.17789585759714,
4.36477521905835,4.55162388290638,4.73845861120085,4.92572539060956,4.98827147659255,
5.17586619279521,5.36306763434357,5.55024230049996,5.73740566481817,5.92499894751711,
5.98592577191106,6.17350335525126,6.36068874716866,6.54784921468969,6.73499944084289,
6.92258141640707,6.98358006722958,7.19047800572963,7.39737594422968),
 .UNSPECIFIED.);
#253=B_SPLINE_CURVE_WITH_KNOTS('',3,(#22957,#22958,#22959,#22960,#22961,
#22962,#22963,#22964,#22965,#22966),.UNSPECIFIED.,.F.,.F.,(4,1,1,1,1,1,
1,4),(7.39737634520948,7.98123436254809,8.97888865786661,9.97654295318512,
10.9741972485036,11.9718515438221,12.9695058391407,13.6805616523891),
 .UNSPECIFIED.);
#254=B_SPLINE_CURVE_WITH_KNOTS('',3,(#22968,#22969,#22970,#22971,#22972,
#22973,#22974,#22975,#22976,#22977,#22978),.UNSPECIFIED.,.F.,.F.,(4,1,1,
1,1,1,1,1,4),(13.6805616523891,13.9671601344592,14.9648144297777,15.9624687250962,
16.9601230204147,17.9577773157332,18.9554316110517,19.9530859063702,19.9637469595687),
 .UNSPECIFIED.);
#255=B_SPLINE_CURVE_WITH_KNOTS('',3,(#22980,#22981,#22982,#22983,#22984,
#22985,#22986,#22987,#22988,#22989,#22990,#22991,#22992,#22993,#22994,#22995,
#22996,#22997,#22998,#22999,#23000,#23001,#23002,#23003,#23004,#23005,#23006,
#23007,#23008,#23009,#23010,#23011,#23012,#23013,#23014,#23015,#23016,#23017,
#23018,#23019,#23020,#23021,#23022,#23023,#23024,#23025,#23026,#23027,#23028,
#23029,#23030,#23031,#23032,#23033,#23034,#23035,#23036,#23037,#23038,#23039,
#23040,#23041,#23042,#23043,#23044,#23045,#23046,#23047,#23048,#23049,#23050,
#23051,#23052,#23053,#23054,#23055,#23056,#23057,#23058,#23059,#23060,#23061,
#23062,#23063,#23064,#23065,#23066,#23067,#23068,#23069,#23070,#23071,#23072,
#23073,#23074,#23075,#23076,#23077,#23078,#23079,#23080,#23081,#23082,#23083,
#23084,#23085,#23086,#23087,#23088,#23089,#23090,#23091,#23092,#23093,#23094),
 .UNSPECIFIED.,.F.,.F.,(4,3,3,3,3,3,3,3,3,3,3,3,3,3,3,3,3,3,3,3,3,3,3,3,
3,3,3,3,3,3,3,3,3,3,3,3,3,3,4),(19.9637469595687,20.1509331180402,20.3377271974283,
20.5244962077931,20.7112586063894,20.8984478398483,20.9507402016887,21.1382782494911,
21.3254226909156,21.5125407629289,21.6996477118573,21.8871858954244,21.9483944970072,
22.1359325437719,22.3230769840842,22.5101950548933,22.6973020025625,22.8848401848119,
22.9460487923258,23.1335868421645,23.3207312856336,23.5078493596721,23.6949563106163,
23.882494496148,23.9437030876443,24.1312411360172,24.318385577994,24.5055036505241,
24.692610599949,24.8801487839735,24.9413573829628,25.128895431322,25.3160398732771,
25.5031579457749,25.6902648951611,25.8778030791379,25.9390116782813,26.1636929039991,
26.2469320713865),.UNSPECIFIED.);
#256=B_SPLINE_CURVE_WITH_KNOTS('',3,(#23096,#23097,#23098,#23099,#23100,
#23101,#23102,#23103,#23104,#23105),.UNSPECIFIED.,.F.,.F.,(4,1,1,1,1,1,
1,4),(26.2469322667482,26.9366659735998,27.9343202689183,28.9319745642368,
29.9296288595553,30.9272831548739,31.9249374501924,32.5301175739278),
 .UNSPECIFIED.);
#257=B_SPLINE_CURVE_WITH_KNOTS('',3,(#23107,#23108,#23109,#23110,#23111,
#23112,#23113,#23114,#23115,#23116),.UNSPECIFIED.,.F.,.F.,(4,1,1,1,1,1,
1,4),(32.5301175739278,32.9225917455109,33.9202460408294,34.9179003361479,
35.9155546314664,36.9132089267849,37.9108632221034,38.8132941166151),
 .UNSPECIFIED.);
#258=B_SPLINE_CURVE_WITH_KNOTS('',3,(#23118,#23119,#23120,#23121,#23122,
#23123,#23124,#23125,#23126,#23127,#23128,#23129,#23130,#23131,#23132,#23133,
#23134,#23135,#23136,#23137,#23138,#23139,#23140,#23141,#23142,#23143,#23144,
#23145,#23146,#23147,#23148,#23149,#23150,#23151,#23152,#23153,#23154,#23155,
#23156,#23157,#23158,#23159,#23160,#23161,#23162,#23163,#23164,#23165,#23166,
#23167,#23168,#23169,#23170,#23171,#23172,#23173,#23174,#23175,#23176,#23177,
#23178,#23179,#23180,#23181,#23182,#23183,#23184,#23185,#23186,#23187,#23188,
#23189,#23190,#23191,#23192,#23193,#23194,#23195,#23196,#23197,#23198,#23199,
#23200,#23201,#23202,#23203,#23204,#23205,#23206,#23207,#23208,#23209,#23210,
#23211,#23212,#23213,#23214,#23215,#23216,#23217,#23218,#23219,#23220,#23221,
#23222,#23223,#23224,#23225,#23226,#23227,#23228,#23229,#23230,#23231,#23232),
 .UNSPECIFIED.,.F.,.F.,(4,3,3,3,3,3,3,3,3,3,3,3,3,3,3,3,3,3,3,3,3,3,3,3,
3,3,3,3,3,3,3,3,3,3,3,3,3,3,4),(38.8133028811074,38.908517517422,39.0960555660062,
39.2832000081941,39.4703180809318,39.6574250305625,39.8449632147861,39.9061718127405,
40.0937098613254,40.2808543035139,40.4679723762523,40.6550793258838,40.8426175101081,
40.903826108059,41.0913641566439,41.2785085988324,41.4656266715708,41.6527336212022,
41.8402718054265,41.9014804033775,42.0890184519623,42.2761628941507,42.4632809668889,
42.6503879165202,42.8379261007444,42.899134698696,43.0866727472808,43.2738171894693,
43.4609352622076,43.648042211839,43.8355803960632,43.8967889940145,44.0843270425993,
44.2714714847877,44.4585895575261,44.6456965071574,44.8332346913816,44.894443289333,
45.096488188287),.UNSPECIFIED.);
#259=B_SPLINE_CURVE_WITH_KNOTS('',3,(#23234,#23235,#23236,#23237,#23238,
#23239,#23240,#23241,#23242,#23243),.UNSPECIFIED.,.F.,.F.,(4,1,1,1,1,1,
1,4),(45.0964910901625,45.8920975846515,46.8897518799701,47.8874061752886,
48.8850604706071,49.8827147659256,50.8803690612441,51.3796734954666),
 .UNSPECIFIED.);
#260=B_SPLINE_CURVE_WITH_KNOTS('',3,(#23245,#23246,#23247,#23248,#23249,
#23250,#23251,#23252,#23253,#23254),.UNSPECIFIED.,.F.,.F.,(4,1,1,1,1,1,
1,4),(51.3796734954666,51.8780233565626,52.8756776518811,53.8733319471996,
54.8709862425181,55.8686405378366,56.8662948331552,57.6628558111006),
 .UNSPECIFIED.);
#261=B_SPLINE_CURVE_WITH_KNOTS('',3,(#23256,#23257,#23258,#23259,#23260,
#23261,#23262,#23263,#23264,#23265,#23266,#23267,#23268,#23269,#23270,#23271,
#23272,#23273,#23274,#23275,#23276,#23277,#23278,#23279,#23280,#23281,#23282,
#23283,#23284,#23285,#23286,#23287,#23288,#23289,#23290,#23291,#23292,#23293,
#23294,#23295,#23296,#23297,#23298,#23299,#23300,#23301,#23302,#23303,#23304,
#23305,#23306,#23307,#23308,#23309,#23310,#23311,#23312,#23313,#23314,#23315,
#23316,#23317,#23318,#23319,#23320,#23321,#23322,#23323,#23324,#23325,#23326,
#23327,#23328,#23329,#23330,#23331,#23332,#23333,#23334,#23335,#23336,#23337,
#23338,#23339,#23340,#23341,#23342,#23343,#23344,#23345,#23346,#23347,#23348,
#23349,#23350,#23351,#23352,#23353,#23354,#23355,#23356,#23357,#23358,#23359,
#23360,#23361,#23362,#23363,#23364,#23365,#23366,#23367,#23368,#23369,#23370),
 .UNSPECIFIED.,.F.,.F.,(4,3,3,3,3,3,3,3,3,3,3,3,3,3,3,3,3,3,3,3,3,3,3,3,
3,3,3,3,3,3,3,3,3,3,3,3,3,3,4),(57.6628588026462,57.8639491284737,58.0514871770584,
58.2386316192467,58.4257496919849,58.6128566416161,58.8003948258402,58.8616034237922,
59.049141472377,59.2362859145655,59.4234039873038,59.6105109369352,59.7980491211594,
59.8592577191107,60.0467957676955,60.233940209884,60.4210582826223,60.6081652322537,
60.7957034164779,60.8569120144292,61.044450063014,61.2315945052024,61.4187125779407,
61.6058195275721,61.7933577117963,61.8545663097477,62.0421043583325,62.229248800521,
62.4163668732593,62.6034738228906,62.7910120071149,62.8522206050662,63.039758653651,
63.2269030958394,63.4140211685777,63.601128118209,63.7886663024333,63.8498749003847,
63.9460441098258),.UNSPECIFIED.);
#262=B_SPLINE_CURVE_WITH_KNOTS('',3,(#23372,#23373,#23374,#23375,#23376,
#23377,#23378,#23379,#23380,#23381),.UNSPECIFIED.,.F.,.F.,(4,1,1,1,1,1,
1,4),(63.9460528873255,64.8475291957032,65.8451834910218,66.8428377863403,
67.8404920816588,68.8381463769773,69.8358006722958,70.2292294170054),
 .UNSPECIFIED.);
#263=B_SPLINE_CURVE_WITH_KNOTS('',3,(#23383,#23384,#23385,#23386,#23387,
#23388,#23389,#23390,#23391,#23392),.UNSPECIFIED.,.F.,.F.,(4,1,1,1,1,1,
1,4),(70.2292294170054,70.8334549676143,71.8311092629328,72.8287635582514,
73.8264178535699,74.8240721488884,75.8217264442069,76.512414724185),
 .UNSPECIFIED.);
#264=B_SPLINE_CURVE_WITH_KNOTS('',3,(#23394,#23395,#23396,#23397,#23398,
#23399,#23400,#23401,#23402,#23403,#23404,#23405,#23406,#23407,#23408,#23409,
#23410,#23411,#23412,#23413,#23414,#23415,#23416,#23417,#23418,#23419,#23420,
#23421,#23422,#23423,#23424,#23425,#23426,#23427,#23428,#23429,#23430,#23431,
#23432,#23433,#23434,#23435,#23436,#23437,#23438,#23439,#23440,#23441,#23442,
#23443,#23444,#23445,#23446,#23447,#23448,#23449,#23450,#23451,#23452,#23453,
#23454,#23455,#23456,#23457,#23458,#23459,#23460,#23461,#23462,#23463,#23464,
#23465,#23466,#23467,#23468,#23469,#23470,#23471,#23472,#23473,#23474,#23475,
#23476,#23477,#23478,#23479,#23480,#23481,#23482,#23483,#23484,#23485,#23486,
#23487,#23488,#23489,#23490,#23491,#23492,#23493,#23494,#23495,#23496,#23497,
#23498,#23499,#23500,#23501,#23502,#23503,#23504,#23505,#23506,#23507,#23508),
 .UNSPECIFIED.,.F.,.F.,(4,3,3,3,3,3,3,3,3,3,3,3,3,3,3,3,3,3,3,3,3,3,3,3,
3,3,3,3,3,3,3,3,3,3,3,3,3,3,4),(76.5124149178937,76.737332646363,76.8193807395254,
77.0069187881103,77.1940632302988,77.3811813030371,77.5682882526685,77.7558264368928,
77.8170350348439,78.0045730834287,78.1917175256171,78.3788355983554,78.5659425479868,
78.753480732211,78.8146893301624,79.0022273787472,79.1893718209356,79.3764898936739,
79.5635968433053,79.7511350275295,79.8123436254809,79.9998816740657,80.1870261162542,
80.3741441889925,80.5612511386239,80.7487893228481,80.8099979207994,80.9975359693842,
81.1846804115726,81.3717984843109,81.5589054339422,81.7464436181664,81.8076522161179,
81.994870137769,82.1816952728114,82.368494414651,82.5552860710844,82.7425043086765,
82.7956000313646),.UNSPECIFIED.);
#265=B_SPLINE_CURVE_WITH_KNOTS('',3,(#23510,#23511,#23512,#23513,#23514,
#23515,#23516,#23517,#23518,#23519,#23520,#23521),.UNSPECIFIED.,.F.,.F.,
(4,2,1,1,1,1,1,1,4),(82.7956000313646,82.8053065114364,83.802960806755,
84.8006151020735,85.798269397392,86.7959236927105,87.793577988029,88.7912322833475,
89.0787853385442),.UNSPECIFIED.);
#266=B_SPLINE_CURVE_WITH_KNOTS('',3,(#23523,#23524,#23525,#23526,#23527,
#23528,#23529,#23530,#23531,#23532),.UNSPECIFIED.,.F.,.F.,(4,1,1,1,1,1,
1,4),(89.0787853385442,89.7888865786661,90.7865408739846,91.7841951693031,
92.7818494646216,93.7795037599401,94.7771580552586,95.3619706457238),
 .UNSPECIFIED.);
#267=B_SPLINE_CURVE_WITH_KNOTS('',3,(#23534,#23535,#23536,#23537,#23538,
#23539,#23540,#23541,#23542,#23543,#23544,#23545,#23546,#23547,#23548,#23549,
#23550,#23551,#23552,#23553,#23554,#23555,#23556,#23557,#23558,#23559,#23560,
#23561,#23562,#23563,#23564,#23565,#23566,#23567,#23568,#23569,#23570,#23571,
#23572,#23573,#23574,#23575,#23576,#23577,#23578,#23579,#23580,#23581,#23582,
#23583,#23584,#23585,#23586,#23587,#23588,#23589,#23590,#23591,#23592,#23593,
#23594,#23595,#23596,#23597,#23598,#23599,#23600,#23601,#23602,#23603,#23604,
#23605,#23606,#23607,#23608,#23609,#23610,#23611,#23612,#23613,#23614,#23615,
#23616,#23617,#23618,#23619,#23620,#23621,#23622,#23623,#23624,#23625,#23626,
#23627,#23628,#23629,#23630,#23631,#23632,#23633,#23634,#23635,#23636,#23637,
#23638,#23639,#23640,#23641,#23642,#23643,#23644,#23645),.UNSPECIFIED.,
 .F.,.F.,(4,3,3,3,3,3,3,3,3,3,3,3,3,3,3,3,3,3,3,3,3,3,3,3,3,3,3,3,3,3,3,
3,3,3,3,3,3,4),(95.3619710488281,95.5683916997026,95.7748123505771,95.9623503991619,
96.1494948413504,96.3366129140888,96.5237198637202,96.7112580479445,96.7724666458956,
96.9600046944804,97.1471491366689,97.3342672094072,97.5213741590385,97.7089123432627,
97.7701209412141,97.9576589897989,98.1448034319873,98.3319215047256,98.5190284543569,
98.7065666385811,98.7677752365326,98.9553132851174,99.1424577273058,99.3295758000441,
99.5166827496755,99.7042209338997,99.7654295318512,99.9529675804363,100.140112022625,
100.327230095364,100.514337044995,100.70187522922,100.76308382717,100.94809698056,
101.13284606384,101.317418303564,101.502339127779,101.645155952903),
 .UNSPECIFIED.);
#268=B_SPLINE_CURVE_WITH_KNOTS('',3,(#23647,#23648,#23649,#23650,#23651,
#23652,#23653,#23654,#23655,#23656,#23657),.UNSPECIFIED.,.F.,.F.,(4,1,1,
1,1,1,1,1,4),(101.645155952903,101.760738122488,102.758392417807,103.756046713125,
104.753701008444,105.751355303762,106.749009599081,107.746663894399,107.928341260083),
 .UNSPECIFIED.);
#269=B_SPLINE_CURVE_WITH_KNOTS('',3,(#23659,#23660,#23661,#23662,#23663,
#23664,#23665,#23666,#23667,#23668),.UNSPECIFIED.,.F.,.F.,(4,1,1,1,1,1,
1,4),(107.928341260083,108.744318189718,109.741972485036,110.739626780355,
111.737281075673,112.734935370992,113.73258966631,114.211525038399),
 .UNSPECIFIED.);
#270=B_SPLINE_CURVE_WITH_KNOTS('',3,(#23670,#23671,#23672,#23673,#23674,
#23675,#23676,#23677,#23678,#23679,#23680,#23681,#23682,#23683,#23684,#23685,
#23686,#23687,#23688,#23689,#23690,#23691,#23692,#23693,#23694,#23695,#23696,
#23697,#23698,#23699,#23700,#23701,#23702,#23703,#23704,#23705,#23706,#23707,
#23708,#23709,#23710,#23711,#23712,#23713,#23714,#23715,#23716,#23717,#23718,
#23719,#23720,#23721,#23722,#23723,#23724,#23725,#23726,#23727,#23728,#23729,
#23730,#23731,#23732,#23733,#23734,#23735,#23736,#23737,#23738,#23739,#23740,
#23741,#23742,#23743,#23744,#23745,#23746,#23747,#23748,#23749,#23750,#23751,
#23752,#23753,#23754,#23755,#23756,#23757,#23758,#23759,#23760,#23761,#23762,
#23763,#23764,#23765,#23766,#23767,#23768,#23769,#23770,#23771,#23772,#23773,
#23774,#23775,#23776,#23777,#23778,#23779,#23780,#23781,#23782,#23783,#23784),
 .UNSPECIFIED.,.F.,.F.,(4,3,3,3,3,3,3,3,3,3,3,3,3,3,3,3,3,3,3,3,3,3,3,3,
3,3,3,3,3,3,3,3,3,3,3,3,3,3,4),(114.211526567263,114.406050577366,114.601390959919,
114.730243961629,114.917782010213,115.104926452402,115.29204452514,115.479151474771,
115.666689658995,115.727898256947,115.915436305532,116.102580747721,116.28969882046,
116.476805770092,116.664343954316,116.725552552266,116.913090600851,117.100235043039,
117.287353115777,117.474460065408,117.661998249632,117.723206847584,117.910744896169,
118.097889338357,118.285007411096,118.472114360727,118.659652544952,118.720861142903,
118.908399191488,119.095543633676,119.282661706415,119.469768656046,119.65730684027,
119.718515438221,119.912564547276,120.097240508108,120.2817442013,120.466424250738,
120.494711874442),.UNSPECIFIED.);
#271=B_SPLINE_CURVE_WITH_KNOTS('',3,(#23786,#23787,#23788,#23789,#23790,
#23791,#23792,#23793,#23794,#23795,#23796),.UNSPECIFIED.,.F.,.F.,(4,1,1,
1,1,1,1,1,4),(120.494711874442,120.71616973354,121.713824028858,122.711478324177,
123.709132619495,124.706786914814,125.704441210132,126.702095505451,126.777897181622),
 .UNSPECIFIED.);
#272=B_SPLINE_CURVE_WITH_KNOTS('',3,(#23798,#23799,#23800,#23801,#23802,
#23803,#23804,#23805,#23806,#23807),.UNSPECIFIED.,.F.,.F.,(4,1,1,1,1,1,
1,4),(126.777897181622,127.699749800769,128.697404096088,129.695058391406,
130.692712686725,131.690366982044,132.688021277362,133.061074978669),
 .UNSPECIFIED.);
#273=B_SPLINE_CURVE_WITH_KNOTS('',3,(#23809,#23810,#23811,#23812,#23813,
#23814,#23815,#23816,#23817,#23818,#23819,#23820,#23821,#23822,#23823,#23824,
#23825,#23826,#23827,#23828,#23829,#23830,#23831,#23832,#23833,#23834,#23835,
#23836,#23837,#23838,#23839,#23840,#23841,#23842,#23843,#23844,#23845,#23846,
#23847,#23848,#23849,#23850,#23851,#23852,#23853,#23854,#23855,#23856,#23857,
#23858,#23859,#23860,#23861,#23862,#23863,#23864,#23865,#23866,#23867,#23868,
#23869,#23870,#23871,#23872,#23873,#23874,#23875,#23876,#23877,#23878,#23879,
#23880,#23881,#23882,#23883,#23884,#23885,#23886,#23887,#23888,#23889,#23890,
#23891,#23892,#23893,#23894,#23895,#23896,#23897,#23898,#23899,#23900,#23901,
#23902,#23903,#23904,#23905,#23906,#23907,#23908,#23909,#23910,#23911,#23912,
#23913,#23914,#23915,#23916,#23917,#23918,#23919,#23920,#23921,#23922,#23923),
 .UNSPECIFIED.,.F.,.F.,(4,3,3,3,3,3,3,3,3,3,3,3,3,3,3,3,3,3,3,3,3,3,3,3,
3,3,3,3,3,3,3,3,3,3,3,3,3,3,4),(133.061082488801,133.249569004459,133.4381076651,
133.627144886932,133.685675572681,133.873213621265,134.060358063453,134.24747613619,
134.434583085821,134.622121270044,134.683329867999,134.870867916584,135.058012358773,
135.245130431511,135.432237381143,135.619775565367,135.680984163318,135.868522211903,
136.055666654091,136.242784726829,136.429891676461,136.617429860685,136.678638458636,
136.866176507221,137.053320949409,137.240439022148,137.427545971779,137.615084156004,
137.676292753955,137.86383080254,138.050975244728,138.238093317467,138.425200267098,
138.612738451322,138.673947049273,138.861220080197,139.048088728297,139.234874348461,
139.344267795981),.UNSPECIFIED.);
#274=B_SPLINE_CURVE_WITH_KNOTS('',3,(#23925,#23926,#23927,#23928,#23929,
#23930,#23931,#23932,#23933,#23934),.UNSPECIFIED.,.F.,.F.,(4,1,1,1,1,1,
1,4),(139.344274773769,139.671601344592,140.66925563991,141.666909935229,
142.664564230547,143.662218525866,144.659872821184,145.62745310316),
 .UNSPECIFIED.);
#275=B_SPLINE_CURVE_WITH_KNOTS('',3,(#23936,#23937,#23938,#23939,#23940,
#23941,#23942,#23943,#23944,#23945,#23946,#23947),.UNSPECIFIED.,.F.,.F.,
(4,2,1,1,1,1,1,1,4),(145.62745310316,145.657527116503,146.655181411821,
147.65283570714,148.650490002458,149.648144297777,150.645798593095,151.643452888414,
151.910635273349),.UNSPECIFIED.);
#276=B_SPLINE_CURVE_WITH_KNOTS('',3,(#23949,#23950,#23951,#23952,#23953,
#23954,#23955,#23956,#23957,#23958,#23959,#23960,#23961,#23962,#23963,#23964,
#23965,#23966,#23967,#23968,#23969,#23970,#23971,#23972,#23973,#23974,#23975,
#23976,#23977,#23978,#23979,#23980,#23981,#23982,#23983,#23984,#23985,#23986,
#23987,#23988,#23989,#23990,#23991,#23992,#23993,#23994,#23995,#23996,#23997,
#23998,#23999,#24000,#24001,#24002,#24003,#24004,#24005,#24006,#24007,#24008,
#24009,#24010,#24011,#24012,#24013,#24014,#24015,#24016,#24017,#24018,#24019,
#24020,#24021,#24022,#24023,#24024,#24025,#24026,#24027,#24028,#24029,#24030,
#24031,#24032,#24033,#24034,#24035,#24036,#24037,#24038,#24039,#24040,#24041,
#24042,#24043,#24044,#24045,#24046,#24047,#24048,#24049,#24050,#24051,#24052,
#24053,#24054,#24055,#24056,#24057,#24058,#24059,#24060),.UNSPECIFIED.,
 .F.,.F.,(4,3,3,3,3,3,3,3,3,3,3,3,3,3,3,3,3,3,3,3,3,3,3,3,3,3,3,3,3,3,3,
3,3,3,3,3,3,4),(151.91063841034,152.096050504932,152.281317851542,152.467037581743,
152.641107183732,152.828645232317,153.015789674506,153.202907747245,153.390014696877,
153.577552881102,153.638761479051,153.826299527635,154.013443969824,154.200562042562,
154.387668992193,154.575207176417,154.636415774369,154.823953822954,155.011098265143,
155.198216337881,155.385323287513,155.572861471737,155.634070069688,155.821608118273,
156.008752560461,156.195870633199,156.382977582831,156.570515767055,156.631724365006,
156.819262413591,157.006406855779,157.193524928517,157.380631878149,157.568170062373,
157.629378660325,157.821576221357,158.01326351236,158.19382371752),
 .UNSPECIFIED.);
#277=B_SPLINE_CURVE_WITH_KNOTS('',3,(#24062,#24063,#24064,#24065,#24066,
#24067,#24068,#24069,#24070,#24071),.UNSPECIFIED.,.F.,.F.,(4,1,1,1,1,1,
1,4),(158.193828690622,158.627032955643,159.624687250962,160.62234154628,
161.619995841599,162.617650136917,163.615304432236,164.477009024699),
 .UNSPECIFIED.);
#278=B_SPLINE_CURVE_WITH_KNOTS('',3,(#24073,#24074,#24075,#24076,#24077,
#24078,#24079,#24080,#24081,#24082,#24083),.UNSPECIFIED.,.F.,.F.,(4,1,1,
1,1,1,1,1,4),(164.477009024699,164.612958727554,165.610613022873,166.608267318191,
167.60592161351,168.603575908828,169.601230204147,170.598884499465,170.760194331879),
 .UNSPECIFIED.);
#279=B_SPLINE_CURVE_WITH_KNOTS('',3,(#24085,#24086,#24087,#24088,#24089,
#24090,#24091,#24092,#24093,#24094,#24095,#24096,#24097,#24098,#24099,#24100,
#24101,#24102,#24103,#24104,#24105,#24106,#24107,#24108,#24109,#24110,#24111,
#24112,#24113,#24114,#24115,#24116,#24117,#24118,#24119,#24120,#24121,#24122,
#24123,#24124,#24125,#24126,#24127,#24128,#24129,#24130,#24131,#24132,#24133,
#24134,#24135,#24136,#24137,#24138,#24139,#24140,#24141,#24142,#24143,#24144,
#24145,#24146,#24147,#24148,#24149,#24150,#24151,#24152,#24153,#24154,#24155,
#24156,#24157,#24158,#24159,#24160,#24161,#24162,#24163,#24164,#24165,#24166,
#24167,#24168,#24169,#24170,#24171,#24172,#24173,#24174,#24175,#24176,#24177,
#24178,#24179,#24180,#24181,#24182,#24183,#24184,#24185,#24186,#24187,#24188,
#24189,#24190,#24191,#24192,#24193,#24194,#24195,#24196,#24197,#24198,#24199),
 .UNSPECIFIED.,.F.,.F.,(4,3,3,3,3,3,3,3,3,3,3,3,3,3,3,3,3,3,3,3,3,3,3,3,
3,3,3,3,3,3,3,3,3,3,3,3,3,3,4),(170.760194331879,170.944734727437,171.129147203637,
171.313475752256,171.498218708515,171.596538794784,171.784076843369,171.971221285557,
172.158339358295,172.345446307926,172.53298449215,172.594193090102,172.781731138687,
172.968875580876,173.155993653614,173.343100603245,173.53063878747,173.591847385421,
173.779385434006,173.966529876195,174.153647948934,174.340754898566,174.528293082791,
174.58950168074,174.777039729324,174.964184171512,175.15130224425,175.338409193881,
175.525947378105,175.587155976058,175.774694024643,175.961838466832,176.14895653957,
176.336063489202,176.523601673426,176.584810271377,176.785743470653,176.985583319409,
177.04337942508),.UNSPECIFIED.);
#280=B_SPLINE_CURVE_WITH_KNOTS('',3,(#24201,#24202,#24203,#24204,#24205,
#24206,#24207,#24208,#24209,#24210),.UNSPECIFIED.,.F.,.F.,(4,1,1,1,1,1,
1,4),(177.043379639058,177.582464566695,178.580118862014,179.577773157332,
180.575427452651,181.573081747969,182.570736043288,183.326564946238),
 .UNSPECIFIED.);
#281=B_SPLINE_CURVE_WITH_KNOTS('',3,(#24212,#24213,#24214,#24215,#24216,
#24217,#24218,#24219,#24220,#24221,#24222),.UNSPECIFIED.,.F.,.F.,(4,1,1,
1,1,1,1,1,4),(183.326564946238,183.568390338606,184.566044633925,185.563698929243,
186.561353224562,187.55900751988,188.556661815199,189.554316110517,189.609750253417),
 .UNSPECIFIED.);
#282=B_SPLINE_CURVE_WITH_KNOTS('',3,(#24224,#24225,#24226,#24227,#24228,
#24229,#24230,#24231,#24232,#24233,#24234,#24235,#24236,#24237,#24238,#24239,
#24240,#24241,#24242,#24243,#24244,#24245,#24246,#24247,#24248,#24249,#24250,
#24251,#24252,#24253,#24254,#24255,#24256,#24257,#24258,#24259,#24260,#24261,
#24262,#24263,#24264,#24265,#24266,#24267,#24268,#24269,#24270,#24271,#24272,
#24273,#24274,#24275,#24276,#24277,#24278,#24279,#24280,#24281,#24282,#24283,
#24284,#24285,#24286,#24287,#24288,#24289,#24290,#24291,#24292,#24293,#24294,
#24295,#24296,#24297,#24298,#24299,#24300,#24301,#24302,#24303,#24304,#24305,
#24306,#24307,#24308,#24309,#24310,#24311,#24312,#24313,#24314,#24315,#24316,
#24317,#24318,#24319,#24320,#24321,#24322,#24323,#24324,#24325,#24326,#24327,
#24328,#24329,#24330,#24331,#24332,#24333,#24334,#24335),.UNSPECIFIED.,
 .F.,.F.,(4,3,3,3,3,3,3,3,3,3,3,3,3,3,3,3,3,3,3,3,3,3,3,3,3,3,3,3,3,3,3,
3,3,3,3,3,3,4),(189.609750253417,189.795701084287,189.984768414674,190.1703338432,
190.361152124518,190.551970405836,190.739508454616,190.926652897001,191.113770969932,
191.300877919756,191.488416104167,191.549624701154,191.737162749492,191.924307191435,
192.111425263935,192.298532213331,192.48607039733,192.547278996473,192.734817044858,
192.921961486842,193.109079559371,193.29618650879,193.483724692802,193.544933291791,
193.732471341682,193.919615785181,194.106733859215,194.293840810136,194.481378995615,
194.54258758711,194.730125633722,194.917270073948,195.10438814477,195.291495092509,
195.479033274912,195.540241882428,195.755377132594,195.892935318778),
 .UNSPECIFIED.);
#283=B_SPLINE_CURVE_WITH_KNOTS('',3,(#24337,#24338,#24339,#24340,#24341,
#24342,#24343,#24344,#24345,#24346),.UNSPECIFIED.,.F.,.F.,(4,1,1,1,1,1,
1,4),(195.892935560597,196.537896177747,197.535550473065,198.533204768384,
199.530859063702,200.528513359021,201.526167654339,202.176120867777),
 .UNSPECIFIED.);
#284=B_SPLINE_CURVE_WITH_KNOTS('',3,(#24348,#24349,#24350,#24351,#24352,
#24353,#24354,#24355,#24356,#24357,#24358,#24359,#24360,#24361,#24362,#24363,
#24364,#24365,#24366,#24367,#24368,#24369,#24370,#24371,#24372,#24373,#24374,
#24375,#24376,#24377,#24378,#24379,#24380,#24381,#24382,#24383,#24384,#24385,
#24386,#24387,#24388,#24389,#24390,#24391,#24392,#24393,#24394,#24395,#24396,
#24397,#24398,#24399,#24400,#24401,#24402,#24403,#24404,#24405,#24406,#24407,
#24408,#24409,#24410,#24411,#24412,#24413,#24414,#24415,#24416,#24417,#24418,
#24419,#24420,#24421,#24422,#24423,#24424,#24425,#24426,#24427,#24428,#24429,
#24430,#24431,#24432,#24433,#24434,#24435,#24436,#24437,#24438,#24439,#24440,
#24441,#24442,#24443,#24444,#24445,#24446,#24447,#24448,#24449,#24450,#24451,
#24452,#24453,#24454,#24455,#24456,#24457,#24458,#24459),.UNSPECIFIED.,
 .F.,.F.,(4,3,3,3,3,3,3,3,3,3,3,3,3,3,3,3,3,3,3,3,3,3,3,3,3,3,3,3,3,3,3,
3,3,3,3,3,3,4),(202.176121107729,202.392189019061,202.523821949658,202.711360327859,
202.898505102102,203.085623505374,203.272730785002,203.460269292354,203.521476244976,
203.709013475378,203.896157100508,204.083274370061,204.270380523695,204.457917936997,
204.519130540295,204.70666908409,204.893814010344,205.080932544026,205.268039941717,
205.455578547114,205.516784835613,205.704324823687,205.891471224293,206.078591252941,
206.26570015905,206.45324026446,206.514439130932,206.701971386111,206.889110036183,
207.07622240564,207.263323697418,207.450856393847,207.51209342625,207.698196269153,
207.888473745604,208.074153943652,208.266730059304,208.459306174956),
 .UNSPECIFIED.);
#285=B_SPLINE_CURVE_WITH_KNOTS('',3,(#24461,#24462,#24463,#24464,#24465,
#24466,#24467,#24468,#24469,#24470,#24471),.UNSPECIFIED.,.F.,.F.,(4,1,1,
1,1,1,1,1,4),(208.459306174956,208.509747721569,209.507402016887,210.505056312206,
211.502710607524,212.500364902843,213.498019198161,214.49567349348,214.742490275424),
 .UNSPECIFIED.);
#286=B_SPLINE_CURVE_WITH_KNOTS('',3,(#24473,#24474,#24475,#24476,#24477,
#24478,#24479,#24480,#24481,#24482,#24483,#24484,#24485),.UNSPECIFIED.,
 .F.,.F.,(4,3,3,3,4),(214.742491482136,214.924334961889,215.106007171726,
215.288050992593,215.423492510042),.UNSPECIFIED.);
#287=B_SPLINE_CURVE_WITH_KNOTS('',3,(#24489,#24490,#24491,#24492,#24493,
#24494,#24495,#24496,#24497,#24498),.UNSPECIFIED.,.F.,.F.,(4,1,1,1,1,1,
1,4),(-217.488636379435,-216.490982084117,-215.493327788798,-214.49567349348,
-213.498019198161,-212.500364902843,-211.502710607524,-211.437656885764),
 .UNSPECIFIED.);
#288=B_SPLINE_CURVE_WITH_KNOTS('',3,(#24500,#24501,#24502,#24503,#24504,
#24505,#24506,#24507,#24508,#24509,#24510,#24511,#24512,#24513,#24514,#24515,
#24516,#24517,#24518,#24519,#24520,#24521,#24522,#24523,#24524,#24525,#24526,
#24527,#24528,#24529,#24530,#24531,#24532,#24533,#24534,#24535,#24536,#24537,
#24538,#24539,#24540,#24541,#24542,#24543,#24544,#24545,#24546,#24547,#24548,
#24549,#24550,#24551,#24552,#24553,#24554,#24555,#24556,#24557,#24558,#24559,
#24560,#24561,#24562,#24563,#24564,#24565,#24566,#24567,#24568,#24569,#24570,
#24571,#24572,#24573,#24574,#24575,#24576,#24577,#24578,#24579,#24580,#24581,
#24582,#24583,#24584,#24585,#24586,#24587,#24588,#24589,#24590,#24591,#24592,
#24593,#24594,#24595,#24596,#24597,#24598,#24599,#24600,#24601,#24602,#24603,
#24604,#24605,#24606,#24607,#24608,#24609,#24610,#24611),.UNSPECIFIED.,
 .F.,.F.,(4,3,3,3,3,3,3,3,3,3,3,3,3,3,3,3,3,3,3,3,3,3,3,3,3,3,3,3,3,3,3,
3,3,3,3,3,3,4),(-211.437656885764,-211.251875774012,-211.065170908561,-210.879760937552,
-210.692408624879,-210.505056312206,-210.317556428218,-210.130451044026,
-209.9433727371,-209.756306005462,-209.568807969712,-209.507402016887,-209.319853122717,
-209.13269771433,-208.945568669285,-208.758450732574,-208.570901743242,
-208.509747721569,-208.322205304621,-208.135056315231,-207.947933502637,
-207.760821696469,-207.573278571308,-207.51209342625,-207.324560864371,
-207.137422044073,-206.950309704675,-206.763208558969,-206.575676176528,
-206.514439130932,-206.326899161105,-206.139752769977,-205.952632737958,
-205.765523821033,-205.577983694059,-205.516784835613,-205.303371487571,
-205.154471579052),.UNSPECIFIED.);
#289=B_SPLINE_CURVE_WITH_KNOTS('',3,(#24613,#24614,#24615,#24616,#24617,
#24618,#24619,#24620,#24621,#24622,#24623,#24624,#24625,#24626,#24627,#24628,
#24629,#24630,#24631,#24632,#24633,#24634,#24635,#24636,#24637,#24638,#24639,
#24640,#24641,#24642,#24643,#24644,#24645,#24646,#24647,#24648,#24649,#24650,
#24651,#24652,#24653,#24654,#24655,#24656,#24657,#24658,#24659,#24660,#24661,
#24662,#24663,#24664,#24665,#24666,#24667,#24668,#24669,#24670,#24671,#24672,
#24673,#24674,#24675,#24676,#24677,#24678,#24679,#24680,#24681,#24682,#24683,
#24684,#24685,#24686,#24687,#24688,#24689,#24690,#24691,#24692,#24693,#24694,
#24695,#24696,#24697,#24698,#24699,#24700,#24701,#24702,#24703,#24704,#24705,
#24706,#24707,#24708,#24709,#24710,#24711,#24712,#24713,#24714,#24715,#24716,
#24717,#24718,#24719,#24720,#24721,#24722,#24723,#24724,#24725,#24726,#24727),
 .UNSPECIFIED.,.F.,.F.,(4,3,3,3,3,3,3,3,3,3,3,3,3,3,3,3,3,3,3,3,3,3,3,3,
3,3,3,3,3,3,3,3,3,3,3,3,3,3,4),(-205.154471578585,-204.966416462605,-204.778333592112,
-204.589761204189,-204.519130540295,-204.331593262598,-204.144449611253,
-203.957332346419,-203.770226215423,-203.582688850692,-203.521476244976,
-203.33393787321,-203.146793102426,-202.95967469825,-202.77256741519,-202.585028900752,
-202.523821949658,-202.336283872299,-202.149139398908,-201.962021291873,
-201.774914306113,-201.587376083692,-201.526167654339,-201.338629711466,
-201.15148537787,-200.964367416273,-200.777260579377,-200.58972250818,-200.528513359021,
-200.340975258119,-200.153830762642,-199.966712636016,-199.779605632095,
-199.592067393986,-199.530859063702,-199.343221598296,-199.155994350822,
-198.968876899421,-198.871286271405),.UNSPECIFIED.);
#290=B_SPLINE_CURVE_WITH_KNOTS('',3,(#24729,#24730,#24731,#24732,#24733,
#24734,#24735,#24736,#24737,#24738),.UNSPECIFIED.,.F.,.F.,(4,1,1,1,1,1,
1,4),(-198.871278975199,-198.533204768384,-197.535550473065,-196.537896177747,
-195.540241882428,-194.54258758711,-193.544933291791,-192.588106266864),
 .UNSPECIFIED.);
#291=B_SPLINE_CURVE_WITH_KNOTS('',3,(#24740,#24741,#24742,#24743,#24744,
#24745,#24746,#24747,#24748,#24749,#24750,#24751,#24752,#24753,#24754,#24755,
#24756,#24757,#24758,#24759,#24760,#24761,#24762,#24763,#24764,#24765,#24766,
#24767,#24768,#24769,#24770,#24771,#24772,#24773,#24774,#24775,#24776,#24777,
#24778,#24779,#24780,#24781,#24782,#24783,#24784,#24785,#24786,#24787,#24788,
#24789,#24790,#24791,#24792,#24793,#24794,#24795,#24796,#24797,#24798,#24799,
#24800,#24801,#24802,#24803,#24804,#24805,#24806,#24807,#24808,#24809,#24810,
#24811,#24812,#24813,#24814,#24815,#24816,#24817,#24818,#24819,#24820,#24821,
#24822,#24823,#24824,#24825,#24826,#24827,#24828,#24829,#24830,#24831,#24832,
#24833,#24834,#24835,#24836,#24837,#24838,#24839,#24840,#24841,#24842,#24843,
#24844,#24845,#24846,#24847,#24848,#24849,#24850,#24851,#24852,#24853,#24854,
#24855,#24856,#24857),.UNSPECIFIED.,.F.,.F.,(4,3,3,3,3,3,3,3,3,3,3,3,3,
3,3,3,3,3,3,3,3,3,3,3,3,3,3,3,3,3,3,3,3,3,3,3,3,3,3,4),(-192.588100964226,
-192.547278996473,-192.359740948114,-192.172596506158,-191.985478433661,
-191.798371484274,-191.610833300298,-191.549624701154,-191.362086652382,
-191.174942210002,-190.987824137069,-190.800717187241,-190.613179002821,
-190.551970405836,-190.364432357295,-190.177287915152,-189.990169842458,
-189.803062892871,-189.61552470869,-189.554316110517,-189.366778061959,
-189.179633619798,-188.992515547088,-188.805408597486,-188.617870413291,
-188.556661815199,-188.369123766587,-188.18197932437,-187.994861251603,
-187.807754301943,-187.62021611769,-187.55900751988,-187.371469471304,-187.184325029124,
-186.997206956394,-186.810100006771,-186.622561822555,-186.561353224562,
-186.321110839942,-186.304915803035),.UNSPECIFIED.);
#292=B_SPLINE_CURVE_WITH_KNOTS('',3,(#24859,#24860,#24861,#24862,#24863,
#24864,#24865,#24866,#24867,#24868),.UNSPECIFIED.,.F.,.F.,(4,1,1,1,1,1,
1,4),(-186.304915657046,-185.563698929243,-184.566044633925,-183.568390338606,
-182.570736043288,-181.573081747969,-180.575427452651,-180.021730349867),
 .UNSPECIFIED.);
#293=B_SPLINE_CURVE_WITH_KNOTS('',3,(#24870,#24871,#24872,#24873,#24874,
#24875,#24876,#24877,#24878,#24879),.UNSPECIFIED.,.F.,.F.,(4,1,1,1,1,1,
1,4),(-180.021730349867,-179.577773157332,-178.580118862013,-177.582464566695,
-176.584810271376,-175.587155976058,-174.589501680739,-173.738552553459),
 .UNSPECIFIED.);
#294=B_SPLINE_CURVE_WITH_KNOTS('',3,(#24881,#24882,#24883,#24884,#24885,
#24886,#24887,#24888,#24889,#24890,#24891,#24892,#24893,#24894,#24895,#24896,
#24897,#24898,#24899,#24900,#24901,#24902,#24903,#24904,#24905,#24906,#24907,
#24908,#24909,#24910,#24911,#24912,#24913,#24914,#24915,#24916,#24917,#24918,
#24919,#24920,#24921,#24922,#24923,#24924,#24925,#24926,#24927,#24928,#24929,
#24930,#24931,#24932,#24933,#24934,#24935,#24936,#24937,#24938,#24939,#24940,
#24941,#24942,#24943,#24944,#24945,#24946,#24947,#24948,#24949,#24950,#24951,
#24952,#24953,#24954,#24955,#24956,#24957,#24958,#24959,#24960,#24961,#24962,
#24963,#24964,#24965,#24966,#24967,#24968,#24969,#24970,#24971,#24972,#24973,
#24974,#24975,#24976,#24977,#24978,#24979,#24980,#24981,#24982,#24983,#24984,
#24985,#24986,#24987,#24988,#24989,#24990,#24991,#24992,#24993,#24994,#24995),
 .UNSPECIFIED.,.F.,.F.,(4,3,3,3,3,3,3,3,3,3,3,3,3,3,3,3,3,3,3,3,3,3,3,3,
3,3,3,3,3,3,3,3,3,3,3,3,3,3,4),(-173.738545042687,-173.591847385421,-173.404309336835,
-173.217164894645,-173.030046821905,-172.842939872272,-172.655401688047,
-172.594193090102,-172.406655041518,-172.21951059933,-172.032392526592,
-171.845285576961,-171.657747392738,-171.596538794784,-171.409000746199,
-171.221856304011,-171.034738231272,-170.847631281641,-170.660093097417,
-170.598884499465,-170.41134645088,-170.224202008692,-170.037083935953,
-169.849976986322,-169.662438802098,-169.601230204147,-169.413692155562,
-169.226547713374,-169.039429640635,-168.852322691004,-168.66478450678,
-168.603575908828,-168.416037860243,-168.228893418054,-168.041775345316,
-167.854668395684,-167.66713021146,-167.60592161351,-167.455359735508),
 .UNSPECIFIED.);
#295=B_SPLINE_CURVE_WITH_KNOTS('',3,(#24997,#24998,#24999,#25000,#25001,
#25002,#25003,#25004,#25005,#25006),.UNSPECIFIED.,.F.,.F.,(4,1,1,1,1,1,
1,4),(-167.455352458497,-166.608267318191,-165.610613022873,-164.612958727554,
-163.615304432236,-162.617650136917,-161.619995841599,-161.172174428328),
 .UNSPECIFIED.);
#296=B_SPLINE_CURVE_WITH_KNOTS('',3,(#25008,#25009,#25010,#25011,#25012,
#25013,#25014,#25015,#25016,#25017),.UNSPECIFIED.,.F.,.F.,(4,1,1,1,1,1,
1,4),(-161.172174428328,-160.62234154628,-159.624687250962,-158.627032955643,
-157.629378660325,-156.631724365006,-155.634070069688,-154.888989121148),
 .UNSPECIFIED.);
#297=B_SPLINE_CURVE_WITH_KNOTS('',3,(#25019,#25020,#25021,#25022,#25023,
#25024,#25025,#25026,#25027,#25028,#25029,#25030,#25031,#25032,#25033,#25034,
#25035,#25036,#25037,#25038,#25039,#25040,#25041,#25042,#25043,#25044,#25045,
#25046,#25047,#25048,#25049,#25050,#25051,#25052,#25053,#25054,#25055,#25056,
#25057,#25058,#25059,#25060,#25061,#25062,#25063,#25064,#25065,#25066,#25067,
#25068,#25069,#25070,#25071,#25072,#25073,#25074,#25075,#25076,#25077,#25078,
#25079,#25080,#25081,#25082,#25083,#25084,#25085,#25086,#25087,#25088,#25089,
#25090,#25091,#25092,#25093,#25094,#25095,#25096,#25097,#25098,#25099,#25100,
#25101,#25102,#25103,#25104,#25105,#25106,#25107,#25108,#25109,#25110,#25111,
#25112,#25113,#25114,#25115,#25116,#25117,#25118,#25119,#25120,#25121,#25122,
#25123,#25124,#25125,#25126,#25127,#25128,#25129,#25130,#25131,#25132,#25133),
 .UNSPECIFIED.,.F.,.F.,(4,3,3,3,3,3,3,3,3,3,3,3,3,3,3,3,3,3,3,3,3,3,3,3,
3,3,3,3,3,3,3,3,3,3,3,3,3,3,4),(-154.88898899765,-154.636415774369,-154.448877725784,
-154.261733283596,-154.074615210858,-153.887508261227,-153.699970077003,
-153.638761479051,-153.451223430466,-153.264078988277,-153.076960915538,
-152.889853965907,-152.702315781682,-152.641107183732,-152.453569135147,
-152.266424692959,-152.079306620221,-151.89219967059,-151.704661486366,
-151.643452888414,-151.455914839829,-151.268770397641,-151.081652324902,
-150.894545375271,-150.707007191046,-150.645798593095,-150.45826054451,
-150.271116102322,-150.083998029584,-149.896891079952,-149.709352895728,
-149.648144297777,-149.460606249192,-149.273461807004,-149.086343734265,
-148.899236784634,-148.71169860041,-148.650490002458,-148.605803813969),
 .UNSPECIFIED.);
#298=B_SPLINE_CURVE_WITH_KNOTS('',3,(#25135,#25136,#25137,#25138,#25139,
#25140,#25141,#25142,#25143,#25144),.UNSPECIFIED.,.F.,.F.,(4,1,1,1,1,1,
1,4),(-148.605798125697,-147.65283570714,-146.655181411821,-145.657527116503,
-144.659872821184,-143.662218525866,-142.664564230547,-142.322618506789),
 .UNSPECIFIED.);
#299=B_SPLINE_CURVE_WITH_KNOTS('',3,(#25146,#25147,#25148,#25149,#25150,
#25151,#25152,#25153,#25154,#25155),.UNSPECIFIED.,.F.,.F.,(4,1,1,1,1,1,
1,4),(-142.322618506789,-141.666909935229,-140.66925563991,-139.671601344592,
-138.673947049273,-137.676292753955,-136.678638458636,-136.03943319961),
 .UNSPECIFIED.);
#300=B_SPLINE_CURVE_WITH_KNOTS('',3,(#25157,#25158,#25159,#25160,#25161,
#25162,#25163,#25164,#25165,#25166,#25167,#25168,#25169,#25170,#25171,#25172,
#25173,#25174,#25175,#25176,#25177,#25178,#25179,#25180,#25181,#25182,#25183,
#25184,#25185,#25186,#25187,#25188,#25189,#25190,#25191,#25192,#25193,#25194,
#25195,#25196,#25197,#25198,#25199,#25200,#25201,#25202,#25203,#25204,#25205,
#25206,#25207,#25208,#25209,#25210,#25211,#25212,#25213,#25214,#25215,#25216,
#25217,#25218,#25219,#25220,#25221,#25222,#25223,#25224,#25225,#25226,#25227,
#25228,#25229,#25230,#25231,#25232,#25233,#25234,#25235,#25236,#25237,#25238,
#25239,#25240,#25241,#25242,#25243,#25244,#25245,#25246,#25247,#25248,#25249,
#25250,#25251,#25252,#25253,#25254,#25255,#25256,#25257,#25258,#25259,#25260,
#25261,#25262,#25263,#25264,#25265,#25266,#25267,#25268),.UNSPECIFIED.,
 .F.,.F.,(4,3,3,3,3,3,3,3,3,3,3,3,3,3,3,3,3,3,3,3,3,3,3,3,3,3,3,3,3,3,3,
3,3,3,3,3,3,4),(-136.039432956653,-135.825338523247,-135.680984163318,-135.493446114733,
-135.306301672544,-135.119183599805,-134.932076650173,-134.744538465948,
-134.683329867999,-134.495791819414,-134.308647377225,-134.121529304486,
-133.934422354855,-133.74688417063,-133.68567557268,-133.498137524096,-133.310993081908,
-133.12387500917,-132.936768059539,-132.749229875315,-132.688021277362,
-132.500483228777,-132.313338786588,-132.12622071385,-131.939113764218,
-131.751575579994,-131.690366982043,-131.502828933458,-131.31568449127,
-131.128566418532,-130.9414594689,-130.753921284676,-130.692712686725,-130.506853125115,
-130.319201816944,-130.133765499097,-129.945006695764,-129.75624789243),
 .UNSPECIFIED.);
#301=B_SPLINE_CURVE_WITH_KNOTS('',3,(#25270,#25271,#25272,#25273,#25274,
#25275,#25276,#25277,#25278,#25279,#25280),.UNSPECIFIED.,.F.,.F.,(4,1,1,
1,1,1,1,1,4),(-129.75624789243,-129.695058391406,-128.697404096088,-127.699749800769,
-126.702095505451,-125.704441210132,-124.706786914814,-123.709132619495,
-123.473062585251),.UNSPECIFIED.);
#302=B_SPLINE_CURVE_WITH_KNOTS('',3,(#25282,#25283,#25284,#25285,#25286,
#25287,#25288,#25289,#25290,#25291),.UNSPECIFIED.,.F.,.F.,(4,1,1,1,1,1,
1,4),(-123.473062585251,-122.711478324177,-121.713824028858,-120.71616973354,
-119.718515438221,-118.720861142903,-117.723206847584,-117.189877278071),
 .UNSPECIFIED.);
#303=B_SPLINE_CURVE_WITH_KNOTS('',3,(#25293,#25294,#25295,#25296,#25297,
#25298,#25299,#25300,#25301,#25302,#25303,#25304,#25305,#25306,#25307,#25308,
#25309,#25310,#25311,#25312,#25313,#25314,#25315,#25316,#25317,#25318,#25319,
#25320,#25321,#25322,#25323,#25324,#25325,#25326,#25327,#25328,#25329,#25330,
#25331,#25332,#25333,#25334,#25335,#25336,#25337,#25338,#25339,#25340,#25341,
#25342,#25343,#25344,#25345,#25346,#25347,#25348,#25349,#25350,#25351,#25352,
#25353,#25354,#25355,#25356,#25357,#25358,#25359,#25360,#25361,#25362,#25363,
#25364,#25365,#25366,#25367,#25368,#25369,#25370,#25371,#25372,#25373,#25374,
#25375,#25376,#25377,#25378,#25379,#25380,#25381,#25382,#25383,#25384,#25385,
#25386,#25387,#25388,#25389,#25390,#25391,#25392,#25393,#25394,#25395,#25396,
#25397,#25398,#25399,#25400,#25401,#25402,#25403,#25404,#25405,#25406,#25407),
 .UNSPECIFIED.,.F.,.F.,(4,3,3,3,3,3,3,3,3,3,3,3,3,3,3,3,3,3,3,3,3,3,3,3,
3,3,3,3,3,3,3,3,3,3,3,3,3,3,4),(-117.189877092994,-116.990698231071,-116.790432269088,
-116.725552552266,-116.538014503681,-116.350870061492,-116.163751988753,
-115.976645039121,-115.789106854896,-115.727898256947,-115.540360208363,
-115.353215766174,-115.166097693436,-114.978990743805,-114.791452559582,
-114.730243961629,-114.542705913044,-114.355561470855,-114.168443398117,
-113.981336448486,-113.793798264261,-113.73258966631,-113.545051617725,
-113.357907175537,-113.170789102799,-112.983682153167,-112.796143968943,
-112.734935370992,-112.547397322407,-112.360252880219,-112.173134807481,
-111.986027857849,-111.798489673625,-111.737281075673,-111.552535196557,
-111.368083942092,-111.183809075707,-110.999269022242,-110.906691970891),
 .UNSPECIFIED.);
#304=B_SPLINE_CURVE_WITH_KNOTS('',3,(#25409,#25410,#25411,#25412,#25413,
#25414,#25415,#25416,#25417,#25418,#25419),.UNSPECIFIED.,.F.,.F.,(4,1,1,
1,1,1,1,1,4),(-110.906691970891,-110.739626780355,-109.741972485036,-108.744318189718,
-107.746663894399,-106.749009599081,-105.751355303762,-104.753701008444,
-104.623506663712),.UNSPECIFIED.);
#305=B_SPLINE_CURVE_WITH_KNOTS('',3,(#25421,#25422,#25423,#25424,#25425,
#25426,#25427,#25428,#25429,#25430),.UNSPECIFIED.,.F.,.F.,(4,1,1,1,1,1,
1,4),(-104.623506663712,-103.756046713125,-102.758392417807,-101.760738122488,
-100.76308382717,-99.7654295318511,-98.7677752365326,-98.3403266725638),
 .UNSPECIFIED.);
#306=B_SPLINE_CURVE_WITH_KNOTS('',3,(#25432,#25433,#25434,#25435,#25436,
#25437,#25438,#25439,#25440,#25441,#25442,#25443,#25444,#25445,#25446,#25447,
#25448,#25449,#25450,#25451,#25452,#25453,#25454,#25455,#25456,#25457,#25458,
#25459,#25460,#25461,#25462,#25463,#25464,#25465,#25466,#25467,#25468,#25469,
#25470,#25471,#25472,#25473,#25474,#25475,#25476,#25477,#25478,#25479,#25480,
#25481,#25482,#25483,#25484,#25485,#25486,#25487,#25488,#25489,#25490,#25491,
#25492,#25493,#25494,#25495,#25496,#25497,#25498,#25499,#25500,#25501,#25502,
#25503,#25504,#25505,#25506,#25507,#25508,#25509,#25510,#25511,#25512,#25513,
#25514,#25515,#25516,#25517,#25518,#25519,#25520,#25521,#25522,#25523,#25524,
#25525,#25526,#25527,#25528,#25529,#25530,#25531,#25532,#25533,#25534,#25535,
#25536,#25537,#25538,#25539,#25540,#25541,#25542,#25543),.UNSPECIFIED.,
 .F.,.F.,(4,3,3,3,3,3,3,3,3,3,3,3,3,3,3,3,3,3,3,3,3,3,3,3,3,3,3,3,3,3,3,
3,3,3,3,3,3,4),(-98.3403213565322,-98.1491648751557,-97.9573414616566,-97.7701209412141,
-97.5825828926293,-97.3954384504409,-97.2083203777026,-97.0212134280712,
-96.833675243847,-96.7724666458956,-96.5849285973108,-96.3977841551224,
-96.2106660823841,-96.0235591327527,-95.8360209485285,-95.7748123505771,
-95.5872743019923,-95.4001298598038,-95.2130117870654,-95.025904837434,
-94.8383666532097,-94.7771580552585,-94.5896200066737,-94.4024755644853,
-94.215357491747,-94.0282505421157,-93.8407123578914,-93.77950375994,-93.5919657113552,
-93.4048212691667,-93.2177031964284,-93.030596246797,-92.8430580625728,
-92.7818494646215,-92.5960124093366,-92.4105589018408,-92.2250567751402,
-92.0571360493526),.UNSPECIFIED.);
#307=B_SPLINE_CURVE_WITH_KNOTS('',3,(#25545,#25546,#25547,#25548,#25549,
#25550,#25551,#25552,#25553,#25554,#25555),.UNSPECIFIED.,.F.,.F.,(4,1,1,
1,1,1,1,1,4),(-92.0571324486301,-91.784195169303,-90.7865408739845,-89.788886578666,
-88.7912322833475,-87.793577988029,-86.7959236927104,-85.7982693973919,
-85.773950742173),.UNSPECIFIED.);
#308=B_SPLINE_CURVE_WITH_KNOTS('',3,(#25557,#25558,#25559,#25560,#25561,
#25562,#25563,#25564,#25565,#25566),.UNSPECIFIED.,.F.,.F.,(4,1,1,1,1,1,
1,4),(-85.773950742173,-84.8006151020734,-83.8029608067549,-82.8053065114364,
-81.8076522161179,-80.8099979207994,-79.8123436254809,-79.4907721948393),
 .UNSPECIFIED.);
#309=B_SPLINE_CURVE_WITH_KNOTS('',3,(#25568,#25569,#25570,#25571,#25572,
#25573,#25574,#25575,#25576,#25577,#25578,#25579,#25580,#25581,#25582,#25583,
#25584,#25585,#25586,#25587,#25588,#25589,#25590,#25591,#25592,#25593,#25594,
#25595,#25596,#25597,#25598,#25599,#25600,#25601,#25602,#25603,#25604,#25605,
#25606,#25607,#25608,#25609,#25610,#25611,#25612,#25613,#25614,#25615,#25616,
#25617,#25618,#25619,#25620,#25621,#25622,#25623,#25624,#25625,#25626,#25627,
#25628,#25629,#25630,#25631,#25632,#25633,#25634,#25635,#25636,#25637,#25638,
#25639,#25640,#25641,#25642,#25643,#25644,#25645,#25646,#25647,#25648,#25649,
#25650,#25651,#25652,#25653,#25654,#25655,#25656,#25657,#25658,#25659,#25660,
#25661,#25662,#25663,#25664,#25665,#25666,#25667,#25668,#25669,#25670,#25671,
#25672,#25673,#25674,#25675,#25676,#25677,#25678,#25679,#25680,#25681,#25682),
 .UNSPECIFIED.,.F.,.F.,(4,3,3,3,3,3,3,3,3,3,3,3,3,3,3,3,3,3,3,3,3,3,3,3,
3,3,3,3,3,3,3,3,3,3,3,3,3,3,4),(-79.4907654349934,-79.304094347987,-79.1174778110582,
-78.9303964543316,-78.8146893301624,-78.6271512815776,-78.4400068393891,
-78.2528887666508,-78.0657818170195,-77.8782436327954,-77.8170350348439,
-77.629496986259,-77.4423525440705,-77.2552344713322,-77.0681275217008,
-76.8805893374765,-76.8193807395253,-76.6318426909405,-76.4446982487521,
-76.2575801760138,-76.0704732263825,-75.8829350421583,-75.8217264442068,
-75.634188395622,-75.4470439534335,-75.2599258806952,-75.0728189310639,
-74.8852807468398,-74.8240721488883,-74.6365341003035,-74.4493896581151,
-74.2622715853767,-74.0751646357452,-73.887626451521,-73.8264178535698,
-73.6371361639319,-73.448293995353,-73.2596672789205,-73.2075801278138),
 .UNSPECIFIED.);
#310=B_SPLINE_CURVE_WITH_KNOTS('',3,(#25684,#25685,#25686,#25687,#25688,
#25689,#25690,#25691,#25692,#25693),.UNSPECIFIED.,.F.,.F.,(4,1,1,1,1,1,
1,4),(-73.2075727019911,-72.8287635582513,-71.8311092629328,-70.8334549676143,
-69.8358006722958,-68.8381463769772,-67.8404920816587,-66.9243948206342),
 .UNSPECIFIED.);
#311=B_SPLINE_CURVE_WITH_KNOTS('',3,(#25695,#25696,#25697,#25698,#25699,
#25700,#25701,#25702,#25703,#25704,#25705),.UNSPECIFIED.,.F.,.F.,(4,1,1,
1,1,1,1,1,4),(-66.9243948206342,-66.8428377863402,-65.8451834910217,-64.8475291957032,
-63.8498749003847,-62.8522206050662,-61.8545663097477,-60.8569120144292,
-60.6412095134546),.UNSPECIFIED.);
#312=B_SPLINE_CURVE_WITH_KNOTS('',3,(#25707,#25708,#25709,#25710,#25711,
#25712,#25713,#25714,#25715,#25716,#25717,#25718,#25719,#25720,#25721,#25722,
#25723,#25724,#25725,#25726,#25727,#25728,#25729,#25730,#25731,#25732,#25733,
#25734,#25735,#25736,#25737,#25738,#25739,#25740,#25741,#25742,#25743,#25744,
#25745,#25746,#25747,#25748,#25749,#25750,#25751,#25752,#25753,#25754,#25755,
#25756,#25757,#25758,#25759,#25760,#25761,#25762,#25763,#25764,#25765,#25766,
#25767,#25768,#25769,#25770,#25771,#25772,#25773,#25774,#25775,#25776,#25777,
#25778,#25779,#25780,#25781,#25782,#25783,#25784,#25785,#25786,#25787,#25788,
#25789,#25790,#25791,#25792,#25793,#25794,#25795,#25796,#25797,#25798,#25799,
#25800,#25801,#25802,#25803,#25804,#25805,#25806,#25807,#25808,#25809,#25810,
#25811,#25812,#25813,#25814,#25815,#25816,#25817,#25818,#25819,#25820,#25821),
 .UNSPECIFIED.,.F.,.F.,(4,3,3,3,3,3,3,3,3,3,3,3,3,3,3,3,3,3,3,3,3,3,3,3,
3,3,3,3,3,3,3,3,3,3,3,3,3,3,4),(-60.6412095134546,-60.4565760673968,-60.2720035492817,
-60.0874545223872,-59.9024986035968,-59.8592577191107,-59.6717196705258,
-59.4845752283373,-59.2974571555989,-59.1103502059676,-58.9228120217433,
-58.8616034237921,-58.6740653752073,-58.4869209330187,-58.2998028602804,
-58.112695910649,-57.9251577264247,-57.8639491284736,-57.6764110798888,
-57.4892666377004,-57.3021485649622,-57.1150416153308,-56.9275034311067,
-56.8662948331551,-56.6787567845703,-56.4916123423818,-56.3044942696435,
-56.1173873200121,-55.9298491357879,-55.8686405378366,-55.6811024892518,
-55.4939580470634,-55.3068399743251,-55.1197330246937,-54.9321948404695,
-54.8709862425181,-54.6751263136016,-54.4800162445405,-54.358024206275),
 .UNSPECIFIED.);
#313=B_SPLINE_CURVE_WITH_KNOTS('',3,(#25823,#25824,#25825,#25826,#25827,
#25828,#25829,#25830,#25831,#25832),.UNSPECIFIED.,.F.,.F.,(4,1,1,1,1,1,
1,4),(-54.358023115501,-53.8733319471996,-52.8756776518811,-51.8780233565626,
-50.8803690612441,-49.8827147659256,-48.885060470607,-48.0748388990954),
 .UNSPECIFIED.);
#314=B_SPLINE_CURVE_WITH_KNOTS('',3,(#25834,#25835,#25836,#25837,#25838,
#25839,#25840,#25841,#25842,#25843,#25844),.UNSPECIFIED.,.F.,.F.,(4,1,1,
1,1,1,1,1,4),(-48.0748388990954,-47.8874061752885,-46.88975187997,-45.8920975846515,
-44.894443289333,-43.8967889940145,-42.899134698696,-41.9014804033775,-41.7916535919158),
 .UNSPECIFIED.);
#315=B_SPLINE_CURVE_WITH_KNOTS('',3,(#25846,#25847,#25848,#25849,#25850,
#25851,#25852,#25853,#25854,#25855,#25856,#25857,#25858,#25859,#25860,#25861,
#25862,#25863,#25864,#25865,#25866,#25867,#25868,#25869,#25870,#25871,#25872,
#25873,#25874,#25875,#25876,#25877,#25878,#25879,#25880,#25881,#25882,#25883,
#25884,#25885,#25886,#25887,#25888,#25889,#25890,#25891,#25892,#25893,#25894,
#25895,#25896,#25897,#25898,#25899,#25900,#25901,#25902,#25903,#25904,#25905,
#25906,#25907,#25908,#25909,#25910,#25911,#25912,#25913,#25914,#25915,#25916,
#25917,#25918,#25919,#25920,#25921,#25922,#25923,#25924,#25925,#25926,#25927,
#25928,#25929,#25930,#25931,#25932,#25933,#25934,#25935,#25936,#25937,#25938,
#25939,#25940,#25941,#25942,#25943,#25944,#25945,#25946,#25947,#25948,#25949,
#25950,#25951,#25952,#25953,#25954,#25955,#25956,#25957),.UNSPECIFIED.,
 .F.,.F.,(4,3,3,3,3,3,3,3,3,3,3,3,3,3,3,3,3,3,3,3,3,3,3,3,3,3,3,3,3,3,3,
3,3,3,3,3,3,4),(-41.7916535919158,-41.606689253253,-41.4219028141221,-41.2372475937333,
-41.0521611009319,-40.903826108059,-40.7162880594741,-40.5291436172856,
-40.3420255445473,-40.1549185949159,-39.9673804106916,-39.9061718127404,
-39.7186337641556,-39.5314893219672,-39.3443712492289,-39.1572642995975,
-38.9697261153734,-38.9085175174219,-38.7209794688371,-38.5338350266486,
-38.3467169539102,-38.1596100042788,-37.9720718200545,-37.9108632221034,
-37.7233251735186,-37.5361807313301,-37.3490626585918,-37.1619557089604,
-36.9744175247362,-36.9132089267849,-36.7256708782003,-36.5385264360123,
-36.3514083632743,-36.1643014136432,-35.9767632294192,-35.9155546314664,
-35.7089829159113,-35.5084687048588),.UNSPECIFIED.);
#316=B_SPLINE_CURVE_WITH_KNOTS('',3,(#25959,#25960,#25961,#25962,#25963,
#25964,#25965,#25966,#25967,#25968),.UNSPECIFIED.,.F.,.F.,(4,1,1,1,1,1,
1,4),(-35.5084682847362,-34.9179003361479,-33.9202460408294,-32.9225917455109,
-31.9249374501923,-30.9272831548738,-29.9296288595553,-29.2252829775566),
 .UNSPECIFIED.);
#317=B_SPLINE_CURVE_WITH_KNOTS('',3,(#25970,#25971,#25972,#25973,#25974,
#25975,#25976,#25977,#25978,#25979,#25980,#25981,#25982,#25983,#25984,#25985,
#25986,#25987,#25988,#25989,#25990,#25991,#25992,#25993,#25994,#25995,#25996,
#25997,#25998,#25999,#26000,#26001,#26002,#26003,#26004,#26005,#26006,#26007,
#26008,#26009,#26010,#26011,#26012,#26013,#26014,#26015,#26016,#26017,#26018,
#26019,#26020,#26021,#26022,#26023,#26024,#26025,#26026,#26027,#26028,#26029,
#26030,#26031,#26032,#26033,#26034,#26035,#26036,#26037,#26038,#26039,#26040,
#26041,#26042,#26043,#26044,#26045,#26046,#26047,#26048,#26049,#26050,#26051,
#26052,#26053,#26054,#26055,#26056,#26057,#26058,#26059,#26060,#26061,#26062,
#26063,#26064,#26065,#26066,#26067,#26068,#26069,#26070,#26071,#26072,#26073,
#26074,#26075,#26076,#26077,#26078,#26079,#26080,#26081,#26082,#26083,#26084),
 .UNSPECIFIED.,.F.,.F.,(4,3,3,3,3,3,3,3,3,3,3,3,3,3,3,3,3,3,3,3,3,3,3,3,
3,3,3,3,3,3,3,3,3,3,3,3,3,3,4),(-29.2252828103121,-28.9967968814183,-28.9319745642368,
-28.7444365156814,-28.557292073522,-28.3701740008118,-28.1830670512081,
-27.9955288670104,-27.9343202689183,-27.746782220377,-27.5596377782329,
-27.3725197055393,-27.1854127559528,-26.9978745717731,-26.9366659735998,
-26.7491279248186,-26.5619834824335,-26.374865409501,-26.1877584596766,
-26.0002202752648,-25.9390116782813,-25.751473629944,-25.5643291880011,
-25.3772111155019,-25.1901041661061,-25.002565982108,-24.9413573829628,
-24.7538193345779,-24.5666748925946,-24.3795568200659,-24.1924498706469,
-24.0049116866351,-23.9437030876443,-23.7560287176089,-23.5687482990062,
-23.3814945807613,-23.1942535727822,-23.0065797464408,-22.9420976703771),
 .UNSPECIFIED.);
#318=B_SPLINE_CURVE_WITH_KNOTS('',3,(#26086,#26087,#26088,#26089,#26090,
#26091,#26092,#26093,#26094,#26095,#26096,#26097,#26098,#26099,#26100,#26101,
#26102,#26103,#26104,#26105,#26106,#26107,#26108,#26109,#26110,#26111,#26112,
#26113,#26114,#26115,#26116,#26117,#26118,#26119,#26120,#26121,#26122,#26123,
#26124,#26125,#26126,#26127,#26128,#26129,#26130,#26131,#26132,#26133,#26134,
#26135,#26136,#26137,#26138,#26139,#26140,#26141,#26142,#26143,#26144,#26145,
#26146,#26147,#26148,#26149,#26150,#26151,#26152,#26153,#26154,#26155,#26156,
#26157,#26158,#26159,#26160,#26161,#26162,#26163,#26164,#26165,#26166,#26167,
#26168,#26169,#26170,#26171,#26172,#26173,#26174,#26175,#26176,#26177,#26178,
#26179,#26180,#26181,#26182,#26183,#26184,#26185,#26186,#26187,#26188,#26189,
#26190,#26191,#26192,#26193,#26194,#26195,#26196,#26197,#26198,#26199,#26200),
 .UNSPECIFIED.,.F.,.F.,(4,3,3,3,3,3,3,3,3,3,3,3,3,3,3,3,3,3,3,3,3,3,3,3,
3,3,3,3,3,3,3,3,3,3,3,3,3,3,4),(-22.9420976699444,-22.7546926683555,-22.5676808462314,
-22.3806950377695,-22.1937187529239,-22.0063128931654,-21.9483944970072,
-21.7608564490805,-21.5737120075872,-21.3865939355861,-21.1994869867172,
-21.0119488032776,-20.9507402016887,-20.7632021445966,-20.5760576938657,
-20.3889396126633,-20.2018326546044,-20.014294462161,-19.9530859063702,
-19.7655478729557,-19.5784034458762,-19.3912853879325,-19.2041784529296,
-19.0166402828235,-18.9554316110517,-18.7678935619543,-18.5807491195069,
-18.3936310468746,-18.2065240975601,-18.0189859139515,-17.9577773157332,
-17.7702392133082,-17.583094716978,-17.3959765904825,-17.2088695872607,
-17.0213313506759,-16.9601230204147,-16.7337449968225,-16.6589125463892),
 .UNSPECIFIED.);
#319=B_SPLINE_CURVE_WITH_KNOTS('',3,(#26202,#26203,#26204,#26205,#26206,
#26207,#26208,#26209,#26210,#26211),.UNSPECIFIED.,.F.,.F.,(4,1,1,1,1,1,
1,4),(-16.6589123631975,-15.9624687250962,-14.9648144297777,-13.9671601344592,
-12.9695058391406,-11.9718515438221,-10.9741972485036,-10.3757270560179),
 .UNSPECIFIED.);
#320=B_SPLINE_CURVE_WITH_KNOTS('',3,(#26212,#26213,#26214,#26215,#26216,
#26217,#26218,#26219,#26220,#26221),.UNSPECIFIED.,.F.,.F.,(4,1,1,1,1,1,
1,4),(-10.3757270560179,-9.97654295318511,-8.9788886578666,-7.98123436254809,
-6.98358006722958,-5.98592577191107,-4.98827147659255,-4.09255058081676),
 .UNSPECIFIED.);
#321=B_SPLINE_CURVE_WITH_KNOTS('',3,(#26224,#26225,#26226,#26227,#26228,
#26229,#26230,#26231,#26232,#26233,#26234,#26235,#26236,#26237,#26238,#26239,
#26240,#26241,#26242,#26243,#26244,#26245,#26246,#26247,#26248,#26249,#26250,
#26251,#26252,#26253,#26254,#26255,#26256,#26257,#26258,#26259,#26260,#26261,
#26262,#26263,#26264,#26265,#26266,#26267,#26268,#26269,#26270,#26271,#26272,
#26273,#26274,#26275,#26276,#26277,#26278,#26279,#26280,#26281,#26282,#26283,
#26284,#26285,#26286,#26287,#26288,#26289,#26290,#26291,#26292,#26293,#26294,
#26295,#26296,#26297,#26298,#26299,#26300,#26301,#26302,#26303,#26304,#26305,
#26306,#26307,#26308,#26309,#26310,#26311,#26312,#26313,#26314,#26315,#26316,
#26317,#26318,#26319,#26320,#26321,#26322,#26323,#26324,#26325,#26326,#26327,
#26328,#26329,#26330,#26331,#26332,#26333,#26334,#26335,#26336,#26337,#26338,
#26339,#26340,#26341,#26342,#26343,#26344,#26345,#26346,#26347,#26348,#26349,
#26350,#26351,#26352,#26353,#26354,#26355,#26356,#26357,#26358,#26359,#26360,
#26361,#26362,#26363,#26364,#26365,#26366,#26367,#26368,#26369,#26370,#26371,
#26372,#26373,#26374,#26375,#26376,#26377,#26378,#26379,#26380,#26381,#26382,
#26383,#26384,#26385,#26386,#26387,#26388,#26389,#26390,#26391,#26392,#26393,
#26394,#26395,#26396,#26397,#26398,#26399,#26400,#26401,#26402,#26403,#26404,
#26405,#26406,#26407,#26408,#26409,#26410,#26411,#26412,#26413,#26414,#26415,
#26416,#26417,#26418,#26419,#26420,#26421,#26422,#26423,#26424,#26425,#26426,
#26427,#26428,#26429,#26430,#26431,#26432,#26433,#26434,#26435,#26436,#26437,
#26438,#26439,#26440,#26441,#26442,#26443,#26444,#26445,#26446,#26447,#26448,
#26449,#26450,#26451,#26452,#26453,#26454,#26455,#26456,#26457,#26458,#26459,
#26460,#26461),.UNSPECIFIED.,.F.,.F.,(4,2,2,2,2,2,2,2,2,2,2,2,2,2,2,2,2,
2,2,2,2,2,2,2,2,2,2,2,2,2,2,2,2,2,2,2,2,2,2,2,2,2,2,2,2,2,2,2,2,2,2,2,2,
2,2,2,2,2,2,2,2,2,2,2,2,2,2,2,2,2,2,2,2,2,2,2,2,2,2,2,2,2,2,2,2,2,2,2,2,
2,2,2,2,2,2,2,2,2,2,2,2,2,2,2,2,2,2,2,2,2,2,2,2,2,2,2,2,2,4),(0.00242918935322954,
0.0505226468104856,0.0640385215741708,0.0669286141768185,0.0685648686987503,
0.0698307604367571,0.0714826753751052,0.0743653603778451,0.0862943637434652,
0.134113484602536,0.142180620281222,0.143852029721217,0.144770387023611,
0.144773779031473,0.14477721763177,0.144780703710955,0.144784238174555,
0.144787821959457,0.144791456033152,0.144795141369183,0.144798878976188,
0.144802669887737,0.144806515164096,0.144810415902515,0.144814373219479,
0.144818388256983,0.14482246218383,0.144826596235181,0.144830791648857,
0.144835049687563,0.144839371667068,0.144843758943846,0.144848212891647,
0.144852734924487,0.144857326511917,0.144861989155769,0.144866724407045,
0.144871533853314,0.144876419120238,0.144881381891246,0.144886423900231,
0.14566638153748,0.146677815262381,0.148757527729657,0.171783571528887,
0.196782559947427,0.210240787798856,0.218362841192007,0.220794721189844,
0.222317759204107,0.223723438679273,0.225535860417369,0.228537058752678,
0.247993293423039,0.279604858173132,0.291922205180772,0.298232088044613,
0.2997523291405,0.300629094591326,0.301384669018166,0.302348035457082,0.304253869745646,
0.316704528616778,0.35369951060433,0.366633777158306,0.374512391147684,
0.376898922896855,0.378399402173584,0.379788141857469,0.381584041810109,
0.384569105905836,0.404403899847237,0.436386959026362,0.448092667714902,
0.454177972001239,0.455670829512531,0.456541673307705,0.457319337950041,
0.458321442969748,0.459979184762913,0.469885443273327,0.474044967198328,
0.477793798562439,0.521127178688317,0.530261230573272,0.532790624444463,
0.534332636991339,0.535728223937639,0.537519441663396,0.540392734731223,
0.556933725177588,0.601629007291696,0.609449109466361,0.611077051839486,
0.611984877523952,0.612762212040367,0.613744288517051,0.615734937152515,
0.629153701833238,0.674154376990143,0.685318692935192,0.688016240151554,
0.689593218484605,0.690978977752344,0.692702401801144,0.695360473672499,
0.708141141000251,0.713107609325545,0.756919625772014,0.765145527407682,
0.766792023320811,0.767701150500468,0.768475133820461,0.769446637304088,
0.771330455415657,0.782652593667203,0.785658621100046,0.801643789430652,
0.801779048931175),.UNSPECIFIED.);
#322=B_SPLINE_CURVE_WITH_KNOTS('',3,(#26465,#26466,#26467,#26468,#26469,
#26470,#26471,#26472,#26473,#26474,#26475,#26476,#26477,#26478,#26479,#26480,
#26481,#26482,#26483,#26484,#26485,#26486,#26487,#26488,#26489,#26490,#26491,
#26492,#26493,#26494,#26495,#26496,#26497,#26498,#26499,#26500,#26501,#26502,
#26503,#26504,#26505,#26506,#26507),.UNSPECIFIED.,.F.,.F.,(4,3,3,3,3,3,
3,3,3,3,3,3,3,3,4),(223.053078404875,223.249759833269,223.446265667279,
223.643245097141,223.803914711538,224.000284327898,224.200605497638,224.396553130159,
224.599061068508,224.801569006857,225.005649510053,225.209253391211,225.412535507524,
225.615947120473,225.799223302175),.UNSPECIFIED.);
#323=B_SPLINE_CURVE_WITH_KNOTS('',3,(#26508,#26509,#26510,#26511,#26512,
#26513,#26514,#26515,#26516,#26517,#26518,#26519,#26520,#26521,#26522,#26523,
#26524,#26525,#26526,#26527,#26528,#26529,#26530,#26531,#26532,#26533,#26534,
#26535,#26536,#26537,#26538,#26539,#26540,#26541,#26542,#26543,#26544,#26545,
#26546,#26547,#26548,#26549,#26550,#26551),.UNSPECIFIED.,.F.,.F.,(4,2,2,
2,2,2,2,2,2,2,2,2,2,2,2,2,2,2,2,2,2,4),(-1.96155998999565,-1.93145588063156,
-1.92783250967384,-1.92604050708938,-1.92494602585897,-1.9241353570081,
-1.92332132892803,-1.92256838047723,-1.92128904881891,-1.91780013673092,
-1.89003524213539,-1.87442280300735,-1.85403488840081,-1.84929335704467,
-1.84774484628021,-1.8462297091599,-1.84482039163455,-1.84298779932934,
-1.83991922159517,-1.81784809663805,-1.79351172412742,-1.78243981456369),
 .UNSPECIFIED.);
#324=B_SPLINE_CURVE_WITH_KNOTS('',3,(#27436,#27437,#27438,#27439,#27440,
#27441,#27442,#27443,#27444,#27445,#27446,#27447,#27448,#27449,#27450,#27451,
#27452,#27453,#27454,#27455,#27456,#27457,#27458,#27459,#27460,#27461,#27462,
#27463,#27464,#27465,#27466,#27467,#27468,#27469,#27470,#27471,#27472,#27473,
#27474,#27475,#27476,#27477,#27478,#27479,#27480,#27481,#27482,#27483,#27484,
#27485,#27486,#27487,#27488,#27489,#27490),.UNSPECIFIED.,.F.,.F.,(4,3,3,
3,3,3,3,3,3,3,3,3,3,3,3,3,3,3,4),(3.98819129420962E-5,0.0136872263540572,
0.0522766260806668,0.0709950800646878,0.0819953190919729,0.119305547150835,
0.143879290941371,0.156749831780157,0.182262464866333,0.192145397802465,
0.199552864933563,0.215672767979732,0.228806216382242,0.263204057038138,
0.279098426169674,0.293672482722726,0.320133366208391,0.333322815206606,
0.366397579005826),.UNSPECIFIED.);
#325=B_SPLINE_CURVE_WITH_KNOTS('',3,(#27492,#27493,#27494,#27495,#27496,
#27497,#27498,#27499,#27500,#27501,#27502,#27503,#27504,#27505,#27506,#27507,
#27508,#27509,#27510,#27511,#27512,#27513,#27514,#27515,#27516,#27517,#27518,
#27519,#27520,#27521,#27522,#27523,#27524,#27525,#27526,#27527,#27528,#27529,
#27530,#27531,#27532,#27533,#27534,#27535,#27536,#27537,#27538,#27539,#27540,
#27541,#27542,#27543),.UNSPECIFIED.,.F.,.F.,(4,3,3,3,3,3,3,3,3,3,3,3,3,
3,3,3,3,4),(-0.366397579005832,-0.355349081053819,-0.328627709487585,-0.313113754886802,
-0.287021709507735,-0.271827012252881,-0.236673702273149,-0.219261174131459,
-0.205739586164244,-0.187146499846321,-0.163753187365531,-0.146916306560471,
-0.134322373995578,-0.100741780496684,-0.0810578579737637,-0.0639676522746132,
-0.0255059552299406,0.),.UNSPECIFIED.);
#326=B_SPLINE_CURVE_WITH_KNOTS('',3,(#27544,#27545,#27546,#27547),
 .UNSPECIFIED.,.F.,.F.,(4,4),(-0.0124837338197822,0.),.UNSPECIFIED.);
#327=B_SPLINE_CURVE_WITH_KNOTS('',3,(#28433,#28434,#28435,#28436,#28437,
#28438,#28439,#28440,#28441,#28442,#28443,#28444,#28445,#28446,#28447,#28448,
#28449,#28450,#28451,#28452,#28453,#28454,#28455,#28456,#28457,#28458,#28459,
#28460,#28461,#28462,#28463,#28464,#28465,#28466,#28467,#28468,#28469,#28470,
#28471,#28472,#28473,#28474,#28475,#28476,#28477,#28478,#28479,#28480,#28481,
#28482,#28483,#28484,#28485,#28486,#28487),.UNSPECIFIED.,.F.,.F.,(4,3,3,
3,3,3,3,3,3,3,3,3,3,3,3,3,3,3,4),(0.,0.0110072508574968,0.0431732332201684,
0.0597682846665091,0.0725876156054097,0.101643661993379,0.12367084288124,
0.136673094424233,0.169449851669546,0.178576016460901,0.191988153704559,
0.204131677343237,0.240029786311497,0.259562619766513,0.274889031344431,
0.300880821280637,0.315410186444722,0.35044636731004,0.364629307890676),
 .UNSPECIFIED.);
#328=B_SPLINE_CURVE_WITH_KNOTS('',3,(#28488,#28489,#28490,#28491),
 .UNSPECIFIED.,.F.,.F.,(4,4),(0.,0.0126590312177446),.UNSPECIFIED.);
#329=B_SPLINE_CURVE_WITH_KNOTS('',3,(#28492,#28493,#28494,#28495,#28496,
#28497,#28498,#28499,#28500,#28501,#28502,#28503,#28504,#28505,#28506,#28507,
#28508,#28509,#28510,#28511,#28512,#28513,#28514,#28515,#28516,#28517,#28518,
#28519,#28520,#28521,#28522,#28523,#28524,#28525,#28526,#28527,#28528,#28529,
#28530,#28531,#28532,#28533,#28534,#28535,#28536,#28537,#28538,#28539,#28540,
#28541,#28542,#28543,#28544,#28545,#28546),.UNSPECIFIED.,.F.,.F.,(4,3,3,
3,3,3,3,3,3,3,3,3,3,3,3,3,3,3,4),(-0.364629307890679,-0.351009649103909,
-0.326038221408134,-0.303066964546125,-0.28084190913311,-0.266670788375262,
-0.255213797252058,-0.218743200019854,-0.200542226689968,-0.18462877353026,
-0.166229720628164,-0.142000108891583,-0.126480131478723,-0.113571829528596,
-0.085178872146449,-0.0628315401147363,-0.0519092898672653,-0.0282641710864551,
-9.4448362746773E-15),.UNSPECIFIED.);
#330=B_SPLINE_CURVE_WITH_KNOTS('',3,(#28599,#28600,#28601,#28602),
 .UNSPECIFIED.,.F.,.F.,(4,4),(49.3506092576781,49.7801089105574),
 .UNSPECIFIED.);
#331=B_SPLINE_CURVE_WITH_KNOTS('',3,(#28605,#28606,#28607,#28608,#28609,
#28610,#28611,#28612,#28613,#28614,#28615,#28616,#28617,#28618,#28619,#28620,
#28621,#28622,#28623),.UNSPECIFIED.,.F.,.F.,(4,3,3,3,3,3,4),(49.3501477946335,
49.5348989026236,49.7266884378777,49.9110953116898,50.0955292586399,50.2803754004188,
50.3020570436401),.UNSPECIFIED.);
#332=B_SPLINE_CURVE_WITH_KNOTS('',3,(#28629,#28630,#28631,#28632,#28633,
#28634,#28635,#28636,#28637,#28638,#28639,#28640,#28641,#28642,#28643,#28644,
#28645,#28646,#28647,#28648,#28649,#28650,#28651,#28652,#28653,#28654,#28655,
#28656,#28657,#28658,#28659,#28660,#28661,#28662,#28663,#28664,#28665,#28666,
#28667,#28668,#28669,#28670,#28671,#28672,#28673,#28674,#28675,#28676,#28677,
#28678,#28679,#28680,#28681,#28682,#28683,#28684,#28685,#28686,#28687,#28688,
#28689,#28690,#28691,#28692,#28693,#28694,#28695,#28696,#28697,#28698,#28699,
#28700,#28701),.UNSPECIFIED.,.F.,.F.,(4,3,3,3,3,3,3,3,3,3,3,3,3,3,3,3,3,
3,3,3,3,3,3,3,4),(43.0673059246895,43.2522056112633,43.4369952653634,43.6222398069954,
43.7929727674573,43.9782156793092,44.163074354931,44.3479065500446,44.5327226681015,
44.7179657215877,44.7908287913073,44.9757569333487,45.1602993349711,45.3448177893337,
45.5293212386388,45.7142590545009,45.7886848151573,45.9742323297121,46.1593920065477,
46.3445154630064,46.5296175368451,46.715133360823,46.7865408390073,47.000219585859,
47.1238896025612),.UNSPECIFIED.);
#333=B_SPLINE_CURVE_WITH_KNOTS('',3,(#28702,#28703,#28704,#28705,#28706,
#28707),.UNSPECIFIED.,.F.,.F.,(4,1,1,4),(47.1238898038469,47.7843968628573,
48.7822528867074,49.3506092576781),.UNSPECIFIED.);
#334=B_SPLINE_CURVE_WITH_KNOTS('',3,(#28709,#28710,#28711,#28712,#28713,
#28714,#28715,#28716,#28717,#28718,#28719,#28720,#28721,#28722,#28723,#28724,
#28725,#28726,#28727,#28728,#28729,#28730,#28731,#28732,#28733,#28734,#28735,
#28736,#28737,#28738,#28739,#28740,#28741,#28742,#28743,#28744,#28745,#28746,
#28747,#28748,#28749,#28750,#28751),.UNSPECIFIED.,.F.,.F.,(4,3,3,3,3,3,
3,3,3,3,3,3,3,3,4),(47.1238898038469,47.3273897998275,47.51231737018,47.6968591993505,
47.8813770883876,48.0658799756973,48.2508172448081,48.3252458236776,48.5107935857524,
48.6959535054872,48.8810771946655,49.0661794955925,49.2516955342477,49.3231018475276,
49.3501477946335),.UNSPECIFIED.);
#335=B_SPLINE_CURVE_WITH_KNOTS('',3,(#28752,#28753,#28754,#28755,#28756,
#28757,#28758,#28759),.UNSPECIFIED.,.F.,.F.,(4,1,1,1,1,4),(43.0658538860988,
43.3359657044275,44.3338217282775,45.3316777521275,46.3295337759775,47.1238866805092),
 .UNSPECIFIED.);
#336=B_SPLINE_CURVE_WITH_KNOTS('',3,(#28765,#28766,#28767,#28768,#28769,
#28770,#28771,#28772,#28773,#28774,#28775,#28776,#28777,#28778,#28779,#28780,
#28781,#28782,#28783,#28784,#28785,#28786,#28787,#28788,#28789,#28790,#28791,
#28792,#28793,#28794,#28795,#28796,#28797,#28798,#28799,#28800,#28801,#28802,
#28803,#28804,#28805,#28806,#28807,#28808,#28809,#28810,#28811,#28812,#28813,
#28814,#28815,#28816,#28817,#28818,#28819,#28820,#28821,#28822,#28823,#28824,
#28825,#28826,#28827,#28828,#28829,#28830,#28831,#28832,#28833,#28834,#28835,
#28836,#28837,#28838,#28839,#28840,#28841,#28842,#28843),.UNSPECIFIED.,
 .F.,.F.,(4,3,3,3,3,3,3,3,3,3,3,3,3,3,3,3,3,3,3,3,3,3,3,3,3,3,4),(36.7834219822921,
36.8079806005072,36.9931719387593,37.1779780330912,37.362756993202,37.5475194411345,
37.7327091962842,37.8058366243572,37.9910292938932,38.1758367476732,38.3606170872144,
38.5453809276248,38.7305720682194,38.8036926482072,38.9888779939723,39.1736781071512,
39.3584511917718,39.5432078181554,39.72839194028,39.8015486720572,39.9867443267892,
40.1715546811428,40.356337756726,40.5411042418332,40.7262978434319,40.7994046959072,
40.8407044966673),.UNSPECIFIED.);
#337=B_SPLINE_CURVE_WITH_KNOTS('',3,(#28844,#28845,#28846,#28847,#28848,
#28849,#28850,#28851,#28852,#28853,#28854,#28855,#28856,#28857,#28858,#28859,
#28860,#28861,#28862,#28863,#28864,#28865,#28866,#28867,#28868,#28869,#28870,
#28871,#28872,#28873,#28874,#28875,#28876,#28877,#28878,#28879,#28880,#28881,
#28882,#28883,#28884,#28885,#28886),.UNSPECIFIED.,.F.,.F.,(4,3,3,3,3,3,
3,3,3,3,3,3,3,3,4),(40.8407044969516,41.0246827204584,41.2178272202831,
41.4014105178206,41.5850067089575,41.7690121301243,41.7972607197572,41.9824130884132,
42.1671801883195,42.351920700675,42.536644970248,42.7217976592989,42.7951167436073,
42.980347380645,43.0673059246895),.UNSPECIFIED.);
#338=B_SPLINE_CURVE_WITH_KNOTS('',3,(#28888,#28889,#28890,#28891,#28892,
#28893),.UNSPECIFIED.,.F.,.F.,(4,1,1,4),(40.8407044966673,41.3402536567274,
42.3381096805775,43.0658538860988),.UNSPECIFIED.);
#339=B_SPLINE_CURVE_WITH_KNOTS('',3,(#28894,#28895,#28896,#28897,#28898,
#28899,#28900,#28901),.UNSPECIFIED.,.F.,.F.,(4,1,1,1,1,4),(36.7839118243441,
37.3488295613274,38.3466855851774,39.3445416090274,40.3423976328774,40.8407044966673),
 .UNSPECIFIED.);
#340=B_SPLINE_CURVE_WITH_KNOTS('',3,(#28907,#28908,#28909,#28910,#28911,
#28912,#28913,#28914),.UNSPECIFIED.,.F.,.F.,(4,1,1,1,1,4),(30.499580403825,
30.8208444574071,31.8187004812571,32.8165565051071,33.8144125289571,34.5575191894877),
 .UNSPECIFIED.);
#341=B_SPLINE_CURVE_WITH_KNOTS('',3,(#28915,#28916,#28917,#28918,#28919,
#28920,#28921,#28922,#28923,#28924,#28925,#28926,#28927,#28928,#28929,#28930,
#28931,#28932,#28933,#28934,#28935,#28936,#28937,#28938,#28939,#28940,#28941,
#28942,#28943,#28944,#28945,#28946,#28947,#28948,#28949,#28950,#28951,#28952,
#28953,#28954,#28955,#28956,#28957),.UNSPECIFIED.,.F.,.F.,(4,3,3,3,3,3,
3,3,3,3,3,3,3,3,4),(34.5575193250544,34.7954285477193,34.8122685528071,
34.9974597158663,35.1822656476729,35.3670444658238,35.5518067834417,35.736996427808,
35.8101245766571,35.995316001551,36.1801199401346,36.3648794202756,36.5496215205385,
36.7347510048651,36.7834219822921),.UNSPECIFIED.);
#342=B_SPLINE_CURVE_WITH_KNOTS('',3,(#28959,#28960,#28961,#28962,#28963,
#28964),.UNSPECIFIED.,.F.,.F.,(4,1,1,4),(34.557522089489,35.3531175136273,
36.3509735374774,36.7839118243441),.UNSPECIFIED.);
#343=B_SPLINE_CURVE_WITH_KNOTS('',3,(#28965,#28966,#28967,#28968,#28969,
#28970,#28971,#28972,#28973,#28974,#28975,#28976,#28977,#28978,#28979,#28980,
#28981,#28982,#28983,#28984,#28985,#28986,#28987,#28988,#28989,#28990,#28991,
#28992,#28993,#28994,#28995,#28996,#28997,#28998,#28999,#29000,#29001,#29002,
#29003,#29004,#29005,#29006,#29007,#29008,#29009,#29010,#29011,#29012,#29013,
#29014,#29015,#29016,#29017,#29018,#29019,#29020,#29021,#29022,#29023,#29024,
#29025,#29026,#29027,#29028,#29029,#29030,#29031,#29032,#29033,#29034,#29035,
#29036,#29037),.UNSPECIFIED.,.F.,.F.,(4,3,3,3,3,3,3,3,3,3,3,3,3,3,3,3,3,
3,3,3,3,3,3,3,4),(30.5009095955721,30.6857963547127,30.8706077913032,31.0553571065148,
31.2405467884087,31.3616934182273,31.5468843306913,31.7316900105254,31.9164685785166,
32.1012306467307,32.2864200475027,32.3595494420773,32.5447402838676,32.7295458923946,
32.9143243892346,33.0990863863056,33.2842757172801,33.3574054659273,33.5425963097738,
33.7274019194642,33.9121804161483,34.0969424123043,34.2821317412473,34.3552614897773,
34.5575191894877),.UNSPECIFIED.);
#344=B_SPLINE_CURVE_WITH_KNOTS('',3,(#29043,#29044,#29045,#29046,#29047,
#29048,#29049,#29050),.UNSPECIFIED.,.F.,.F.,(4,1,1,1,1,4),(24.2177779943852,
24.833708314307,25.831564338157,26.829420362007,27.827276385857,28.2743338823081),
 .UNSPECIFIED.);
#345=B_SPLINE_CURVE_WITH_KNOTS('',3,(#29051,#29052,#29053,#29054,#29055,
#29056),.UNSPECIFIED.,.F.,.F.,(4,1,1,4),(28.2743338823081,28.825132409707,
29.822988433557,30.499580403825),.UNSPECIFIED.);
#346=B_SPLINE_CURVE_WITH_KNOTS('',3,(#29058,#29059,#29060,#29061,#29062,
#29063,#29064,#29065,#29066,#29067,#29068,#29069,#29070,#29071,#29072,#29073,
#29074,#29075,#29076,#29077,#29078,#29079,#29080,#29081,#29082,#29083,#29084,
#29085,#29086,#29087,#29088,#29089,#29090,#29091,#29092,#29093,#29094,#29095,
#29096,#29097,#29098,#29099,#29100),.UNSPECIFIED.,.F.,.F.,(4,3,3,3,3,3,
3,3,3,3,3,3,3,3,4),(28.2743338823081,28.3681253466772,28.5533165056894,
28.7381224361274,28.9229012568358,29.1076635792727,29.292853231745,29.3659813705272,
29.5511722540038,29.7359779062434,29.9207564491344,30.105518493657,30.2907078733232,
30.3638373943772,30.5009095955721),.UNSPECIFIED.);
#347=B_SPLINE_CURVE_WITH_KNOTS('',3,(#29101,#29102,#29103,#29104,#29105,
#29106,#29107,#29108),.UNSPECIFIED.,.F.,.F.,(4,1,1,1,1,4),(24.2163877000371,
24.3767012512771,25.3745572751272,26.3724132989772,27.3702693228272,28.2743251167369),
 .UNSPECIFIED.);
#348=B_SPLINE_CURVE_WITH_KNOTS('',3,(#29114,#29115,#29116,#29117,#29118,
#29119),.UNSPECIFIED.,.F.,.F.,(4,1,1,4),(15.7079632679489,16.393853060477,
17.391709084327,17.9337114285602),.UNSPECIFIED.);
#349=B_SPLINE_CURVE_WITH_KNOTS('',3,(#29121,#29122,#29123,#29124,#29125),
 .UNSPECIFIED.,.F.,.F.,(4,1,4),(14.398141012777,15.395997036627,15.7079632679489),
 .UNSPECIFIED.);
#350=B_SPLINE_CURVE_WITH_KNOTS('',3,(#29129,#29130,#29131,#29132,#29133,
#29134,#29135,#29136,#29137,#29138,#29139,#29140,#29141,#29142,#29143,#29144,
#29145,#29146,#29147,#29148,#29149,#29150,#29151,#29152,#29153,#29154,#29155,
#29156,#29157,#29158,#29159,#29160,#29161,#29162),.UNSPECIFIED.,.F.,.F.,
(4,3,3,3,3,3,3,3,3,3,3,4),(13.8761928799105,14.0610251969122,14.2454741135462,
14.4298929930741,14.614300434641,14.7991186579602,14.8551480758068,15.0378750128527,
15.22034104049,15.4026395868345,15.5852458051357,15.7079632679489),
 .UNSPECIFIED.);
#351=B_SPLINE_CURVE_WITH_KNOTS('',3,(#29163,#29164,#29165,#29166,#29167,
#29168,#29169),.UNSPECIFIED.,.F.,.F.,(4,1,1,1,4),(15.7079632679489,15.8530040996568,
16.8508601235068,17.8487161473568,17.9345037532639),.UNSPECIFIED.);
#352=B_SPLINE_CURVE_WITH_KNOTS('',3,(#29176,#29177,#29178,#29179,#29180,
#29181,#29182),.UNSPECIFIED.,.F.,.F.,(4,3,4),(-35.9039115982717,-35.7093251171368,
-35.6145585437837),.UNSPECIFIED.);
#353=B_SPLINE_CURVE_WITH_KNOTS('',3,(#29188,#29189,#29190,#29191,#29192,
#29193,#29194,#29195,#29196,#29197,#29198,#29199,#29200,#29201,#29202,#29203,
#29204,#29205,#29206,#29207,#29208,#29209,#29210,#29211,#29212,#29213,#29214,
#29215,#29216,#29217,#29218,#29219,#29220,#29221,#29222,#29223,#29224,#29225,
#29226,#29227,#29228,#29229,#29230,#29231,#29232,#29233,#29234,#29235,#29236,
#29237,#29238,#29239,#29240,#29241,#29242,#29243,#29244,#29245,#29246,#29247,
#29248,#29249,#29250,#29251,#29252,#29253,#29254,#29255,#29256,#29257,#29258,
#29259,#29260,#29261,#29262,#29263,#29264,#29265,#29266),.UNSPECIFIED.,
 .F.,.F.,(4,3,3,3,3,3,3,3,3,3,3,3,3,3,3,3,3,3,3,3,3,3,3,3,3,3,4),(33.0790390540969,
33.2735762055381,33.46804344454,33.6624725923823,33.8573645120063,33.9271048109006,
34.1226408072398,34.3232208141175,34.5182959535662,34.7216283941584,34.9249608347506,
35.1203950360828,35.3210004917123,35.5160009265929,35.7194088925967,35.9228168586006,
36.1158604071302,36.3170635259603,36.5096929699558,36.7023561566481,36.8955227366531,
36.9206728824506,37.1212646060516,37.3213945687078,37.521209127055,37.7211565859618,
37.9185289063006),.UNSPECIFIED.);
#354=B_SPLINE_CURVE_WITH_KNOTS('',3,(#29269,#29270,#29271,#29272,#29273,
#29274,#29275),.UNSPECIFIED.,.F.,.F.,(4,3,4),(-35.6145585437837,-35.4203717509587,
-35.2623097995902),.UNSPECIFIED.);
#355=B_SPLINE_CURVE_WITH_KNOTS('',3,(#29276,#29277,#29278,#29279,#29280,
#29281,#29282,#29283,#29284,#29285,#29286,#29287,#29288,#29289,#29290,#29291,
#29292,#29293,#29294,#29295,#29296,#29297,#29298,#29299,#29300,#29301,#29302,
#29303,#29304,#29305,#29306,#29307,#29308,#29309,#29310,#29311,#29312,#29313,
#29314,#29315,#29316,#29317,#29318,#29319,#29320,#29321,#29322,#29323,#29324,
#29325,#29326,#29327,#29328,#29329,#29330,#29331,#29332,#29333,#29334,#29335,
#29336,#29337,#29338,#29339,#29340,#29341,#29342,#29343,#29344,#29345,#29346,
#29347,#29348,#29349,#29350,#29351,#29352,#29353,#29354,#29355,#29356,#29357,
#29358,#29359,#29360,#29361,#29362,#29363,#29364,#29365,#29366,#29367,#29368,
#29369,#29370,#29371,#29372,#29373,#29374,#29375,#29376,#29377,#29378,#29379,
#29380,#29381,#29382,#29383,#29384,#29385,#29386,#29387,#29388,#29389,#29390,
#29391,#29392,#29393,#29394,#29395,#29396,#29397,#29398,#29399,#29400,#29401,
#29402,#29403,#29404,#29405,#29406,#29407,#29408,#29409,#29410,#29411,#29412,
#29413,#29414,#29415,#29416,#29417),.UNSPECIFIED.,.F.,.F.,(4,2,2,2,2,2,
2,2,2,2,2,2,2,2,2,2,2,2,2,2,2,2,2,2,2,2,2,2,2,2,2,2,2,2,2,2,2,2,2,2,2,2,
2,2,2,2,2,2,2,2,2,2,2,2,2,2,2,2,2,2,2,2,2,2,2,2,2,2,2,2,4),(-2.09956907933678,
-2.06727823295237,-2.05113928097752,-2.04526555762392,-2.04069307487311,
-2.03395102562868,-2.0049198629128,-1.97492707024399,-1.96497929591049,
-1.9571746485176,-1.94784846270027,-1.92838554133457,-1.89840120523387,
-1.88397088568164,-1.87832989099013,-1.87386120551477,-1.86834424737194,
-1.8491586326455,-1.82144758790311,-1.80429694004099,-1.79556342272441,
-1.78779550168319,-1.77722589230856,-1.74615256112504,-1.72734733537564,
-1.71922792962137,-1.71265167434785,-1.70819167444808,-1.70255259139146,
-1.68966202158187,-1.65645274471046,-1.63785863086284,-1.62888569237065,
-1.62106710750307,-1.6108374858822,-1.58812458017681,-1.56329361085236,
-1.55008067968731,-1.54457821075647,-1.54005036449493,-1.53309163082334,
-1.51022880175722,-1.48620348032539,-1.47021600955296,-1.46160199872145,
-1.45371801381501,-1.4443719545512,-1.4054864659731,-1.38487674877509,-1.37876788363224,
-1.37474939765288,-1.36899841169059,-1.35476317763241,-1.32283037891195,
-1.30454812183421,-1.29563417016638,-1.28784056555371,-1.27742929934751,
-1.25336736896966,-1.22948832239679,-1.21652206902214,-1.211065003871,-1.20654778236472,
-1.19958918674502,-1.17700413632658,-1.15277316727466,-1.13670931451525,
-1.12808396368615,-1.12020382988944,-1.11087854057808,-1.10890790056262),
 .UNSPECIFIED.);
#356=B_SPLINE_CURVE_WITH_KNOTS('',3,(#29423,#29424,#29425,#29426,#29427,
#29428,#29429,#29430,#29431,#29432,#29433,#29434,#29435,#29436,#29437,#29438,
#29439,#29440,#29441,#29442,#29443,#29444,#29445,#29446,#29447,#29448,#29449,
#29450,#29451,#29452,#29453,#29454,#29455,#29456,#29457,#29458,#29459,#29460,
#29461,#29462,#29463,#29464,#29465,#29466,#29467,#29468,#29469,#29470,#29471,
#29472,#29473,#29474,#29475,#29476,#29477,#29478,#29479,#29480,#29481,#29482,
#29483,#29484,#29485,#29486,#29487,#29488,#29489,#29490,#29491,#29492,#29493,
#29494,#29495,#29496,#29497,#29498,#29499,#29500,#29501,#29502,#29503,#29504,
#29505,#29506,#29507,#29508,#29509,#29510,#29511,#29512,#29513,#29514,#29515,
#29516,#29517,#29518,#29519,#29520,#29521,#29522,#29523,#29524,#29525,#29526,
#29527,#29528,#29529,#29530,#29531,#29532,#29533,#29534,#29535,#29536,#29537,
#29538,#29539,#29540,#29541,#29542,#29543,#29544,#29545,#29546,#29547,#29548,
#29549,#29550,#29551,#29552,#29553,#29554,#29555,#29556,#29557,#29558,#29559,
#29560),.UNSPECIFIED.,.F.,.F.,(4,2,2,2,2,2,2,2,2,2,2,2,2,2,2,2,2,2,2,2,
2,2,2,2,2,2,2,2,2,2,2,2,2,2,2,2,2,2,2,2,2,2,2,2,2,2,2,2,2,2,2,2,2,2,2,2,
2,2,2,2,2,2,2,2,2,2,2,2,4),(-0.991433053737511,-0.977337473195815,-0.970260427033518,
-0.965731400384691,-0.960340191712212,-0.947871567324226,-0.925756726093449,
-0.899550892131357,-0.889012428469617,-0.881208946363963,-0.872368111299795,
-0.854642934878591,-0.824922087795449,-0.808102337432252,-0.802259230694242,
-0.797807958152794,-0.791593169296394,-0.767930537438954,-0.731774736881957,
-0.721763989333825,-0.713991396496742,-0.704949329826644,-0.68556844250453,
-0.648247985382728,-0.63868331559613,-0.633735303879916,-0.628985330485743,
-0.620544831051483,-0.608949905838288,-0.563842929072849,-0.554177962826543,
-0.546428881125405,-0.536981897527955,-0.513266709646065,-0.478873020045048,
-0.470893579663265,-0.466225921200858,-0.461171453087757,-0.450949690624499,
-0.43534485981113,-0.397908716123077,-0.388056142299395,-0.380303253382117,
-0.371171801678835,-0.350914210840861,-0.325483444909963,-0.308043631438932,
-0.302154028897844,-0.297706968658483,-0.291555734644497,-0.269878621440673,
-0.23047302162497,-0.22075162425777,-0.213001903003153,-0.20360740505944,
-0.180558783665135,-0.154770716380689,-0.140725473519647,-0.135006970928188,
-0.13052259975358,-0.123957933809361,-0.11587583906428,-0.0972910383236796,
-0.0662746582505576,-0.055705898203988,-0.0478817462372992,-0.03901320709763,
-0.0278029871581142,-0.000514778870911421),.UNSPECIFIED.);
#357=B_SPLINE_CURVE_WITH_KNOTS('',3,(#29561,#29562,#29563,#29564,#29565,
#29566,#29567),.UNSPECIFIED.,.F.,.F.,(4,3,4),(32.7257487910699,32.9292487870506,
33.0790390540969),.UNSPECIFIED.);
#358=B_SPLINE_CURVE_WITH_KNOTS('',3,(#29568,#29569,#29570,#29571,#29572,
#29573,#29574,#29575,#29576,#29577,#29578,#29579,#29580,#29581,#29582,#29583,
#29584,#29585,#29586,#29587,#29588,#29589,#29590,#29591,#29592,#29593,#29594,
#29595,#29596,#29597,#29598,#29599,#29600,#29601,#29602,#29603,#29604,#29605,
#29606,#29607,#29608,#29609,#29610,#29611,#29612,#29613,#29614,#29615,#29616,
#29617,#29618,#29619,#29620,#29621,#29622,#29623,#29624,#29625,#29626,#29627,
#29628,#29629,#29630,#29631,#29632,#29633,#29634,#29635,#29636,#29637,#29638,
#29639,#29640,#29641,#29642,#29643,#29644,#29645,#29646,#29647,#29648,#29649,
#29650,#29651,#29652,#29653,#29654,#29655,#29656,#29657,#29658,#29659,#29660,
#29661,#29662,#29663,#29664,#29665,#29666,#29667,#29668,#29669,#29670,#29671,
#29672,#29673,#29674,#29675,#29676,#29677,#29678,#29679,#29680,#29681,#29682,
#29683,#29684,#29685,#29686,#29687,#29688,#29689,#29690,#29691,#29692,#29693,
#29694,#29695,#29696,#29697,#29698,#29699,#29700,#29701,#29702,#29703,#29704,
#29705,#29706,#29707,#29708,#29709,#29710,#29711,#29712,#29713),
 .UNSPECIFIED.,.F.,.F.,(4,2,2,2,2,2,2,2,2,2,2,2,2,2,2,2,2,2,2,2,2,2,2,2,
2,2,2,2,2,2,2,2,2,2,2,2,2,2,2,2,2,2,2,2,2,2,2,2,2,2,2,2,2,2,2,2,2,2,2,2,
2,2,2,2,2,2,2,2,2,2,2,2,4),(-1.10890790056262,-1.08811400786465,-1.06318372338053,
-1.04994021317825,-1.04444326883627,-1.03992947342965,-1.03302212634358,
-1.01224940857337,-0.973994608384534,-0.96412889609262,-0.956366366469846,
-0.947072597747512,-0.925302220732801,-0.899983273449288,-0.884706268315308,
-0.879198964123304,-0.874720431324555,-0.869038138806254,-0.854145446547423,
-0.821608263830272,-0.804072321356126,-0.795248786020499,-0.787429498191781,
-0.77681804710707,-0.754150286556068,-0.719217613508706,-0.712560368572158,
-0.70807520733043,-0.702440706573095,-0.687999386930956,-0.657824106116089,
-0.638567692320855,-0.629385465205663,-0.621615945375873,-0.611603976187643,
-0.600215820083641,-0.576544292565914,-0.553133319059069,-0.546185319417576,
-0.541668318479214,-0.536199473415859,-0.523162722974888,-0.499025961886179,
-0.475264353138502,-0.464868363473715,-0.457070286812277,-0.448133574319588,
-0.429699580583213,-0.39710237357353,-0.383466126319985,-0.37784292645349,
-0.373356313458516,-0.366681667502665,-0.358405928620901,-0.338936199038841,
-0.309142058113764,-0.298510973793431,-0.290689197980293,-0.281874329537709,
-0.264403258376847,-0.235633820083133,-0.217992758262308,-0.2124641790746,
-0.20798318456978,-0.202320139387413,-0.187609849018096,-0.156053362441548,
-0.137688722408426,-0.128760066264379,-0.120960650483311,-0.110549993486284,
-0.0847207655443684,-0.0592711779484536),.UNSPECIFIED.);
#359=B_SPLINE_CURVE_WITH_KNOTS('',3,(#29718,#29719,#29720,#29721,#29722,
#29723,#29724,#29725,#29726,#29727,#29728,#29729,#29730,#29731,#29732,#29733,
#29734,#29735,#29736,#29737,#29738,#29739,#29740,#29741,#29742,#29743,#29744,
#29745,#29746,#29747,#29748,#29749,#29750,#29751,#29752,#29753,#29754,#29755,
#29756,#29757,#29758,#29759,#29760,#29761,#29762,#29763,#29764,#29765,#29766,
#29767,#29768,#29769,#29770,#29771,#29772,#29773,#29774,#29775,#29776,#29777,
#29778,#29779,#29780,#29781,#29782,#29783,#29784,#29785,#29786,#29787,#29788,
#29789,#29790,#29791,#29792,#29793,#29794,#29795,#29796,#29797,#29798,#29799,
#29800,#29801,#29802,#29803,#29804,#29805,#29806,#29807,#29808,#29809,#29810,
#29811,#29812,#29813,#29814,#29815,#29816,#29817,#29818,#29819,#29820,#29821,
#29822,#29823,#29824,#29825,#29826,#29827,#29828,#29829,#29830,#29831,#29832,
#29833,#29834,#29835,#29836,#29837,#29838,#29839,#29840,#29841,#29842,#29843,
#29844,#29845,#29846,#29847,#29848,#29849,#29850,#29851,#29852,#29853,#29854,
#29855,#29856,#29857,#29858,#29859,#29860,#29861,#29862,#29863),
 .UNSPECIFIED.,.F.,.F.,(4,2,2,2,2,2,2,2,2,2,2,2,2,2,2,2,2,2,2,2,2,2,2,2,
2,2,2,2,2,2,2,2,2,2,2,2,2,2,2,2,2,2,2,2,2,2,2,2,2,2,2,2,2,2,2,2,2,2,2,2,
2,2,2,2,2,2,2,2,2,2,2,2,4),(-2.04121419657881,-2.03466850023715,-1.99673483105692,
-1.97563061114487,-1.96950366710435,-1.96505311876075,-1.95912893479973,
-1.94130357244149,-1.91241050598299,-1.89490467746027,-1.88609045027922,
-1.87827899848259,-1.86767963115871,-1.83709734466832,-1.81813557854545,
-1.80997305387442,-1.80336442429608,-1.79888792552053,-1.79323567347023,
-1.77942600076917,-1.74698641198956,-1.72858684331008,-1.71965963253582,
-1.71187019235517,-1.70148838986718,-1.66783377789036,-1.65055046134357,
-1.64277192072265,-1.63638781643952,-1.63192826839746,-1.62621775383506,
-1.61184066976607,-1.58005428931297,-1.56180786107244,-1.55289974187417,
-1.54510730016148,-1.53469157129649,-1.51051515512083,-1.48675015988346,
-1.47381671776211,-1.46836454848299,-1.46385123309717,-1.45689664040709,
-1.42389683982038,-1.40208634430952,-1.3904921613322,-1.38255555364844,
-1.37411856026509,-1.35926141727359,-1.32329440306762,-1.30783293564939,
-1.30209717341356,-1.29763101975112,-1.29114574596063,-1.25980509640235,
-1.23296816746598,-1.22243465905132,-1.21463047561848,-1.2057843620489,
-1.18802610289659,-1.15578223609239,-1.14094886261482,-1.1352763545984,
-1.13080233979671,-1.12422345794836,-1.08878610807526,-1.07166119841832,
-1.05853431663075,-1.05036493253978,-1.04224445103514,-1.02943037548668,
-1.01294627034538,-0.991433053737511),.UNSPECIFIED.);
#360=B_SPLINE_CURVE_WITH_KNOTS('',3,(#29865,#29866,#29867,#29868,#29869,
#29870,#29871,#29872,#29873,#29874,#29875,#29876,#29877,#29878),
 .UNSPECIFIED.,.F.,.F.,(4,2,2,2,2,2,4),(-0.0592711779484536,-0.0517373192803024,
-0.0454235810713492,-0.0409631664080061,-0.0350813863120996,-0.0277951384227308,
-0.000495761613670239),.UNSPECIFIED.);
#361=B_SPLINE_CURVE_WITH_KNOTS('',3,(#29879,#29880,#29881,#29882,#29883,
#29884,#29885,#29886,#29887,#29888,#29889,#29890,#29891,#29892,#29893,#29894,
#29895,#29896,#29897,#29898,#29899,#29900,#29901,#29902,#29903,#29904,#29905,
#29906,#29907,#29908,#29909,#29910,#29911,#29912,#29913,#29914,#29915,#29916,
#29917,#29918,#29919,#29920,#29921,#29922,#29923,#29924,#29925,#29926,#29927,
#29928,#29929,#29930,#29931,#29932,#29933,#29934,#29935,#29936,#29937,#29938,
#29939,#29940,#29941,#29942,#29943,#29944,#29945,#29946,#29947,#29948,#29949,
#29950,#29951,#29952,#29953,#29954,#29955,#29956,#29957,#29958,#29959,#29960,
#29961,#29962,#29963,#29964,#29965,#29966,#29967,#29968,#29969,#29970,#29971,
#29972,#29973,#29974,#29975,#29976,#29977,#29978,#29979,#29980,#29981,#29982,
#29983,#29984,#29985,#29986,#29987,#29988,#29989,#29990,#29991,#29992,#29993,
#29994,#29995,#29996,#29997,#29998,#29999,#30000,#30001,#30002,#30003,#30004,
#30005,#30006,#30007,#30008,#30009,#30010,#30011,#30012,#30013,#30014,#30015,
#30016),.UNSPECIFIED.,.F.,.F.,(4,2,2,2,2,2,2,2,2,2,2,2,2,2,2,2,2,2,2,2,
2,2,2,2,2,2,2,2,2,2,2,2,2,2,2,2,2,2,2,2,2,2,2,2,2,2,2,2,2,2,2,2,2,2,2,2,
2,2,2,2,2,2,2,2,2,2,2,2,4),(-2.09995567732276,-2.08136011835908,-2.07053665316555,
-2.06158601273293,-2.05378969108546,-2.04360051766163,-2.01015146619416,
-1.98437054469011,-1.97811554025164,-1.97365723714953,-1.96783013784949,
-1.9515564402826,-1.92541936142596,-1.90465052046543,-1.8954529777995,-1.88768543248497,
-1.87786519525954,-1.8401322124454,-1.81750972601926,-1.81132166147492,
-1.80686515424378,-1.80098042609273,-1.7857588514941,-1.75491562200284,
-1.73689583871495,-1.72800966091386,-1.72020199951066,-1.70971066915749,
-1.67726454538687,-1.65096600352949,-1.64470612746598,-1.64024757279835,
-1.63442429985572,-1.61939784692932,-1.58830100529951,-1.57021851111152,
-1.561324552486,-1.5535185049408,-1.54304238166541,-1.51040648934652,-1.4851281413965,
-1.47846905065918,-1.47398367726841,-1.46835032329901,-1.45528241327861,
-1.42224637658264,-1.40371019162329,-1.39476055023921,-1.38696457802254,
-1.3765914400719,-1.34280519617554,-1.32559316132554,-1.3178297338326,-1.31145328402773,
-1.3069896735068,-1.30125938958142,-1.28677121863048,-1.25510807035848,
-1.23688904940545,-1.22797860606782,-1.22017634457431,-1.20973328775075,
-1.17671553975917,-1.15112688542641,-1.14475626310066,-1.14029309509931,
-1.13455872305219,-1.12004228789955,-1.10908322593535),.UNSPECIFIED.);
#362=B_SPLINE_CURVE_WITH_KNOTS('',3,(#30022,#30023,#30024,#30025,#30026,
#30027,#30028,#30029,#30030,#30031),.UNSPECIFIED.,.F.,.F.,(4,1,1,1,1,1,
1,4),(14.2298304186001,14.9678403577503,15.9656963816003,16.9635524054503,
17.9614084293003,18.9592644531503,19.9571204770003,20.1593781767107),
 .UNSPECIFIED.);
#363=B_SPLINE_CURVE_WITH_KNOTS('',3,(#30032,#30033,#30034,#30035,#30036,
#30037,#30038,#30039,#30040,#30041,#30042,#30043),.UNSPECIFIED.,.F.,.F.,
(4,2,2,2,2,4),(-2.10029956731405,-2.07301378137977,-2.06183096664427,-2.05296432909478,
-2.04516370709654,-2.04121419657881),.UNSPECIFIED.);
#364=B_SPLINE_CURVE_WITH_KNOTS('',3,(#30044,#30045,#30046,#30047,#30048,
#30049,#30050,#30051,#30052,#30053,#30054,#30055,#30056,#30057,#30058,#30059,
#30060,#30061,#30062,#30063,#30064,#30065,#30066,#30067,#30068,#30069,#30070,
#30071,#30072,#30073,#30074,#30075,#30076,#30077,#30078,#30079,#30080,#30081,
#30082,#30083,#30084,#30085,#30086,#30087,#30088,#30089,#30090,#30091,#30092,
#30093,#30094,#30095,#30096,#30097,#30098,#30099,#30100,#30101,#30102,#30103,
#30104,#30105,#30106,#30107,#30108,#30109,#30110,#30111,#30112,#30113,#30114,
#30115,#30116,#30117,#30118,#30119,#30120,#30121,#30122,#30123,#30124,#30125,
#30126,#30127,#30128,#30129,#30130,#30131,#30132,#30133,#30134,#30135,#30136,
#30137,#30138,#30139,#30140,#30141,#30142,#30143,#30144,#30145,#30146,#30147,
#30148,#30149,#30150,#30151,#30152,#30153,#30154,#30155,#30156,#30157,#30158,
#30159,#30160,#30161,#30162,#30163,#30164,#30165,#30166,#30167,#30168,#30169,
#30170,#30171,#30172,#30173,#30174,#30175,#30176,#30177,#30178,#30179,#30180,
#30181,#30182,#30183,#30184,#30185,#30186,#30187,#30188,#30189),
 .UNSPECIFIED.,.F.,.F.,(4,2,2,2,2,2,2,2,2,2,2,2,2,2,2,2,2,2,2,2,2,2,2,2,
2,2,2,2,2,2,2,2,2,2,2,2,2,2,2,2,2,2,2,2,2,2,2,2,2,2,2,2,2,2,2,2,2,2,2,2,
2,2,2,2,2,2,2,2,2,2,2,2,4),(-1.10908322593535,-1.09452357101242,-1.07885078350604,
-1.0664449458177,-1.05838175086237,-1.05012684182069,-1.03648745952744,
-1.01828085964119,-0.98400040133331,-0.977832177048194,-0.973376623572291,
-0.967367964568854,-0.948537902901784,-0.905845993639871,-0.896180508699763,
-0.888426608656805,-0.878967513193345,-0.855124832993121,-0.820323487666477,
-0.812662804933415,-0.808497166747434,-0.803534746221879,-0.793899404845258,
-0.779708753006532,-0.741056059669688,-0.730667222588459,-0.722870919731796,
-0.713932583421837,-0.695476049326578,-0.662770132945483,-0.649248091834972,
-0.643641549608126,-0.639153170494086,-0.632453988480397,-0.608955843683073,
-0.574070435251138,-0.563916717951346,-0.556125229568534,-0.547156900805119,
-0.528452158744065,-0.494616651173478,-0.482463992718098,-0.476898237890252,
-0.47244553617305,-0.46571806331023,-0.440737361566452,-0.407878836719139,
-0.397418838370953,-0.389615546980399,-0.380715651187146,-0.362572536864072,
-0.331206215588982,-0.316462204577392,-0.310692519780951,-0.306231790098015,
-0.299906908412369,-0.292229487452682,-0.275376974235804,-0.2408127995192,
-0.230624915535627,-0.222829372912667,-0.213879344633832,-0.195332863843477,
-0.162229644351655,-0.149311970874657,-0.143671854051328,-0.139188617244332,
-0.13254312814391,-0.124317324947088,-0.105076000220516,-0.074926734187765,
-0.0643064573797544,-0.059535086939838),.UNSPECIFIED.);
#365=B_SPLINE_CURVE_WITH_KNOTS('',3,(#30195,#30196,#30197,#30198,#30199,
#30200,#30201,#30202,#30203,#30204),.UNSPECIFIED.,.F.,.F.,(4,3,3,4),(-4.19978038454387,
-4.00487054183563,-3.99142409540007,-3.84638326369223),.UNSPECIFIED.);
#366=B_SPLINE_CURVE_WITH_KNOTS('',3,(#30206,#30207,#30208,#30209,#30210,
#30211,#30212,#30213,#30214,#30215,#30216,#30217,#30218,#30219,#30220,#30221,
#30222,#30223,#30224,#30225,#30226,#30227,#30228,#30229,#30230,#30231,#30232,
#30233,#30234,#30235,#30236,#30237,#30238,#30239,#30240,#30241,#30242,#30243,
#30244,#30245,#30246,#30247,#30248,#30249,#30250,#30251,#30252,#30253,#30254,
#30255,#30256,#30257,#30258,#30259,#30260,#30261,#30262,#30263,#30264,#30265,
#30266,#30267,#30268,#30269),.UNSPECIFIED.,.F.,.F.,(4,3,3,3,3,3,3,3,3,3,
3,3,3,3,3,3,3,3,3,3,3,4),(-3.84638326322867,-3.65397025968246,-3.46172848296446,
-3.26958860119382,-3.07703096775827,-2.99356807155005,-2.79813514545863,
-2.59752937101898,-2.40253021789293,-2.19912113279648,-1.99571204770004,
-1.80266597681147,-1.60146348857111,-1.40883152145279,-1.2161658177683,
-1.02299676263876,-0.99785602385002,-0.797266138461779,-0.597138004075606,
-0.397325262770041,-0.197379540394573,0.),.UNSPECIFIED.);
#367=B_SPLINE_CURVE_WITH_KNOTS('',3,(#30273,#30274,#30275,#30276,#30277,
#30278,#30279,#30280,#30281,#30282,#30283,#30284,#30285,#30286,#30287,#30288,
#30289,#30290,#30291,#30292,#30293,#30294,#30295,#30296,#30297,#30298,#30299,
#30300,#30301,#30302,#30303,#30304,#30305,#30306,#30307,#30308,#30309,#30310,
#30311,#30312,#30313,#30314,#30315,#30316,#30317,#30318,#30319,#30320,#30321,
#30322,#30323,#30324,#30325,#30326,#30327,#30328,#30329,#30330,#30331,#30332,
#30333,#30334,#30335,#30336,#30337,#30338,#30339,#30340,#30341,#30342,#30343,
#30344,#30345,#30346,#30347,#30348,#30349,#30350,#30351,#30352,#30353,#30354,
#30355,#30356,#30357),.UNSPECIFIED.,.F.,.F.,(4,3,3,3,3,3,3,3,3,3,3,3,3,
3,3,3,3,3,3,3,3,3,3,3,3,3,3,3,4),(2.01461730579157,2.20940053805023,2.40544242142519,
2.59977896966128,2.79667352060566,2.99356807155005,3.18907181874155,3.38965988790618,
3.58473914322286,3.78808161931147,3.99142409540007,4.18631859471067,4.38705897584553,
4.58149457188408,4.78538734556708,4.98928011925009,5.1844968224971,5.38515665264785,
5.57992515679133,5.78353064994571,5.9871361431001,6.18233678227411,6.38300062844312,
6.57775624002241,6.78137420348627,6.98499216695013,7.18245932510578,7.38773344372867,
7.59300756235157),.UNSPECIFIED.);
#368=B_SPLINE_CURVE_WITH_KNOTS('',3,(#30358,#30359,#30360,#30361,#30362,
#30363,#30364),.UNSPECIFIED.,.F.,.F.,(4,3,4),(7.59300756271701,7.81029936589963,
7.94551948382001),.UNSPECIFIED.);
#369=B_SPLINE_CURVE_WITH_KNOTS('',3,(#30367,#30368,#30369,#30370,#30371,
#30372,#30373,#30374,#30375,#30376,#30377,#30378,#30379,#30380,#30381,#30382,
#30383,#30384,#30385,#30386,#30387,#30388,#30389,#30390,#30391,#30392,#30393,
#30394,#30395,#30396,#30397,#30398,#30399,#30400,#30401,#30402,#30403,#30404,
#30405,#30406,#30407,#30408,#30409,#30410,#30411,#30412,#30413,#30414,#30415,
#30416,#30417,#30418,#30419,#30420,#30421,#30422,#30423,#30424,#30425,#30426,
#30427,#30428,#30429,#30430,#30431,#30432,#30433,#30434,#30435,#30436,#30437,
#30438,#30439,#30440,#30441,#30442,#30443,#30444,#30445,#30446,#30447,#30448,
#30449,#30450,#30451,#30452,#30453,#30454,#30455,#30456,#30457,#30458,#30459,
#30460),.UNSPECIFIED.,.F.,.F.,(4,3,3,3,3,3,3,3,3,3,3,3,3,3,3,3,3,3,3,3,
3,3,3,3,3,3,3,3,3,3,3,4),(7.94551948382001,7.98284819080014,8.17801888453478,
8.37869021706362,8.57341294492868,8.77705857978941,8.98070421465015,9.17586858267023,
9.37654149662772,9.57125816316011,9.77490920083014,9.97856023850017,10.1737145962393,
10.374390012767,10.569096013294,10.7727561378221,10.9764162623502,11.1715780438284,
11.3722516044214,11.5669653285368,11.7706188073685,11.9742722862002,12.169432598189,
12.3701065261543,12.5648187904311,12.7684735502406,12.9721283100502,13.1649388907362,
13.3574741832482,13.5498287982422,13.7425729885002,13.8761925898232),
 .UNSPECIFIED.);
#370=B_SPLINE_CURVE_WITH_KNOTS('',3,(#30461,#30462,#30463,#30464,#30465),
 .UNSPECIFIED.,.F.,.F.,(4,1,4),(13.8761928695312,13.9699843339002,14.2298304186001),
 .UNSPECIFIED.);
#371=B_SPLINE_CURVE_WITH_KNOTS('',3,(#30467,#30468,#30469,#30470,#30471,
#30472,#30473,#30474,#30475,#30476),.UNSPECIFIED.,.F.,.F.,(4,2,2,2,4),(-0.059535086939838,
-0.0564873878884514,-0.0476707125610788,-0.0301752185997041,-0.000496026846082839),
 .UNSPECIFIED.);
#372=B_SPLINE_CURVE_WITH_KNOTS('',3,(#30477,#30478,#30479,#30480,#30481,
#30482,#30483,#30484,#30485,#30486,#30487,#30488,#30489,#30490,#30491,#30492,
#30493,#30494,#30495,#30496,#30497,#30498,#30499,#30500,#30501,#30502,#30503,
#30504,#30505,#30506,#30507,#30508,#30509,#30510,#30511,#30512,#30513,#30514,
#30515,#30516,#30517,#30518,#30519,#30520,#30521,#30522,#30523,#30524,#30525,
#30526,#30527,#30528,#30529,#30530,#30531,#30532,#30533,#30534,#30535,#30536,
#30537,#30538,#30539,#30540,#30541,#30542,#30543,#30544,#30545,#30546,#30547,
#30548,#30549,#30550,#30551,#30552,#30553,#30554,#30555,#30556,#30557,#30558,
#30559,#30560,#30561,#30562,#30563,#30564,#30565,#30566,#30567),
 .UNSPECIFIED.,.F.,.F.,(4,3,3,3,3,3,3,3,3,3,3,3,3,3,3,3,3,3,3,3,3,3,3,3,
3,3,3,3,3,3,4),(-10.1295685708718,-9.97856023850017,-9.78339530381815,-9.58272253152615,
-9.38800594878533,-9.18435508171774,-8.98070421465016,-8.78553363511177,
-8.58486227403386,-8.39013959387681,-8.18649389233848,-7.98284819080014,
-7.78772887232996,-7.587044695985,-7.39237295372156,-7.18868256033584,-6.98499216695012,
-6.78978727159251,-6.58912448946941,-6.39436949264541,-6.19075281787275,
-5.9871361431001,-5.79192140739705,-5.59126108536031,-5.39649262078602,
-5.19288637001805,-4.98928011925009,-4.79190518557354,-4.59739735246488,
-4.39858886850438,-4.19978038454387),.UNSPECIFIED.);
#373=B_SPLINE_CURVE_WITH_KNOTS('',3,(#30570,#30571,#30572,#30573,#30574,
#30575,#30576,#30577),.UNSPECIFIED.,.F.,.F.,(4,1,1,1,1,4),(17.9345037532639,
18.8465721712069,19.8444281950569,20.8422842189069,21.8401402427569,21.9911485751285),
 .UNSPECIFIED.);
#374=B_SPLINE_CURVE_WITH_KNOTS('',3,(#30578,#30579,#30580,#30581,#30582,
#30583),.UNSPECIFIED.,.F.,.F.,(4,1,1,4),(21.9911485751285,22.8379962666069,
23.8358522904569,24.2177779943852),.UNSPECIFIED.);
#375=B_SPLINE_CURVE_WITH_KNOTS('',3,(#30585,#30586,#30587,#30588,#30589,
#30590),.UNSPECIFIED.,.F.,.F.,(4,1,1,4),(21.9911485751285,22.3809892035771,
23.3788452274271,24.2163877000371),.UNSPECIFIED.);
#376=B_SPLINE_CURVE_WITH_KNOTS('',3,(#30591,#30592,#30593,#30594,#30595,
#30596,#30597,#30598),.UNSPECIFIED.,.F.,.F.,(4,1,1,1,1,4),(17.9337114285602,
18.389565108177,19.3874211320271,20.3852771558771,21.3831331797271,21.9911485751285),
 .UNSPECIFIED.);
#377=B_SPLINE_CURVE_WITH_KNOTS('',3,(#30763,#30764,#30765,#30766,#30767,
#30768,#30769,#30770,#30771,#30772,#30773,#30774,#30775,#30776,#30777,#30778,
#30779,#30780,#30781,#30782,#30783,#30784,#30785,#30786,#30787,#30788,#30789,
#30790,#30791,#30792,#30793,#30794,#30795,#30796,#30797,#30798,#30799,#30800,
#30801,#30802,#30803,#30804,#30805,#30806,#30807,#30808,#30809,#30810,#30811,
#30812,#30813,#30814),.UNSPECIFIED.,.F.,.F.,(4,3,3,3,3,3,3,3,3,3,3,3,3,
3,3,3,3,4),(0.,0.0396840521457091,0.0636437457144271,0.0792335113002467,
0.0944204906890096,0.132954435400309,0.150798681725158,0.164378967463246,
0.197217246712606,0.224559338868837,0.23844204002927,0.272690357598131,
0.292926531995206,0.308438743578011,0.33189942988077,0.349623021968201,
0.375435310304714,0.378621596831395),.UNSPECIFIED.);
#378=B_SPLINE_CURVE_WITH_KNOTS('',3,(#30815,#30816,#30817,#30818,#30819,
#30820,#30821,#30822,#30823,#30824,#30825,#30826,#30827,#30828,#30829,#30830,
#30831,#30832,#30833,#30834,#30835,#30836,#30837,#30838,#30839,#30840,#30841,
#30842,#30843,#30844,#30845,#30846,#30847,#30848,#30849,#30850,#30851,#30852,
#30853,#30854,#30855,#30856,#30857,#30858,#30859,#30860,#30861,#30862,#30863),
 .UNSPECIFIED.,.F.,.F.,(4,3,3,3,3,3,3,3,3,3,3,3,3,3,3,3,4),(0.,0.0336993562020884,
0.058720674885152,0.0749541916937741,0.111295928345171,0.130052519737085,
0.144860843722413,0.177258566323581,0.196035872055023,0.216652831180755,
0.255754035742724,0.276800562011943,0.29210454494085,0.320718965530381,
0.341188801348946,0.373057649428629,0.376894338948221),.UNSPECIFIED.);
#379=B_SPLINE_CURVE_WITH_KNOTS('',3,(#31028,#31029,#31030,#31031,#31032,
#31033,#31034,#31035,#31036,#31037,#31038,#31039,#31040,#31041,#31042,#31043,
#31044,#31045,#31046,#31047,#31048,#31049,#31050,#31051,#31052,#31053,#31054,
#31055,#31056,#31057,#31058,#31059,#31060,#31061,#31062,#31063,#31064,#31065,
#31066,#31067,#31068,#31069,#31070,#31071,#31072,#31073,#31074,#31075,#31076),
 .UNSPECIFIED.,.F.,.F.,(4,3,3,3,3,3,3,3,3,3,3,3,3,3,3,3,4),(0.,0.0336994181625108,
0.0587206999399412,0.0749542011850698,0.111295952145659,0.130052464675815,
0.144860842330347,0.177258566323583,0.19603586132328,0.216652857487139,
0.255754055472513,0.276800514863678,0.292104375485169,0.32071687926599,
0.341192754041541,0.373057649428634,0.376894335898406),.UNSPECIFIED.);
#380=B_SPLINE_CURVE_WITH_KNOTS('',3,(#31077,#31078,#31079,#31080,#31081,
#31082,#31083,#31084,#31085,#31086,#31087,#31088,#31089,#31090,#31091,#31092,
#31093,#31094,#31095,#31096,#31097,#31098,#31099,#31100,#31101,#31102,#31103,
#31104,#31105,#31106,#31107,#31108,#31109,#31110,#31111,#31112,#31113,#31114,
#31115,#31116,#31117,#31118,#31119,#31120,#31121,#31122,#31123,#31124,#31125,
#31126,#31127,#31128),.UNSPECIFIED.,.F.,.F.,(4,3,3,3,3,3,3,3,3,3,3,3,3,
3,3,3,3,4),(0.,0.0396840879974647,0.0636435323828637,0.0791466588049358,
0.0941437197617132,0.13268566673474,0.150609314840976,0.164286924555333,
0.19721724671262,0.224559319465188,0.238441985208755,0.272690316482752,
0.292926560932525,0.308438754786714,0.331899421631229,0.349622992774256,
0.37543531030474,0.378621596831421),.UNSPECIFIED.);
#381=FACE_BOUND('',#914,.T.);
#382=FACE_BOUND('',#915,.T.);
#383=FACE_BOUND('',#916,.T.);
#384=FACE_BOUND('',#919,.T.);
#385=FACE_BOUND('',#920,.T.);
#386=FACE_BOUND('',#921,.T.);
#387=FACE_BOUND('',#931,.T.);
#388=FACE_BOUND('',#932,.T.);
#389=FACE_BOUND('',#939,.T.);
#390=FACE_BOUND('',#941,.T.);
#391=FACE_BOUND('',#942,.T.);
#392=FACE_BOUND('',#948,.T.);
#393=FACE_BOUND('',#954,.T.);
#394=FACE_BOUND('',#955,.T.);
#395=FACE_BOUND('',#961,.T.);
#396=FACE_BOUND('',#965,.T.);
#397=FACE_BOUND('',#967,.T.);
#398=FACE_BOUND('',#968,.T.);
#399=FACE_BOUND('',#972,.T.);
#400=FACE_BOUND('',#975,.T.);
#401=FACE_BOUND('',#1014,.T.);
#402=FACE_BOUND('',#1021,.T.);
#403=FACE_BOUND('',#1035,.T.);
#404=FACE_BOUND('',#1036,.T.);
#405=FACE_BOUND('',#1037,.T.);
#406=FACE_BOUND('',#1038,.T.);
#407=FACE_BOUND('',#1039,.T.);
#408=FACE_BOUND('',#1040,.T.);
#409=FACE_BOUND('',#1106,.T.);
#410=FACE_BOUND('',#1109,.T.);
#411=FACE_BOUND('',#1128,.T.);
#412=FACE_BOUND('',#1136,.T.);
#413=FACE_BOUND('',#1182,.T.);
#414=FACE_BOUND('',#1183,.T.);
#415=FACE_BOUND('',#1184,.T.);
#416=FACE_BOUND('',#1185,.T.);
#417=CIRCLE('',#5907,1.);
#418=CIRCLE('',#5908,1.);
#419=CIRCLE('',#5911,1.);
#420=CIRCLE('',#5912,1.);
#421=CIRCLE('',#5914,0.225);
#422=CIRCLE('',#5915,0.225);
#423=CIRCLE('',#5917,0.225);
#424=CIRCLE('',#5918,0.225);
#425=CIRCLE('',#5927,0.225000000000001);
#426=CIRCLE('',#5928,0.225000000000001);
#427=CIRCLE('',#5930,0.224999999999994);
#428=CIRCLE('',#5931,0.224999999999994);
#429=CIRCLE('',#5933,0.42);
#430=CIRCLE('',#5935,0.42);
#431=CIRCLE('',#5941,0.4);
#432=CIRCLE('',#5942,0.22);
#433=CIRCLE('',#5944,0.4);
#434=CIRCLE('',#5946,0.22);
#435=CIRCLE('',#5950,0.22);
#436=CIRCLE('',#5951,0.22);
#437=CIRCLE('',#5953,0.4);
#438=CIRCLE('',#5954,0.4);
#439=CIRCLE('',#5960,0.225);
#440=CIRCLE('',#5961,0.225);
#441=CIRCLE('',#5963,0.225);
#442=CIRCLE('',#5964,0.225);
#443=CIRCLE('',#5966,0.42);
#444=CIRCLE('',#5968,0.42);
#445=CIRCLE('',#5972,0.42);
#446=CIRCLE('',#5973,0.42);
#447=CIRCLE('',#5977,0.4);
#448=CIRCLE('',#5978,0.22);
#449=CIRCLE('',#5980,0.22);
#450=CIRCLE('',#5982,0.4);
#451=CIRCLE('',#5989,0.3);
#452=CIRCLE('',#5990,0.2);
#453=CIRCLE('',#5992,0.3);
#454=CIRCLE('',#5994,0.35);
#455=CIRCLE('',#5995,0.2);
#456=CIRCLE('',#5997,0.35);
#457=CIRCLE('',#6010,0.409999999999997);
#458=CIRCLE('',#6011,0.409999999999997);
#459=CIRCLE('',#6014,0.409999999999997);
#460=CIRCLE('',#6015,0.409999999999997);
#461=CIRCLE('',#6018,0.409999999999997);
#462=CIRCLE('',#6019,0.409999999999997);
#463=CIRCLE('',#6022,0.409999999999997);
#464=CIRCLE('',#6023,0.409999999999997);
#465=CIRCLE('',#6026,0.225000000000001);
#466=CIRCLE('',#6027,0.225000000000001);
#467=CIRCLE('',#6029,0.224999999999994);
#468=CIRCLE('',#6030,0.224999999999994);
#469=CIRCLE('',#6091,0.15555);
#470=CIRCLE('',#6126,0.1954);
#471=CIRCLE('',#6127,0.1954);
#472=CIRCLE('',#6129,0.15555);
#473=CIRCLE('',#6138,0.4);
#474=CIRCLE('',#6140,0.4);
#475=CIRCLE('',#6145,0.205475);
#476=CIRCLE('',#6151,0.205475);
#477=CIRCLE('',#6153,0.1666);
#478=CIRCLE('',#6155,0.1666);
#479=CIRCLE('',#6160,0.1666);
#480=CIRCLE('',#6173,0.409999999999997);
#481=CIRCLE('',#6174,0.409999999999997);
#482=CIRCLE('',#6177,0.409999999999997);
#483=CIRCLE('',#6178,0.409999999999997);
#484=CIRCLE('',#6181,0.409999999999997);
#485=CIRCLE('',#6182,0.409999999999997);
#486=CIRCLE('',#6185,0.409999999999997);
#487=CIRCLE('',#6186,0.409999999999997);
#488=CIRCLE('',#6246,0.4);
#489=CIRCLE('',#6247,0.4);
#490=CYLINDRICAL_SURFACE('',#5906,1.);
#491=CYLINDRICAL_SURFACE('',#5910,1.);
#492=CYLINDRICAL_SURFACE('',#5913,0.225);
#493=CYLINDRICAL_SURFACE('',#5916,0.225);
#494=CYLINDRICAL_SURFACE('',#5926,0.225000000000001);
#495=CYLINDRICAL_SURFACE('',#5929,0.224999999999994);
#496=CYLINDRICAL_SURFACE('',#5934,0.42);
#497=CYLINDRICAL_SURFACE('',#5943,0.4);
#498=CYLINDRICAL_SURFACE('',#5945,0.22);
#499=CYLINDRICAL_SURFACE('',#5949,0.22);
#500=CYLINDRICAL_SURFACE('',#5952,0.4);
#501=CYLINDRICAL_SURFACE('',#5959,0.225);
#502=CYLINDRICAL_SURFACE('',#5962,0.225);
#503=CYLINDRICAL_SURFACE('',#5967,0.42);
#504=CYLINDRICAL_SURFACE('',#5971,0.42);
#505=CYLINDRICAL_SURFACE('',#5979,0.22);
#506=CYLINDRICAL_SURFACE('',#5981,0.4);
#507=CYLINDRICAL_SURFACE('',#5991,0.3);
#508=CYLINDRICAL_SURFACE('',#5996,0.35);
#509=CYLINDRICAL_SURFACE('',#5999,0.2);
#510=CYLINDRICAL_SURFACE('',#6009,0.409999999999997);
#511=CYLINDRICAL_SURFACE('',#6013,0.409999999999997);
#512=CYLINDRICAL_SURFACE('',#6017,0.409999999999997);
#513=CYLINDRICAL_SURFACE('',#6021,0.409999999999997);
#514=CYLINDRICAL_SURFACE('',#6025,0.225000000000001);
#515=CYLINDRICAL_SURFACE('',#6028,0.224999999999994);
#516=CYLINDRICAL_SURFACE('',#6090,0.15555);
#517=CYLINDRICAL_SURFACE('',#6092,0.15555);
#518=CYLINDRICAL_SURFACE('',#6093,0.15555);
#519=CYLINDRICAL_SURFACE('',#6094,0.15555);
#520=CYLINDRICAL_SURFACE('',#6095,0.15555);
#521=CYLINDRICAL_SURFACE('',#6096,0.15555);
#522=CYLINDRICAL_SURFACE('',#6097,0.15555);
#523=CYLINDRICAL_SURFACE('',#6098,0.15555);
#524=CYLINDRICAL_SURFACE('',#6099,0.15555);
#525=CYLINDRICAL_SURFACE('',#6100,0.15555);
#526=CYLINDRICAL_SURFACE('',#6101,0.15555);
#527=CYLINDRICAL_SURFACE('',#6102,0.15555);
#528=CYLINDRICAL_SURFACE('',#6103,0.15555);
#529=CYLINDRICAL_SURFACE('',#6104,0.15555);
#530=CYLINDRICAL_SURFACE('',#6105,0.15555);
#531=CYLINDRICAL_SURFACE('',#6106,0.15555);
#532=CYLINDRICAL_SURFACE('',#6107,0.15555);
#533=CYLINDRICAL_SURFACE('',#6108,0.15555);
#534=CYLINDRICAL_SURFACE('',#6109,0.15555);
#535=CYLINDRICAL_SURFACE('',#6110,0.15555);
#536=CYLINDRICAL_SURFACE('',#6111,0.15555);
#537=CYLINDRICAL_SURFACE('',#6112,0.15555);
#538=CYLINDRICAL_SURFACE('',#6113,0.15555);
#539=CYLINDRICAL_SURFACE('',#6114,0.15555);
#540=CYLINDRICAL_SURFACE('',#6115,0.15555);
#541=CYLINDRICAL_SURFACE('',#6116,0.15555);
#542=CYLINDRICAL_SURFACE('',#6117,0.15555);
#543=CYLINDRICAL_SURFACE('',#6118,0.15555);
#544=CYLINDRICAL_SURFACE('',#6119,0.15555);
#545=CYLINDRICAL_SURFACE('',#6120,0.15555);
#546=CYLINDRICAL_SURFACE('',#6121,0.15555);
#547=CYLINDRICAL_SURFACE('',#6122,0.15555);
#548=CYLINDRICAL_SURFACE('',#6123,0.15555);
#549=CYLINDRICAL_SURFACE('',#6124,0.15555);
#550=CYLINDRICAL_SURFACE('',#6125,0.1954);
#551=CYLINDRICAL_SURFACE('',#6128,0.15555);
#552=CYLINDRICAL_SURFACE('',#6139,0.4);
#553=CYLINDRICAL_SURFACE('',#6144,0.205475);
#554=CYLINDRICAL_SURFACE('',#6146,0.205475);
#555=CYLINDRICAL_SURFACE('',#6147,0.205475);
#556=CYLINDRICAL_SURFACE('',#6148,0.205475);
#557=CYLINDRICAL_SURFACE('',#6149,0.205475);
#558=CYLINDRICAL_SURFACE('',#6150,0.205475);
#559=CYLINDRICAL_SURFACE('',#6152,0.1666);
#560=CYLINDRICAL_SURFACE('',#6154,0.1666);
#561=CYLINDRICAL_SURFACE('',#6156,0.1666);
#562=CYLINDRICAL_SURFACE('',#6157,0.1666);
#563=CYLINDRICAL_SURFACE('',#6158,0.1666);
#564=CYLINDRICAL_SURFACE('',#6159,0.1666);
#565=CYLINDRICAL_SURFACE('',#6161,0.1666);
#566=CYLINDRICAL_SURFACE('',#6162,0.205475);
#567=CYLINDRICAL_SURFACE('',#6172,0.409999999999997);
#568=CYLINDRICAL_SURFACE('',#6176,0.409999999999997);
#569=CYLINDRICAL_SURFACE('',#6180,0.409999999999997);
#570=CYLINDRICAL_SURFACE('',#6184,0.409999999999997);
#571=CYLINDRICAL_SURFACE('',#6245,0.4);
#572=SHAPE_REPRESENTATION_RELATIONSHIP('SRR','None',#31636,#587);
#573=SHAPE_REPRESENTATION_RELATIONSHIP('SRR','None',#31637,#588);
#574=SHAPE_REPRESENTATION_RELATIONSHIP('SRR','None',#31638,#589);
#575=SHAPE_REPRESENTATION_RELATIONSHIP('SRR','None',#31639,#590);
#576=SHAPE_REPRESENTATION_RELATIONSHIP('SRR','None',#31640,#591);
#577=SHAPE_REPRESENTATION_RELATIONSHIP('SRR','None',#31641,#592);
#578=SHAPE_REPRESENTATION_RELATIONSHIP('SRR','None',#31642,#593);
#579=SHAPE_REPRESENTATION_RELATIONSHIP('SRR','None',#31643,#594);
#580=SHAPE_REPRESENTATION_RELATIONSHIP('SRR','None',#31644,#595);
#581=SHAPE_REPRESENTATION_RELATIONSHIP('SRR','None',#31645,#596);
#582=SHAPE_REPRESENTATION_RELATIONSHIP('SRR','None',#31646,#597);
#583=SHAPE_REPRESENTATION_RELATIONSHIP('SRR','None',#31647,#598);
#584=SHAPE_REPRESENTATION_RELATIONSHIP('SRR','None',#31648,#599);
#585=SHAPE_REPRESENTATION_RELATIONSHIP('SRR','None',#31649,#600);
#586=SHAPE_REPRESENTATION_RELATIONSHIP('SRR','None',#31650,#601);
#587=ADVANCED_BREP_SHAPE_REPRESENTATION('',(#617),#31551);
#588=ADVANCED_BREP_SHAPE_REPRESENTATION('',(#618),#31552);
#589=ADVANCED_BREP_SHAPE_REPRESENTATION('',(#619),#31553);
#590=ADVANCED_BREP_SHAPE_REPRESENTATION('',(#620),#31554);
#591=ADVANCED_BREP_SHAPE_REPRESENTATION('',(#621),#31555);
#592=ADVANCED_BREP_SHAPE_REPRESENTATION('',(#622),#31556);
#593=ADVANCED_BREP_SHAPE_REPRESENTATION('',(#623),#31557);
#594=ADVANCED_BREP_SHAPE_REPRESENTATION('',(#624),#31558);
#595=ADVANCED_BREP_SHAPE_REPRESENTATION('',(#625),#31559);
#596=ADVANCED_BREP_SHAPE_REPRESENTATION('',(#626),#31560);
#597=ADVANCED_BREP_SHAPE_REPRESENTATION('',(#627),#31561);
#598=ADVANCED_BREP_SHAPE_REPRESENTATION('',(#628),#31562);
#599=ADVANCED_BREP_SHAPE_REPRESENTATION('',(#629),#31563);
#600=ADVANCED_BREP_SHAPE_REPRESENTATION('',(#630),#31564);
#601=ADVANCED_BREP_SHAPE_REPRESENTATION('',(#631),#31565);
#602=STYLED_ITEM('',(#31720),#617);
#603=STYLED_ITEM('',(#31721),#618);
#604=STYLED_ITEM('',(#31720),#619);
#605=STYLED_ITEM('',(#31720),#620);
#606=STYLED_ITEM('',(#31722),#621);
#607=STYLED_ITEM('',(#31720),#622);
#608=STYLED_ITEM('',(#31723),#623);
#609=STYLED_ITEM('',(#31724),#624);
#610=STYLED_ITEM('',(#31721),#625);
#611=STYLED_ITEM('',(#31720),#626);
#612=STYLED_ITEM('',(#31720),#627);
#613=STYLED_ITEM('',(#31723),#628);
#614=STYLED_ITEM('',(#31724),#629);
#615=STYLED_ITEM('',(#31721),#630);
#616=STYLED_ITEM('',(#31725),#631);
#617=MANIFOLD_SOLID_BREP('Body1',#5715);
#618=MANIFOLD_SOLID_BREP('Body1',#5716);
#619=MANIFOLD_SOLID_BREP('Body1',#5717);
#620=MANIFOLD_SOLID_BREP('Body1',#5718);
#621=MANIFOLD_SOLID_BREP('Body1',#5719);
#622=MANIFOLD_SOLID_BREP('Body1',#5720);
#623=MANIFOLD_SOLID_BREP('Body1',#5721);
#624=MANIFOLD_SOLID_BREP('Body1',#5722);
#625=MANIFOLD_SOLID_BREP('Body1',#5723);
#626=MANIFOLD_SOLID_BREP('Body1',#5724);
#627=MANIFOLD_SOLID_BREP('Body1',#5725);
#628=MANIFOLD_SOLID_BREP('Body1',#5726);
#629=MANIFOLD_SOLID_BREP('Body1',#5727);
#630=MANIFOLD_SOLID_BREP('Body1',#5728);
#631=MANIFOLD_SOLID_BREP('Body1',#5729);
#632=FACE_OUTER_BOUND('',#901,.T.);
#633=FACE_OUTER_BOUND('',#902,.T.);
#634=FACE_OUTER_BOUND('',#903,.T.);
#635=FACE_OUTER_BOUND('',#904,.T.);
#636=FACE_OUTER_BOUND('',#905,.T.);
#637=FACE_OUTER_BOUND('',#906,.T.);
#638=FACE_OUTER_BOUND('',#907,.T.);
#639=FACE_OUTER_BOUND('',#908,.T.);
#640=FACE_OUTER_BOUND('',#909,.T.);
#641=FACE_OUTER_BOUND('',#910,.T.);
#642=FACE_OUTER_BOUND('',#911,.T.);
#643=FACE_OUTER_BOUND('',#912,.T.);
#644=FACE_OUTER_BOUND('',#913,.T.);
#645=FACE_OUTER_BOUND('',#917,.T.);
#646=FACE_OUTER_BOUND('',#918,.T.);
#647=FACE_OUTER_BOUND('',#922,.T.);
#648=FACE_OUTER_BOUND('',#923,.T.);
#649=FACE_OUTER_BOUND('',#924,.T.);
#650=FACE_OUTER_BOUND('',#925,.T.);
#651=FACE_OUTER_BOUND('',#926,.T.);
#652=FACE_OUTER_BOUND('',#927,.T.);
#653=FACE_OUTER_BOUND('',#928,.T.);
#654=FACE_OUTER_BOUND('',#929,.T.);
#655=FACE_OUTER_BOUND('',#930,.T.);
#656=FACE_OUTER_BOUND('',#933,.T.);
#657=FACE_OUTER_BOUND('',#934,.T.);
#658=FACE_OUTER_BOUND('',#935,.T.);
#659=FACE_OUTER_BOUND('',#936,.T.);
#660=FACE_OUTER_BOUND('',#937,.T.);
#661=FACE_OUTER_BOUND('',#938,.T.);
#662=FACE_OUTER_BOUND('',#940,.T.);
#663=FACE_OUTER_BOUND('',#943,.T.);
#664=FACE_OUTER_BOUND('',#944,.T.);
#665=FACE_OUTER_BOUND('',#945,.T.);
#666=FACE_OUTER_BOUND('',#946,.T.);
#667=FACE_OUTER_BOUND('',#947,.T.);
#668=FACE_OUTER_BOUND('',#949,.T.);
#669=FACE_OUTER_BOUND('',#950,.T.);
#670=FACE_OUTER_BOUND('',#951,.T.);
#671=FACE_OUTER_BOUND('',#952,.T.);
#672=FACE_OUTER_BOUND('',#953,.T.);
#673=FACE_OUTER_BOUND('',#956,.T.);
#674=FACE_OUTER_BOUND('',#957,.T.);
#675=FACE_OUTER_BOUND('',#958,.T.);
#676=FACE_OUTER_BOUND('',#959,.T.);
#677=FACE_OUTER_BOUND('',#960,.T.);
#678=FACE_OUTER_BOUND('',#962,.T.);
#679=FACE_OUTER_BOUND('',#963,.T.);
#680=FACE_OUTER_BOUND('',#964,.T.);
#681=FACE_OUTER_BOUND('',#966,.T.);
#682=FACE_OUTER_BOUND('',#969,.T.);
#683=FACE_OUTER_BOUND('',#970,.T.);
#684=FACE_OUTER_BOUND('',#971,.T.);
#685=FACE_OUTER_BOUND('',#973,.T.);
#686=FACE_OUTER_BOUND('',#974,.T.);
#687=FACE_OUTER_BOUND('',#976,.T.);
#688=FACE_OUTER_BOUND('',#977,.T.);
#689=FACE_OUTER_BOUND('',#978,.T.);
#690=FACE_OUTER_BOUND('',#979,.T.);
#691=FACE_OUTER_BOUND('',#980,.T.);
#692=FACE_OUTER_BOUND('',#981,.T.);
#693=FACE_OUTER_BOUND('',#982,.T.);
#694=FACE_OUTER_BOUND('',#983,.T.);
#695=FACE_OUTER_BOUND('',#984,.T.);
#696=FACE_OUTER_BOUND('',#985,.T.);
#697=FACE_OUTER_BOUND('',#986,.T.);
#698=FACE_OUTER_BOUND('',#987,.T.);
#699=FACE_OUTER_BOUND('',#988,.T.);
#700=FACE_OUTER_BOUND('',#989,.T.);
#701=FACE_OUTER_BOUND('',#990,.T.);
#702=FACE_OUTER_BOUND('',#991,.T.);
#703=FACE_OUTER_BOUND('',#992,.T.);
#704=FACE_OUTER_BOUND('',#993,.T.);
#705=FACE_OUTER_BOUND('',#994,.T.);
#706=FACE_OUTER_BOUND('',#995,.T.);
#707=FACE_OUTER_BOUND('',#996,.T.);
#708=FACE_OUTER_BOUND('',#997,.T.);
#709=FACE_OUTER_BOUND('',#998,.T.);
#710=FACE_OUTER_BOUND('',#999,.T.);
#711=FACE_OUTER_BOUND('',#1000,.T.);
#712=FACE_OUTER_BOUND('',#1001,.T.);
#713=FACE_OUTER_BOUND('',#1002,.T.);
#714=FACE_OUTER_BOUND('',#1003,.T.);
#715=FACE_OUTER_BOUND('',#1004,.T.);
#716=FACE_OUTER_BOUND('',#1005,.T.);
#717=FACE_OUTER_BOUND('',#1006,.T.);
#718=FACE_OUTER_BOUND('',#1007,.T.);
#719=FACE_OUTER_BOUND('',#1008,.T.);
#720=FACE_OUTER_BOUND('',#1009,.T.);
#721=FACE_OUTER_BOUND('',#1010,.T.);
#722=FACE_OUTER_BOUND('',#1011,.T.);
#723=FACE_OUTER_BOUND('',#1012,.T.);
#724=FACE_OUTER_BOUND('',#1013,.T.);
#725=FACE_OUTER_BOUND('',#1015,.T.);
#726=FACE_OUTER_BOUND('',#1016,.T.);
#727=FACE_OUTER_BOUND('',#1017,.T.);
#728=FACE_OUTER_BOUND('',#1018,.T.);
#729=FACE_OUTER_BOUND('',#1019,.T.);
#730=FACE_OUTER_BOUND('',#1020,.T.);
#731=FACE_OUTER_BOUND('',#1022,.T.);
#732=FACE_OUTER_BOUND('',#1023,.T.);
#733=FACE_OUTER_BOUND('',#1024,.T.);
#734=FACE_OUTER_BOUND('',#1025,.T.);
#735=FACE_OUTER_BOUND('',#1026,.T.);
#736=FACE_OUTER_BOUND('',#1027,.T.);
#737=FACE_OUTER_BOUND('',#1028,.T.);
#738=FACE_OUTER_BOUND('',#1029,.T.);
#739=FACE_OUTER_BOUND('',#1030,.T.);
#740=FACE_OUTER_BOUND('',#1031,.T.);
#741=FACE_OUTER_BOUND('',#1032,.T.);
#742=FACE_OUTER_BOUND('',#1033,.T.);
#743=FACE_OUTER_BOUND('',#1034,.T.);
#744=FACE_OUTER_BOUND('',#1041,.T.);
#745=FACE_OUTER_BOUND('',#1042,.T.);
#746=FACE_OUTER_BOUND('',#1043,.T.);
#747=FACE_OUTER_BOUND('',#1044,.T.);
#748=FACE_OUTER_BOUND('',#1045,.T.);
#749=FACE_OUTER_BOUND('',#1046,.T.);
#750=FACE_OUTER_BOUND('',#1047,.T.);
#751=FACE_OUTER_BOUND('',#1048,.T.);
#752=FACE_OUTER_BOUND('',#1049,.T.);
#753=FACE_OUTER_BOUND('',#1050,.T.);
#754=FACE_OUTER_BOUND('',#1051,.T.);
#755=FACE_OUTER_BOUND('',#1052,.T.);
#756=FACE_OUTER_BOUND('',#1053,.T.);
#757=FACE_OUTER_BOUND('',#1054,.T.);
#758=FACE_OUTER_BOUND('',#1055,.T.);
#759=FACE_OUTER_BOUND('',#1056,.T.);
#760=FACE_OUTER_BOUND('',#1057,.T.);
#761=FACE_OUTER_BOUND('',#1058,.T.);
#762=FACE_OUTER_BOUND('',#1059,.T.);
#763=FACE_OUTER_BOUND('',#1060,.T.);
#764=FACE_OUTER_BOUND('',#1061,.T.);
#765=FACE_OUTER_BOUND('',#1062,.T.);
#766=FACE_OUTER_BOUND('',#1063,.T.);
#767=FACE_OUTER_BOUND('',#1064,.T.);
#768=FACE_OUTER_BOUND('',#1065,.T.);
#769=FACE_OUTER_BOUND('',#1066,.T.);
#770=FACE_OUTER_BOUND('',#1067,.T.);
#771=FACE_OUTER_BOUND('',#1068,.T.);
#772=FACE_OUTER_BOUND('',#1069,.T.);
#773=FACE_OUTER_BOUND('',#1070,.T.);
#774=FACE_OUTER_BOUND('',#1071,.T.);
#775=FACE_OUTER_BOUND('',#1072,.T.);
#776=FACE_OUTER_BOUND('',#1073,.T.);
#777=FACE_OUTER_BOUND('',#1074,.T.);
#778=FACE_OUTER_BOUND('',#1075,.T.);
#779=FACE_OUTER_BOUND('',#1076,.T.);
#780=FACE_OUTER_BOUND('',#1077,.T.);
#781=FACE_OUTER_BOUND('',#1078,.T.);
#782=FACE_OUTER_BOUND('',#1079,.T.);
#783=FACE_OUTER_BOUND('',#1080,.T.);
#784=FACE_OUTER_BOUND('',#1081,.T.);
#785=FACE_OUTER_BOUND('',#1082,.T.);
#786=FACE_OUTER_BOUND('',#1083,.T.);
#787=FACE_OUTER_BOUND('',#1084,.T.);
#788=FACE_OUTER_BOUND('',#1085,.T.);
#789=FACE_OUTER_BOUND('',#1086,.T.);
#790=FACE_OUTER_BOUND('',#1087,.T.);
#791=FACE_OUTER_BOUND('',#1088,.T.);
#792=FACE_OUTER_BOUND('',#1089,.T.);
#793=FACE_OUTER_BOUND('',#1090,.T.);
#794=FACE_OUTER_BOUND('',#1091,.T.);
#795=FACE_OUTER_BOUND('',#1092,.T.);
#796=FACE_OUTER_BOUND('',#1093,.T.);
#797=FACE_OUTER_BOUND('',#1094,.T.);
#798=FACE_OUTER_BOUND('',#1095,.T.);
#799=FACE_OUTER_BOUND('',#1096,.T.);
#800=FACE_OUTER_BOUND('',#1097,.T.);
#801=FACE_OUTER_BOUND('',#1098,.T.);
#802=FACE_OUTER_BOUND('',#1099,.T.);
#803=FACE_OUTER_BOUND('',#1100,.T.);
#804=FACE_OUTER_BOUND('',#1101,.T.);
#805=FACE_OUTER_BOUND('',#1102,.T.);
#806=FACE_OUTER_BOUND('',#1103,.T.);
#807=FACE_OUTER_BOUND('',#1104,.T.);
#808=FACE_OUTER_BOUND('',#1105,.T.);
#809=FACE_OUTER_BOUND('',#1107,.T.);
#810=FACE_OUTER_BOUND('',#1108,.T.);
#811=FACE_OUTER_BOUND('',#1110,.T.);
#812=FACE_OUTER_BOUND('',#1111,.T.);
#813=FACE_OUTER_BOUND('',#1112,.T.);
#814=FACE_OUTER_BOUND('',#1113,.T.);
#815=FACE_OUTER_BOUND('',#1114,.T.);
#816=FACE_OUTER_BOUND('',#1115,.T.);
#817=FACE_OUTER_BOUND('',#1116,.T.);
#818=FACE_OUTER_BOUND('',#1117,.T.);
#819=FACE_OUTER_BOUND('',#1118,.T.);
#820=FACE_OUTER_BOUND('',#1119,.T.);
#821=FACE_OUTER_BOUND('',#1120,.T.);
#822=FACE_OUTER_BOUND('',#1121,.T.);
#823=FACE_OUTER_BOUND('',#1122,.T.);
#824=FACE_OUTER_BOUND('',#1123,.T.);
#825=FACE_OUTER_BOUND('',#1124,.T.);
#826=FACE_OUTER_BOUND('',#1125,.T.);
#827=FACE_OUTER_BOUND('',#1126,.T.);
#828=FACE_OUTER_BOUND('',#1127,.T.);
#829=FACE_OUTER_BOUND('',#1129,.T.);
#830=FACE_OUTER_BOUND('',#1130,.T.);
#831=FACE_OUTER_BOUND('',#1131,.T.);
#832=FACE_OUTER_BOUND('',#1132,.T.);
#833=FACE_OUTER_BOUND('',#1133,.T.);
#834=FACE_OUTER_BOUND('',#1134,.T.);
#835=FACE_OUTER_BOUND('',#1135,.T.);
#836=FACE_OUTER_BOUND('',#1137,.T.);
#837=FACE_OUTER_BOUND('',#1138,.T.);
#838=FACE_OUTER_BOUND('',#1139,.T.);
#839=FACE_OUTER_BOUND('',#1140,.T.);
#840=FACE_OUTER_BOUND('',#1141,.T.);
#841=FACE_OUTER_BOUND('',#1142,.T.);
#842=FACE_OUTER_BOUND('',#1143,.T.);
#843=FACE_OUTER_BOUND('',#1144,.T.);
#844=FACE_OUTER_BOUND('',#1145,.T.);
#845=FACE_OUTER_BOUND('',#1146,.T.);
#846=FACE_OUTER_BOUND('',#1147,.T.);
#847=FACE_OUTER_BOUND('',#1148,.T.);
#848=FACE_OUTER_BOUND('',#1149,.T.);
#849=FACE_OUTER_BOUND('',#1150,.T.);
#850=FACE_OUTER_BOUND('',#1151,.T.);
#851=FACE_OUTER_BOUND('',#1152,.T.);
#852=FACE_OUTER_BOUND('',#1153,.T.);
#853=FACE_OUTER_BOUND('',#1154,.T.);
#854=FACE_OUTER_BOUND('',#1155,.T.);
#855=FACE_OUTER_BOUND('',#1156,.T.);
#856=FACE_OUTER_BOUND('',#1157,.T.);
#857=FACE_OUTER_BOUND('',#1158,.T.);
#858=FACE_OUTER_BOUND('',#1159,.T.);
#859=FACE_OUTER_BOUND('',#1160,.T.);
#860=FACE_OUTER_BOUND('',#1161,.T.);
#861=FACE_OUTER_BOUND('',#1162,.T.);
#862=FACE_OUTER_BOUND('',#1163,.T.);
#863=FACE_OUTER_BOUND('',#1164,.T.);
#864=FACE_OUTER_BOUND('',#1165,.T.);
#865=FACE_OUTER_BOUND('',#1166,.T.);
#866=FACE_OUTER_BOUND('',#1167,.T.);
#867=FACE_OUTER_BOUND('',#1168,.T.);
#868=FACE_OUTER_BOUND('',#1169,.T.);
#869=FACE_OUTER_BOUND('',#1170,.T.);
#870=FACE_OUTER_BOUND('',#1171,.T.);
#871=FACE_OUTER_BOUND('',#1172,.T.);
#872=FACE_OUTER_BOUND('',#1173,.T.);
#873=FACE_OUTER_BOUND('',#1174,.T.);
#874=FACE_OUTER_BOUND('',#1175,.T.);
#875=FACE_OUTER_BOUND('',#1176,.T.);
#876=FACE_OUTER_BOUND('',#1177,.T.);
#877=FACE_OUTER_BOUND('',#1178,.T.);
#878=FACE_OUTER_BOUND('',#1179,.T.);
#879=FACE_OUTER_BOUND('',#1180,.T.);
#880=FACE_OUTER_BOUND('',#1181,.T.);
#881=FACE_OUTER_BOUND('',#1186,.T.);
#882=FACE_OUTER_BOUND('',#1187,.T.);
#883=FACE_OUTER_BOUND('',#1188,.T.);
#884=FACE_OUTER_BOUND('',#1189,.T.);
#885=FACE_OUTER_BOUND('',#1190,.T.);
#886=FACE_OUTER_BOUND('',#1191,.T.);
#887=FACE_OUTER_BOUND('',#1192,.T.);
#888=FACE_OUTER_BOUND('',#1193,.T.);
#889=FACE_OUTER_BOUND('',#1194,.T.);
#890=FACE_OUTER_BOUND('',#1195,.T.);
#891=FACE_OUTER_BOUND('',#1196,.T.);
#892=FACE_OUTER_BOUND('',#1197,.T.);
#893=FACE_OUTER_BOUND('',#1198,.T.);
#894=FACE_OUTER_BOUND('',#1199,.T.);
#895=FACE_OUTER_BOUND('',#1200,.T.);
#896=FACE_OUTER_BOUND('',#1201,.T.);
#897=FACE_OUTER_BOUND('',#1202,.T.);
#898=FACE_OUTER_BOUND('',#1203,.T.);
#899=FACE_OUTER_BOUND('',#1204,.T.);
#900=FACE_OUTER_BOUND('',#1205,.T.);
#901=EDGE_LOOP('',(#3627,#3628,#3629,#3630));
#902=EDGE_LOOP('',(#3631,#3632,#3633,#3634));
#903=EDGE_LOOP('',(#3635,#3636,#3637,#3638));
#904=EDGE_LOOP('',(#3639,#3640,#3641,#3642));
#905=EDGE_LOOP('',(#3643,#3644,#3645,#3646));
#906=EDGE_LOOP('',(#3647,#3648,#3649,#3650));
#907=EDGE_LOOP('',(#3651,#3652,#3653,#3654));
#908=EDGE_LOOP('',(#3655,#3656,#3657,#3658));
#909=EDGE_LOOP('',(#3659,#3660,#3661,#3662));
#910=EDGE_LOOP('',(#3663,#3664,#3665,#3666));
#911=EDGE_LOOP('',(#3667,#3668,#3669,#3670));
#912=EDGE_LOOP('',(#3671,#3672,#3673,#3674));
#913=EDGE_LOOP('',(#3675,#3676,#3677,#3678));
#914=EDGE_LOOP('',(#3679,#3680,#3681,#3682));
#915=EDGE_LOOP('',(#3683));
#916=EDGE_LOOP('',(#3684));
#917=EDGE_LOOP('',(#3685,#3686,#3687,#3688));
#918=EDGE_LOOP('',(#3689,#3690,#3691,#3692));
#919=EDGE_LOOP('',(#3693,#3694,#3695,#3696));
#920=EDGE_LOOP('',(#3697));
#921=EDGE_LOOP('',(#3698));
#922=EDGE_LOOP('',(#3699,#3700,#3701,#3702));
#923=EDGE_LOOP('',(#3703,#3704,#3705,#3706));
#924=EDGE_LOOP('',(#3707,#3708,#3709,#3710));
#925=EDGE_LOOP('',(#3711,#3712,#3713,#3714));
#926=EDGE_LOOP('',(#3715,#3716,#3717,#3718));
#927=EDGE_LOOP('',(#3719,#3720,#3721,#3722));
#928=EDGE_LOOP('',(#3723,#3724,#3725,#3726));
#929=EDGE_LOOP('',(#3727,#3728,#3729,#3730));
#930=EDGE_LOOP('',(#3731,#3732,#3733,#3734,#3735,#3736,#3737,#3738,#3739,
#3740,#3741,#3742));
#931=EDGE_LOOP('',(#3743));
#932=EDGE_LOOP('',(#3744));
#933=EDGE_LOOP('',(#3745,#3746,#3747,#3748,#3749,#3750));
#934=EDGE_LOOP('',(#3751,#3752,#3753,#3754,#3755,#3756));
#935=EDGE_LOOP('',(#3757,#3758,#3759,#3760,#3761));
#936=EDGE_LOOP('',(#3762,#3763,#3764,#3765));
#937=EDGE_LOOP('',(#3766,#3767,#3768,#3769));
#938=EDGE_LOOP('',(#3770,#3771,#3772,#3773));
#939=EDGE_LOOP('',(#3774,#3775,#3776));
#940=EDGE_LOOP('',(#3777,#3778,#3779,#3780,#3781,#3782,#3783,#3784,#3785,
#3786,#3787,#3788,#3789,#3790,#3791,#3792));
#941=EDGE_LOOP('',(#3793));
#942=EDGE_LOOP('',(#3794));
#943=EDGE_LOOP('',(#3795,#3796,#3797,#3798));
#944=EDGE_LOOP('',(#3799,#3800,#3801,#3802));
#945=EDGE_LOOP('',(#3803,#3804,#3805,#3806,#3807));
#946=EDGE_LOOP('',(#3808,#3809,#3810,#3811));
#947=EDGE_LOOP('',(#3812,#3813,#3814,#3815));
#948=EDGE_LOOP('',(#3816,#3817,#3818));
#949=EDGE_LOOP('',(#3819,#3820,#3821,#3822));
#950=EDGE_LOOP('',(#3823,#3824,#3825,#3826));
#951=EDGE_LOOP('',(#3827,#3828,#3829));
#952=EDGE_LOOP('',(#3830,#3831,#3832,#3833));
#953=EDGE_LOOP('',(#3834,#3835,#3836,#3837,#3838,#3839,#3840,#3841,#3842,
#3843,#3844,#3845));
#954=EDGE_LOOP('',(#3846));
#955=EDGE_LOOP('',(#3847));
#956=EDGE_LOOP('',(#3848,#3849,#3850,#3851,#3852,#3853,#3854,#3855,#3856,
#3857,#3858,#3859));
#957=EDGE_LOOP('',(#3860,#3861,#3862,#3863));
#958=EDGE_LOOP('',(#3864,#3865,#3866));
#959=EDGE_LOOP('',(#3867,#3868,#3869,#3870,#3871));
#960=EDGE_LOOP('',(#3872,#3873,#3874));
#961=EDGE_LOOP('',(#3875));
#962=EDGE_LOOP('',(#3876,#3877,#3878,#3879));
#963=EDGE_LOOP('',(#3880,#3881,#3882,#3883));
#964=EDGE_LOOP('',(#3884,#3885,#3886));
#965=EDGE_LOOP('',(#3887));
#966=EDGE_LOOP('',(#3888,#3889,#3890,#3891));
#967=EDGE_LOOP('',(#3892));
#968=EDGE_LOOP('',(#3893));
#969=EDGE_LOOP('',(#3894,#3895,#3896,#3897));
#970=EDGE_LOOP('',(#3898,#3899,#3900,#3901,#3902));
#971=EDGE_LOOP('',(#3903));
#972=EDGE_LOOP('',(#3904));
#973=EDGE_LOOP('',(#3905,#3906,#3907,#3908));
#974=EDGE_LOOP('',(#3909));
#975=EDGE_LOOP('',(#3910));
#976=EDGE_LOOP('',(#3911,#3912,#3913,#3914));
#977=EDGE_LOOP('',(#3915));
#978=EDGE_LOOP('',(#3916,#3917,#3918,#3919));
#979=EDGE_LOOP('',(#3920));
#980=EDGE_LOOP('',(#3921,#3922,#3923,#3924));
#981=EDGE_LOOP('',(#3925,#3926,#3927,#3928));
#982=EDGE_LOOP('',(#3929,#3930,#3931,#3932));
#983=EDGE_LOOP('',(#3933,#3934,#3935,#3936));
#984=EDGE_LOOP('',(#3937,#3938,#3939,#3940));
#985=EDGE_LOOP('',(#3941,#3942,#3943,#3944));
#986=EDGE_LOOP('',(#3945,#3946,#3947,#3948));
#987=EDGE_LOOP('',(#3949));
#988=EDGE_LOOP('',(#3950,#3951,#3952,#3953));
#989=EDGE_LOOP('',(#3954));
#990=EDGE_LOOP('',(#3955,#3956,#3957,#3958));
#991=EDGE_LOOP('',(#3959));
#992=EDGE_LOOP('',(#3960,#3961,#3962,#3963));
#993=EDGE_LOOP('',(#3964));
#994=EDGE_LOOP('',(#3965,#3966,#3967,#3968));
#995=EDGE_LOOP('',(#3969,#3970,#3971,#3972));
#996=EDGE_LOOP('',(#3973,#3974,#3975,#3976));
#997=EDGE_LOOP('',(#3977,#3978,#3979,#3980));
#998=EDGE_LOOP('',(#3981,#3982,#3983,#3984));
#999=EDGE_LOOP('',(#3985,#3986,#3987,#3988));
#1000=EDGE_LOOP('',(#3989,#3990,#3991,#3992));
#1001=EDGE_LOOP('',(#3993,#3994,#3995,#3996));
#1002=EDGE_LOOP('',(#3997,#3998,#3999,#4000));
#1003=EDGE_LOOP('',(#4001,#4002,#4003,#4004));
#1004=EDGE_LOOP('',(#4005,#4006,#4007,#4008,#4009,#4010,#4011,#4012,#4013,
#4014,#4015,#4016,#4017,#4018,#4019,#4020,#4021,#4022,#4023,#4024,#4025,
#4026,#4027,#4028,#4029,#4030,#4031,#4032,#4033,#4034,#4035,#4036,#4037,
#4038,#4039,#4040));
#1005=EDGE_LOOP('',(#4041,#4042,#4043,#4044));
#1006=EDGE_LOOP('',(#4045,#4046,#4047,#4048));
#1007=EDGE_LOOP('',(#4049,#4050,#4051,#4052));
#1008=EDGE_LOOP('',(#4053,#4054,#4055,#4056));
#1009=EDGE_LOOP('',(#4057,#4058,#4059,#4060));
#1010=EDGE_LOOP('',(#4061,#4062,#4063,#4064));
#1011=EDGE_LOOP('',(#4065,#4066,#4067,#4068));
#1012=EDGE_LOOP('',(#4069,#4070,#4071,#4072));
#1013=EDGE_LOOP('',(#4073,#4074,#4075,#4076));
#1014=EDGE_LOOP('',(#4077));
#1015=EDGE_LOOP('',(#4078,#4079,#4080,#4081));
#1016=EDGE_LOOP('',(#4082,#4083,#4084,#4085));
#1017=EDGE_LOOP('',(#4086,#4087,#4088,#4089));
#1018=EDGE_LOOP('',(#4090,#4091,#4092,#4093));
#1019=EDGE_LOOP('',(#4094,#4095,#4096,#4097));
#1020=EDGE_LOOP('',(#4098,#4099,#4100,#4101));
#1021=EDGE_LOOP('',(#4102));
#1022=EDGE_LOOP('',(#4103,#4104,#4105,#4106));
#1023=EDGE_LOOP('',(#4107,#4108,#4109,#4110));
#1024=EDGE_LOOP('',(#4111,#4112,#4113,#4114));
#1025=EDGE_LOOP('',(#4115,#4116,#4117,#4118));
#1026=EDGE_LOOP('',(#4119,#4120,#4121,#4122));
#1027=EDGE_LOOP('',(#4123,#4124,#4125,#4126));
#1028=EDGE_LOOP('',(#4127,#4128,#4129,#4130));
#1029=EDGE_LOOP('',(#4131,#4132,#4133,#4134));
#1030=EDGE_LOOP('',(#4135,#4136,#4137,#4138));
#1031=EDGE_LOOP('',(#4139,#4140,#4141,#4142,#4143,#4144,#4145,#4146,#4147,
#4148,#4149,#4150,#4151,#4152,#4153,#4154,#4155,#4156,#4157,#4158));
#1032=EDGE_LOOP('',(#4159,#4160,#4161,#4162));
#1033=EDGE_LOOP('',(#4163,#4164,#4165,#4166,#4167,#4168,#4169,#4170,#4171,
#4172,#4173,#4174,#4175,#4176,#4177,#4178,#4179,#4180,#4181,#4182));
#1034=EDGE_LOOP('',(#4183,#4184,#4185,#4186));
#1035=EDGE_LOOP('',(#4187));
#1036=EDGE_LOOP('',(#4188));
#1037=EDGE_LOOP('',(#4189));
#1038=EDGE_LOOP('',(#4190));
#1039=EDGE_LOOP('',(#4191));
#1040=EDGE_LOOP('',(#4192));
#1041=EDGE_LOOP('',(#4193,#4194,#4195,#4196));
#1042=EDGE_LOOP('',(#4197,#4198,#4199,#4200));
#1043=EDGE_LOOP('',(#4201,#4202,#4203,#4204));
#1044=EDGE_LOOP('',(#4205,#4206,#4207,#4208));
#1045=EDGE_LOOP('',(#4209,#4210,#4211,#4212,#4213,#4214,#4215,#4216));
#1046=EDGE_LOOP('',(#4217,#4218,#4219,#4220));
#1047=EDGE_LOOP('',(#4221,#4222,#4223,#4224));
#1048=EDGE_LOOP('',(#4225,#4226,#4227,#4228));
#1049=EDGE_LOOP('',(#4229,#4230,#4231,#4232,#4233,#4234,#4235,#4236));
#1050=EDGE_LOOP('',(#4237,#4238,#4239,#4240));
#1051=EDGE_LOOP('',(#4241,#4242,#4243,#4244));
#1052=EDGE_LOOP('',(#4245,#4246,#4247,#4248));
#1053=EDGE_LOOP('',(#4249,#4250,#4251,#4252));
#1054=EDGE_LOOP('',(#4253,#4254,#4255,#4256));
#1055=EDGE_LOOP('',(#4257,#4258,#4259,#4260));
#1056=EDGE_LOOP('',(#4261,#4262,#4263,#4264));
#1057=EDGE_LOOP('',(#4265,#4266,#4267,#4268));
#1058=EDGE_LOOP('',(#4269,#4270,#4271,#4272,#4273,#4274));
#1059=EDGE_LOOP('',(#4275,#4276,#4277,#4278,#4279,#4280));
#1060=EDGE_LOOP('',(#4281,#4282,#4283,#4284));
#1061=EDGE_LOOP('',(#4285,#4286,#4287,#4288,#4289));
#1062=EDGE_LOOP('',(#4290,#4291,#4292,#4293,#4294));
#1063=EDGE_LOOP('',(#4295,#4296,#4297,#4298,#4299));
#1064=EDGE_LOOP('',(#4300,#4301,#4302,#4303,#4304));
#1065=EDGE_LOOP('',(#4305,#4306,#4307,#4308,#4309));
#1066=EDGE_LOOP('',(#4310,#4311,#4312,#4313,#4314,#4315));
#1067=EDGE_LOOP('',(#4316,#4317,#4318,#4319,#4320,#4321));
#1068=EDGE_LOOP('',(#4322,#4323,#4324,#4325,#4326));
#1069=EDGE_LOOP('',(#4327,#4328,#4329,#4330,#4331));
#1070=EDGE_LOOP('',(#4332,#4333,#4334,#4335,#4336));
#1071=EDGE_LOOP('',(#4337,#4338,#4339,#4340,#4341));
#1072=EDGE_LOOP('',(#4342,#4343,#4344,#4345,#4346));
#1073=EDGE_LOOP('',(#4347,#4348,#4349,#4350,#4351));
#1074=EDGE_LOOP('',(#4352,#4353,#4354,#4355,#4356));
#1075=EDGE_LOOP('',(#4357,#4358,#4359,#4360,#4361));
#1076=EDGE_LOOP('',(#4362,#4363,#4364,#4365,#4366));
#1077=EDGE_LOOP('',(#4367,#4368,#4369,#4370,#4371));
#1078=EDGE_LOOP('',(#4372,#4373,#4374,#4375,#4376,#4377));
#1079=EDGE_LOOP('',(#4378,#4379,#4380,#4381,#4382,#4383));
#1080=EDGE_LOOP('',(#4384,#4385,#4386,#4387,#4388));
#1081=EDGE_LOOP('',(#4389,#4390,#4391,#4392,#4393));
#1082=EDGE_LOOP('',(#4394,#4395,#4396,#4397,#4398));
#1083=EDGE_LOOP('',(#4399,#4400,#4401,#4402,#4403));
#1084=EDGE_LOOP('',(#4404,#4405,#4406,#4407,#4408));
#1085=EDGE_LOOP('',(#4409,#4410,#4411,#4412,#4413));
#1086=EDGE_LOOP('',(#4414,#4415,#4416,#4417,#4418));
#1087=EDGE_LOOP('',(#4419,#4420,#4421,#4422,#4423));
#1088=EDGE_LOOP('',(#4424,#4425,#4426,#4427,#4428,#4429));
#1089=EDGE_LOOP('',(#4430,#4431,#4432,#4433));
#1090=EDGE_LOOP('',(#4434,#4435,#4436,#4437,#4438,#4439));
#1091=EDGE_LOOP('',(#4440,#4441,#4442,#4443,#4444));
#1092=EDGE_LOOP('',(#4445,#4446,#4447,#4448,#4449,#4450));
#1093=EDGE_LOOP('',(#4451,#4452,#4453,#4454,#4455));
#1094=EDGE_LOOP('',(#4456,#4457,#4458,#4459,#4460,#4461,#4462,#4463,#4464,
#4465,#4466,#4467,#4468,#4469,#4470,#4471,#4472,#4473,#4474,#4475,#4476,
#4477,#4478,#4479,#4480,#4481,#4482,#4483,#4484,#4485,#4486,#4487,#4488,
#4489,#4490,#4491,#4492,#4493,#4494,#4495,#4496,#4497,#4498,#4499,#4500,
#4501,#4502,#4503,#4504,#4505,#4506,#4507,#4508,#4509,#4510,#4511,#4512,
#4513,#4514,#4515,#4516,#4517,#4518,#4519,#4520,#4521,#4522,#4523,#4524,
#4525,#4526,#4527,#4528));
#1095=EDGE_LOOP('',(#4529,#4530,#4531,#4532,#4533));
#1096=EDGE_LOOP('',(#4534,#4535,#4536,#4537,#4538,#4539,#4540,#4541,#4542,
#4543,#4544,#4545,#4546,#4547,#4548,#4549,#4550,#4551,#4552,#4553,#4554,
#4555,#4556,#4557,#4558,#4559,#4560,#4561,#4562,#4563,#4564,#4565,#4566,
#4567,#4568,#4569,#4570,#4571,#4572,#4573,#4574,#4575,#4576,#4577,#4578,
#4579,#4580,#4581,#4582,#4583,#4584,#4585,#4586,#4587,#4588,#4589,#4590,
#4591,#4592,#4593,#4594,#4595,#4596,#4597,#4598,#4599,#4600,#4601,#4602,
#4603,#4604,#4605,#4606,#4607,#4608,#4609,#4610,#4611,#4612,#4613,#4614,
#4615,#4616,#4617,#4618,#4619,#4620,#4621,#4622,#4623,#4624,#4625,#4626,
#4627));
#1097=EDGE_LOOP('',(#4628,#4629,#4630,#4631,#4632,#4633,#4634,#4635,#4636,
#4637,#4638,#4639,#4640,#4641,#4642,#4643,#4644,#4645,#4646,#4647,#4648,
#4649,#4650,#4651,#4652,#4653,#4654,#4655,#4656,#4657,#4658,#4659,#4660,
#4661,#4662,#4663,#4664,#4665,#4666,#4667,#4668,#4669,#4670,#4671,#4672,
#4673,#4674,#4675,#4676,#4677,#4678,#4679,#4680,#4681,#4682,#4683,#4684,
#4685,#4686,#4687,#4688,#4689,#4690,#4691,#4692,#4693,#4694,#4695,#4696,
#4697,#4698,#4699,#4700,#4701,#4702,#4703,#4704,#4705,#4706,#4707,#4708,
#4709,#4710,#4711,#4712,#4713,#4714,#4715,#4716,#4717,#4718,#4719,#4720));
#1098=EDGE_LOOP('',(#4721,#4722,#4723,#4724));
#1099=EDGE_LOOP('',(#4725,#4726,#4727,#4728));
#1100=EDGE_LOOP('',(#4729,#4730,#4731,#4732));
#1101=EDGE_LOOP('',(#4733,#4734,#4735,#4736));
#1102=EDGE_LOOP('',(#4737,#4738,#4739,#4740));
#1103=EDGE_LOOP('',(#4741,#4742,#4743,#4744));
#1104=EDGE_LOOP('',(#4745,#4746,#4747,#4748,#4749,#4750));
#1105=EDGE_LOOP('',(#4751));
#1106=EDGE_LOOP('',(#4752,#4753,#4754,#4755,#4756));
#1107=EDGE_LOOP('',(#4757,#4758,#4759,#4760));
#1108=EDGE_LOOP('',(#4761));
#1109=EDGE_LOOP('',(#4762,#4763,#4764,#4765,#4766,#4767));
#1110=EDGE_LOOP('',(#4768,#4769,#4770,#4771,#4772));
#1111=EDGE_LOOP('',(#4773,#4774,#4775,#4776));
#1112=EDGE_LOOP('',(#4777,#4778,#4779,#4780,#4781,#4782));
#1113=EDGE_LOOP('',(#4783,#4784,#4785,#4786,#4787,#4788));
#1114=EDGE_LOOP('',(#4789,#4790,#4791,#4792,#4793,#4794));
#1115=EDGE_LOOP('',(#4795,#4796,#4797,#4798,#4799,#4800));
#1116=EDGE_LOOP('',(#4801,#4802,#4803,#4804,#4805,#4806));
#1117=EDGE_LOOP('',(#4807,#4808,#4809));
#1118=EDGE_LOOP('',(#4810,#4811,#4812,#4813,#4814,#4815));
#1119=EDGE_LOOP('',(#4816,#4817,#4818,#4819,#4820));
#1120=EDGE_LOOP('',(#4821,#4822,#4823,#4824,#4825));
#1121=EDGE_LOOP('',(#4826,#4827,#4828,#4829,#4830));
#1122=EDGE_LOOP('',(#4831,#4832,#4833,#4834,#4835,#4836));
#1123=EDGE_LOOP('',(#4837,#4838,#4839,#4840,#4841,#4842));
#1124=EDGE_LOOP('',(#4843,#4844,#4845,#4846,#4847,#4848));
#1125=EDGE_LOOP('',(#4849,#4850,#4851,#4852,#4853,#4854,#4855,#4856,#4857,
#4858,#4859,#4860,#4861,#4862,#4863,#4864,#4865,#4866,#4867,#4868,#4869,
#4870,#4871,#4872,#4873,#4874));
#1126=EDGE_LOOP('',(#4875,#4876,#4877,#4878,#4879,#4880,#4881,#4882,#4883,
#4884,#4885,#4886,#4887,#4888,#4889,#4890,#4891,#4892,#4893,#4894,#4895,
#4896,#4897,#4898,#4899));
#1127=EDGE_LOOP('',(#4900,#4901,#4902,#4903,#4904,#4905));
#1128=EDGE_LOOP('',(#4906,#4907,#4908,#4909));
#1129=EDGE_LOOP('',(#4910,#4911,#4912,#4913));
#1130=EDGE_LOOP('',(#4914,#4915,#4916,#4917));
#1131=EDGE_LOOP('',(#4918,#4919,#4920,#4921));
#1132=EDGE_LOOP('',(#4922,#4923,#4924,#4925));
#1133=EDGE_LOOP('',(#4926,#4927,#4928,#4929));
#1134=EDGE_LOOP('',(#4930,#4931,#4932,#4933));
#1135=EDGE_LOOP('',(#4934,#4935,#4936,#4937,#4938,#4939));
#1136=EDGE_LOOP('',(#4940,#4941,#4942,#4943,#4944));
#1137=EDGE_LOOP('',(#4945,#4946,#4947,#4948));
#1138=EDGE_LOOP('',(#4949));
#1139=EDGE_LOOP('',(#4950,#4951,#4952,#4953));
#1140=EDGE_LOOP('',(#4954));
#1141=EDGE_LOOP('',(#4955,#4956,#4957,#4958));
#1142=EDGE_LOOP('',(#4959));
#1143=EDGE_LOOP('',(#4960,#4961,#4962,#4963));
#1144=EDGE_LOOP('',(#4964));
#1145=EDGE_LOOP('',(#4965,#4966,#4967,#4968));
#1146=EDGE_LOOP('',(#4969,#4970,#4971,#4972));
#1147=EDGE_LOOP('',(#4973,#4974,#4975,#4976));
#1148=EDGE_LOOP('',(#4977,#4978,#4979,#4980));
#1149=EDGE_LOOP('',(#4981,#4982,#4983,#4984));
#1150=EDGE_LOOP('',(#4985,#4986,#4987,#4988));
#1151=EDGE_LOOP('',(#4989,#4990,#4991,#4992));
#1152=EDGE_LOOP('',(#4993,#4994,#4995,#4996));
#1153=EDGE_LOOP('',(#4997,#4998,#4999,#5000,#5001,#5002,#5003,#5004,#5005,
#5006,#5007,#5008,#5009,#5010,#5011,#5012,#5013,#5014,#5015,#5016,#5017,
#5018,#5019,#5020,#5021,#5022,#5023,#5024,#5025,#5026,#5027,#5028,#5029,
#5030,#5031,#5032));
#1154=EDGE_LOOP('',(#5033,#5034,#5035,#5036));
#1155=EDGE_LOOP('',(#5037,#5038,#5039,#5040));
#1156=EDGE_LOOP('',(#5041,#5042,#5043,#5044));
#1157=EDGE_LOOP('',(#5045,#5046,#5047,#5048));
#1158=EDGE_LOOP('',(#5049,#5050,#5051,#5052));
#1159=EDGE_LOOP('',(#5053,#5054,#5055,#5056));
#1160=EDGE_LOOP('',(#5057,#5058,#5059,#5060));
#1161=EDGE_LOOP('',(#5061,#5062,#5063,#5064));
#1162=EDGE_LOOP('',(#5065,#5066,#5067,#5068));
#1163=EDGE_LOOP('',(#5069,#5070,#5071,#5072));
#1164=EDGE_LOOP('',(#5073,#5074,#5075,#5076));
#1165=EDGE_LOOP('',(#5077,#5078,#5079,#5080));
#1166=EDGE_LOOP('',(#5081,#5082,#5083,#5084));
#1167=EDGE_LOOP('',(#5085,#5086,#5087,#5088));
#1168=EDGE_LOOP('',(#5089,#5090,#5091,#5092));
#1169=EDGE_LOOP('',(#5093,#5094,#5095,#5096));
#1170=EDGE_LOOP('',(#5097,#5098,#5099,#5100));
#1171=EDGE_LOOP('',(#5101,#5102,#5103,#5104));
#1172=EDGE_LOOP('',(#5105,#5106,#5107,#5108));
#1173=EDGE_LOOP('',(#5109,#5110,#5111,#5112));
#1174=EDGE_LOOP('',(#5113,#5114,#5115,#5116));
#1175=EDGE_LOOP('',(#5117,#5118,#5119,#5120));
#1176=EDGE_LOOP('',(#5121,#5122,#5123,#5124));
#1177=EDGE_LOOP('',(#5125,#5126,#5127,#5128));
#1178=EDGE_LOOP('',(#5129,#5130,#5131,#5132,#5133,#5134,#5135,#5136,#5137,
#5138,#5139,#5140,#5141,#5142,#5143,#5144,#5145,#5146,#5147,#5148));
#1179=EDGE_LOOP('',(#5149,#5150,#5151,#5152));
#1180=EDGE_LOOP('',(#5153,#5154,#5155,#5156,#5157,#5158,#5159,#5160,#5161,
#5162,#5163,#5164,#5165,#5166,#5167,#5168,#5169,#5170,#5171,#5172));
#1181=EDGE_LOOP('',(#5173,#5174,#5175,#5176));
#1182=EDGE_LOOP('',(#5177));
#1183=EDGE_LOOP('',(#5178));
#1184=EDGE_LOOP('',(#5179));
#1185=EDGE_LOOP('',(#5180));
#1186=EDGE_LOOP('',(#5181,#5182,#5183,#5184));
#1187=EDGE_LOOP('',(#5185,#5186,#5187,#5188));
#1188=EDGE_LOOP('',(#5189,#5190,#5191,#5192));
#1189=EDGE_LOOP('',(#5193,#5194,#5195,#5196));
#1190=EDGE_LOOP('',(#5197,#5198,#5199,#5200,#5201,#5202,#5203,#5204));
#1191=EDGE_LOOP('',(#5205,#5206,#5207,#5208));
#1192=EDGE_LOOP('',(#5209,#5210,#5211,#5212));
#1193=EDGE_LOOP('',(#5213,#5214,#5215,#5216));
#1194=EDGE_LOOP('',(#5217,#5218,#5219,#5220,#5221,#5222,#5223,#5224));
#1195=EDGE_LOOP('',(#5225,#5226,#5227,#5228));
#1196=EDGE_LOOP('',(#5229,#5230,#5231,#5232));
#1197=EDGE_LOOP('',(#5233,#5234,#5235,#5236));
#1198=EDGE_LOOP('',(#5237,#5238,#5239,#5240));
#1199=EDGE_LOOP('',(#5241,#5242,#5243,#5244));
#1200=EDGE_LOOP('',(#5245,#5246,#5247,#5248));
#1201=EDGE_LOOP('',(#5249,#5250,#5251,#5252));
#1202=EDGE_LOOP('',(#5253,#5254,#5255,#5256));
#1203=EDGE_LOOP('',(#5257,#5258,#5259,#5260));
#1204=EDGE_LOOP('',(#5261));
#1205=EDGE_LOOP('',(#5262));
#1206=LINE('',#7566,#1713);
#1207=LINE('',#7568,#1714);
#1208=LINE('',#7570,#1715);
#1209=LINE('',#7571,#1716);
#1210=LINE('',#7574,#1717);
#1211=LINE('',#7576,#1718);
#1212=LINE('',#7577,#1719);
#1213=LINE('',#7580,#1720);
#1214=LINE('',#7582,#1721);
#1215=LINE('',#7583,#1722);
#1216=LINE('',#7585,#1723);
#1217=LINE('',#7586,#1724);
#1218=LINE('',#7593,#1725);
#1219=LINE('',#7595,#1726);
#1220=LINE('',#7597,#1727);
#1221=LINE('',#7598,#1728);
#1222=LINE('',#7603,#1729);
#1223=LINE('',#7607,#1730);
#1224=LINE('',#7609,#1731);
#1225=LINE('',#7610,#1732);
#1226=LINE('',#7618,#1733);
#1227=LINE('',#7624,#1734);
#1228=LINE('',#7629,#1735);
#1229=LINE('',#7631,#1736);
#1230=LINE('',#7633,#1737);
#1231=LINE('',#7634,#1738);
#1232=LINE('',#7637,#1739);
#1233=LINE('',#7639,#1740);
#1234=LINE('',#7640,#1741);
#1235=LINE('',#7643,#1742);
#1236=LINE('',#7645,#1743);
#1237=LINE('',#7646,#1744);
#1238=LINE('',#7648,#1745);
#1239=LINE('',#7649,#1746);
#1240=LINE('',#7657,#1747);
#1241=LINE('',#7663,#1748);
#1242=LINE('',#7668,#1749);
#1243=LINE('',#7672,#1750);
#1244=LINE('',#7673,#1751);
#1245=LINE('',#7676,#1752);
#1246=LINE('',#7679,#1753);
#1247=LINE('',#7682,#1754);
#1248=LINE('',#7684,#1755);
#1249=LINE('',#7685,#1756);
#1250=LINE('',#7688,#1757);
#1251=LINE('',#7690,#1758);
#1252=LINE('',#7692,#1759);
#1253=LINE('',#7694,#1760);
#1254=LINE('',#7696,#1761);
#1255=LINE('',#7698,#1762);
#1256=LINE('',#7700,#1763);
#1257=LINE('',#7702,#1764);
#1258=LINE('',#7703,#1765);
#1259=LINE('',#7706,#1766);
#1260=LINE('',#7708,#1767);
#1261=LINE('',#7710,#1768);
#1262=LINE('',#7711,#1769);
#1263=LINE('',#7714,#1770);
#1264=LINE('',#7716,#1771);
#1265=LINE('',#7718,#1772);
#1266=LINE('',#7719,#1773);
#1267=LINE('',#7724,#1774);
#1268=LINE('',#7729,#1775);
#1269=LINE('',#7732,#1776);
#1270=LINE('',#7736,#1777);
#1271=LINE('',#7737,#1778);
#1272=LINE('',#7738,#1779);
#1273=LINE('',#7741,#1780);
#1274=LINE('',#7743,#1781);
#1275=LINE('',#7745,#1782);
#1276=LINE('',#7747,#1783);
#1277=LINE('',#7749,#1784);
#1278=LINE('',#7750,#1785);
#1279=LINE('',#7759,#1786);
#1280=LINE('',#7766,#1787);
#1281=LINE('',#7772,#1788);
#1282=LINE('',#7777,#1789);
#1283=LINE('',#7780,#1790);
#1284=LINE('',#7783,#1791);
#1285=LINE('',#7786,#1792);
#1286=LINE('',#7789,#1793);
#1287=LINE('',#7791,#1794);
#1288=LINE('',#7793,#1795);
#1289=LINE('',#7795,#1796);
#1290=LINE('',#7797,#1797);
#1291=LINE('',#7799,#1798);
#1292=LINE('',#7801,#1799);
#1293=LINE('',#7803,#1800);
#1294=LINE('',#7805,#1801);
#1295=LINE('',#7806,#1802);
#1296=LINE('',#7809,#1803);
#1297=LINE('',#7811,#1804);
#1298=LINE('',#7813,#1805);
#1299=LINE('',#7815,#1806);
#1300=LINE('',#7816,#1807);
#1301=LINE('',#7818,#1808);
#1302=LINE('',#7820,#1809);
#1303=LINE('',#7821,#1810);
#1304=LINE('',#7828,#1811);
#1305=LINE('',#7829,#1812);
#1306=LINE('',#7837,#1813);
#1307=LINE('',#7843,#1814);
#1308=LINE('',#7844,#1815);
#1309=LINE('',#7846,#1816);
#1310=LINE('',#7857,#1817);
#1311=LINE('',#7865,#1818);
#1312=LINE('',#7869,#1819);
#1313=LINE('',#7875,#1820);
#1314=LINE('',#7877,#1821);
#1315=LINE('',#7879,#1822);
#1316=LINE('',#7880,#1823);
#1317=LINE('',#7883,#1824);
#1318=LINE('',#7885,#1825);
#1319=LINE('',#7886,#1826);
#1320=LINE('',#7889,#1827);
#1321=LINE('',#7891,#1828);
#1322=LINE('',#7892,#1829);
#1323=LINE('',#7894,#1830);
#1324=LINE('',#7895,#1831);
#1325=LINE('',#7903,#1832);
#1326=LINE('',#7910,#1833);
#1327=LINE('',#7917,#1834);
#1328=LINE('',#7924,#1835);
#1329=LINE('',#7931,#1836);
#1330=LINE('',#7937,#1837);
#1331=LINE('',#7942,#1838);
#1332=LINE('',#7944,#1839);
#1333=LINE('',#7946,#1840);
#1334=LINE('',#7947,#1841);
#1335=LINE('',#7951,#1842);
#1336=LINE('',#7953,#1843);
#1337=LINE('',#7955,#1844);
#1338=LINE('',#7956,#1845);
#1339=LINE('',#7960,#1846);
#1340=LINE('',#7962,#1847);
#1341=LINE('',#7964,#1848);
#1342=LINE('',#7965,#1849);
#1343=LINE('',#7969,#1850);
#1344=LINE('',#7971,#1851);
#1345=LINE('',#7973,#1852);
#1346=LINE('',#7974,#1853);
#1347=LINE('',#7978,#1854);
#1348=LINE('',#7980,#1855);
#1349=LINE('',#7982,#1856);
#1350=LINE('',#7983,#1857);
#1351=LINE('',#7987,#1858);
#1352=LINE('',#7989,#1859);
#1353=LINE('',#7991,#1860);
#1354=LINE('',#7992,#1861);
#1355=LINE('',#7996,#1862);
#1356=LINE('',#7998,#1863);
#1357=LINE('',#8000,#1864);
#1358=LINE('',#8001,#1865);
#1359=LINE('',#8005,#1866);
#1360=LINE('',#8007,#1867);
#1361=LINE('',#8009,#1868);
#1362=LINE('',#8010,#1869);
#1363=LINE('',#8013,#1870);
#1364=LINE('',#8015,#1871);
#1365=LINE('',#8017,#1872);
#1366=LINE('',#8019,#1873);
#1367=LINE('',#8020,#1874);
#1368=LINE('',#8022,#1875);
#1369=LINE('',#8024,#1876);
#1370=LINE('',#8025,#1877);
#1371=LINE('',#8027,#1878);
#1372=LINE('',#8029,#1879);
#1373=LINE('',#8030,#1880);
#1374=LINE('',#8032,#1881);
#1375=LINE('',#8034,#1882);
#1376=LINE('',#8035,#1883);
#1377=LINE('',#8037,#1884);
#1378=LINE('',#8039,#1885);
#1379=LINE('',#8041,#1886);
#1380=LINE('',#8043,#1887);
#1381=LINE('',#8044,#1888);
#1382=LINE('',#8046,#1889);
#1383=LINE('',#8048,#1890);
#1384=LINE('',#8049,#1891);
#1385=LINE('',#8051,#1892);
#1386=LINE('',#8053,#1893);
#1387=LINE('',#8054,#1894);
#1388=LINE('',#8056,#1895);
#1389=LINE('',#8058,#1896);
#1390=LINE('',#8059,#1897);
#1391=LINE('',#8062,#1898);
#1392=LINE('',#8063,#1899);
#1393=LINE('',#8066,#1900);
#1394=LINE('',#8067,#1901);
#1395=LINE('',#8070,#1902);
#1396=LINE('',#8071,#1903);
#1397=LINE('',#8074,#1904);
#1398=LINE('',#8075,#1905);
#1399=LINE('',#8077,#1906);
#1400=LINE('',#8079,#1907);
#1401=LINE('',#8082,#1908);
#1402=LINE('',#8083,#1909);
#1403=LINE('',#8086,#1910);
#1404=LINE('',#8087,#1911);
#1405=LINE('',#8090,#1912);
#1406=LINE('',#8091,#1913);
#1407=LINE('',#8094,#1914);
#1408=LINE('',#8095,#1915);
#1409=LINE('',#8097,#1916);
#1410=LINE('',#8099,#1917);
#1411=LINE('',#8102,#1918);
#1412=LINE('',#8103,#1919);
#1413=LINE('',#8106,#1920);
#1414=LINE('',#8107,#1921);
#1415=LINE('',#8110,#1922);
#1416=LINE('',#8111,#1923);
#1417=LINE('',#8114,#1924);
#1418=LINE('',#8115,#1925);
#1419=LINE('',#8117,#1926);
#1420=LINE('',#8119,#1927);
#1421=LINE('',#8122,#1928);
#1422=LINE('',#8123,#1929);
#1423=LINE('',#8126,#1930);
#1424=LINE('',#8127,#1931);
#1425=LINE('',#8130,#1932);
#1426=LINE('',#8131,#1933);
#1427=LINE('',#8134,#1934);
#1428=LINE('',#8135,#1935);
#1429=LINE('',#8137,#1936);
#1430=LINE('',#8139,#1937);
#1431=LINE('',#8142,#1938);
#1432=LINE('',#8144,#1939);
#1433=LINE('',#8145,#1940);
#1434=LINE('',#8148,#1941);
#1435=LINE('',#8149,#1942);
#1436=LINE('',#8152,#1943);
#1437=LINE('',#8153,#1944);
#1438=LINE('',#8155,#1945);
#1439=LINE('',#8161,#1946);
#1440=LINE('',#8163,#1947);
#1441=LINE('',#8165,#1948);
#1442=LINE('',#8166,#1949);
#1443=LINE('',#8170,#1950);
#1444=LINE('',#8172,#1951);
#1445=LINE('',#8174,#1952);
#1446=LINE('',#8175,#1953);
#1447=LINE('',#8177,#1954);
#1448=LINE('',#8178,#1955);
#1449=LINE('',#8181,#1956);
#1450=LINE('',#8183,#1957);
#1451=LINE('',#8185,#1958);
#1452=LINE('',#8187,#1959);
#1453=LINE('',#8188,#1960);
#1454=LINE('',#8191,#1961);
#1455=LINE('',#8192,#1962);
#1456=LINE('',#8195,#1963);
#1457=LINE('',#8197,#1964);
#1458=LINE('',#8198,#1965);
#1459=LINE('',#8201,#1966);
#1460=LINE('',#8202,#1967);
#1461=LINE('',#8204,#1968);
#1462=LINE('',#8205,#1969);
#1463=LINE('',#8212,#1970);
#1464=LINE('',#8214,#1971);
#1465=LINE('',#8216,#1972);
#1466=LINE('',#8217,#1973);
#1467=LINE('',#8220,#1974);
#1468=LINE('',#8222,#1975);
#1469=LINE('',#8223,#1976);
#1470=LINE('',#8226,#1977);
#1471=LINE('',#8228,#1978);
#1472=LINE('',#8229,#1979);
#1473=LINE('',#8232,#1980);
#1474=LINE('',#8234,#1981);
#1475=LINE('',#8235,#1982);
#1476=LINE('',#8238,#1983);
#1477=LINE('',#8240,#1984);
#1478=LINE('',#8241,#1985);
#1479=LINE('',#8243,#1986);
#1480=LINE('',#8244,#1987);
#1481=LINE('',#8251,#1988);
#1482=LINE('',#8484,#1989);
#1483=LINE('',#8929,#1990);
#1484=LINE('',#9416,#1991);
#1485=LINE('',#9903,#1992);
#1486=LINE('',#10404,#1993);
#1487=LINE('',#10757,#1994);
#1488=LINE('',#10881,#1995);
#1489=LINE('',#11182,#1996);
#1490=LINE('',#11611,#1997);
#1491=LINE('',#12114,#1998);
#1492=LINE('',#12613,#1999);
#1493=LINE('',#13152,#2000);
#1494=LINE('',#13803,#2001);
#1495=LINE('',#14304,#2002);
#1496=LINE('',#14805,#2003);
#1497=LINE('',#15288,#2004);
#1498=LINE('',#15783,#2005);
#1499=LINE('',#16140,#2006);
#1500=LINE('',#16267,#2007);
#1501=LINE('',#16562,#2008);
#1502=LINE('',#17007,#2009);
#1503=LINE('',#17534,#2010);
#1504=LINE('',#18099,#2011);
#1505=LINE('',#18604,#2012);
#1506=LINE('',#19073,#2013);
#1507=LINE('',#19538,#2014);
#1508=LINE('',#20029,#2015);
#1509=LINE('',#20351,#2016);
#1510=LINE('',#20827,#2017);
#1511=LINE('',#21285,#2018);
#1512=LINE('',#21586,#2019);
#1513=LINE('',#21934,#2020);
#1514=LINE('',#22286,#2021);
#1515=LINE('',#28550,#2022);
#1516=LINE('',#28552,#2023);
#1517=LINE('',#28554,#2024);
#1518=LINE('',#28555,#2025);
#1519=LINE('',#28558,#2026);
#1520=LINE('',#28560,#2027);
#1521=LINE('',#28561,#2028);
#1522=LINE('',#28564,#2029);
#1523=LINE('',#28566,#2030);
#1524=LINE('',#28567,#2031);
#1525=LINE('',#28570,#2032);
#1526=LINE('',#28572,#2033);
#1527=LINE('',#28573,#2034);
#1528=LINE('',#28576,#2035);
#1529=LINE('',#28578,#2036);
#1530=LINE('',#28579,#2037);
#1531=LINE('',#28581,#2038);
#1532=LINE('',#28582,#2039);
#1533=LINE('',#28589,#2040);
#1534=LINE('',#28597,#2041);
#1535=LINE('',#28627,#2042);
#1536=LINE('',#28763,#2043);
#1537=LINE('',#28905,#2044);
#1538=LINE('',#29041,#2045);
#1539=LINE('',#29112,#2046);
#1540=LINE('',#29173,#2047);
#1541=LINE('',#29186,#2048);
#1542=LINE('',#29421,#2049);
#1543=LINE('',#29717,#2050);
#1544=LINE('',#30020,#2051);
#1545=LINE('',#30193,#2052);
#1546=LINE('',#31132,#2053);
#1547=LINE('',#31134,#2054);
#1548=LINE('',#31136,#2055);
#1549=LINE('',#31138,#2056);
#1550=LINE('',#31140,#2057);
#1551=LINE('',#31141,#2058);
#1552=LINE('',#31145,#2059);
#1553=LINE('',#31146,#2060);
#1554=LINE('',#31147,#2061);
#1555=LINE('',#31150,#2062);
#1556=LINE('',#31151,#2063);
#1557=LINE('',#31154,#2064);
#1558=LINE('',#31155,#2065);
#1559=LINE('',#31158,#2066);
#1560=LINE('',#31159,#2067);
#1561=LINE('',#31162,#2068);
#1562=LINE('',#31163,#2069);
#1563=LINE('',#31165,#2070);
#1564=LINE('',#31172,#2071);
#1565=LINE('',#31179,#2072);
#1566=LINE('',#31186,#2073);
#1567=LINE('',#31193,#2074);
#1568=LINE('',#31199,#2075);
#1569=LINE('',#31201,#2076);
#1570=LINE('',#31203,#2077);
#1571=LINE('',#31204,#2078);
#1572=LINE('',#31208,#2079);
#1573=LINE('',#31210,#2080);
#1574=LINE('',#31212,#2081);
#1575=LINE('',#31213,#2082);
#1576=LINE('',#31217,#2083);
#1577=LINE('',#31219,#2084);
#1578=LINE('',#31221,#2085);
#1579=LINE('',#31222,#2086);
#1580=LINE('',#31226,#2087);
#1581=LINE('',#31228,#2088);
#1582=LINE('',#31230,#2089);
#1583=LINE('',#31231,#2090);
#1584=LINE('',#31235,#2091);
#1585=LINE('',#31237,#2092);
#1586=LINE('',#31239,#2093);
#1587=LINE('',#31240,#2094);
#1588=LINE('',#31244,#2095);
#1589=LINE('',#31246,#2096);
#1590=LINE('',#31248,#2097);
#1591=LINE('',#31249,#2098);
#1592=LINE('',#31253,#2099);
#1593=LINE('',#31255,#2100);
#1594=LINE('',#31257,#2101);
#1595=LINE('',#31258,#2102);
#1596=LINE('',#31262,#2103);
#1597=LINE('',#31264,#2104);
#1598=LINE('',#31266,#2105);
#1599=LINE('',#31267,#2106);
#1600=LINE('',#31270,#2107);
#1601=LINE('',#31272,#2108);
#1602=LINE('',#31274,#2109);
#1603=LINE('',#31276,#2110);
#1604=LINE('',#31277,#2111);
#1605=LINE('',#31279,#2112);
#1606=LINE('',#31281,#2113);
#1607=LINE('',#31282,#2114);
#1608=LINE('',#31284,#2115);
#1609=LINE('',#31286,#2116);
#1610=LINE('',#31287,#2117);
#1611=LINE('',#31289,#2118);
#1612=LINE('',#31291,#2119);
#1613=LINE('',#31292,#2120);
#1614=LINE('',#31294,#2121);
#1615=LINE('',#31296,#2122);
#1616=LINE('',#31298,#2123);
#1617=LINE('',#31300,#2124);
#1618=LINE('',#31301,#2125);
#1619=LINE('',#31303,#2126);
#1620=LINE('',#31305,#2127);
#1621=LINE('',#31306,#2128);
#1622=LINE('',#31308,#2129);
#1623=LINE('',#31310,#2130);
#1624=LINE('',#31311,#2131);
#1625=LINE('',#31313,#2132);
#1626=LINE('',#31315,#2133);
#1627=LINE('',#31316,#2134);
#1628=LINE('',#31319,#2135);
#1629=LINE('',#31320,#2136);
#1630=LINE('',#31323,#2137);
#1631=LINE('',#31324,#2138);
#1632=LINE('',#31327,#2139);
#1633=LINE('',#31328,#2140);
#1634=LINE('',#31331,#2141);
#1635=LINE('',#31332,#2142);
#1636=LINE('',#31334,#2143);
#1637=LINE('',#31336,#2144);
#1638=LINE('',#31339,#2145);
#1639=LINE('',#31340,#2146);
#1640=LINE('',#31343,#2147);
#1641=LINE('',#31344,#2148);
#1642=LINE('',#31347,#2149);
#1643=LINE('',#31348,#2150);
#1644=LINE('',#31351,#2151);
#1645=LINE('',#31352,#2152);
#1646=LINE('',#31354,#2153);
#1647=LINE('',#31356,#2154);
#1648=LINE('',#31359,#2155);
#1649=LINE('',#31360,#2156);
#1650=LINE('',#31363,#2157);
#1651=LINE('',#31364,#2158);
#1652=LINE('',#31367,#2159);
#1653=LINE('',#31368,#2160);
#1654=LINE('',#31371,#2161);
#1655=LINE('',#31372,#2162);
#1656=LINE('',#31374,#2163);
#1657=LINE('',#31376,#2164);
#1658=LINE('',#31379,#2165);
#1659=LINE('',#31380,#2166);
#1660=LINE('',#31383,#2167);
#1661=LINE('',#31384,#2168);
#1662=LINE('',#31387,#2169);
#1663=LINE('',#31388,#2170);
#1664=LINE('',#31391,#2171);
#1665=LINE('',#31392,#2172);
#1666=LINE('',#31394,#2173);
#1667=LINE('',#31396,#2174);
#1668=LINE('',#31399,#2175);
#1669=LINE('',#31401,#2176);
#1670=LINE('',#31402,#2177);
#1671=LINE('',#31405,#2178);
#1672=LINE('',#31406,#2179);
#1673=LINE('',#31409,#2180);
#1674=LINE('',#31410,#2181);
#1675=LINE('',#31412,#2182);
#1676=LINE('',#31418,#2183);
#1677=LINE('',#31420,#2184);
#1678=LINE('',#31422,#2185);
#1679=LINE('',#31423,#2186);
#1680=LINE('',#31427,#2187);
#1681=LINE('',#31429,#2188);
#1682=LINE('',#31431,#2189);
#1683=LINE('',#31432,#2190);
#1684=LINE('',#31434,#2191);
#1685=LINE('',#31435,#2192);
#1686=LINE('',#31438,#2193);
#1687=LINE('',#31440,#2194);
#1688=LINE('',#31442,#2195);
#1689=LINE('',#31444,#2196);
#1690=LINE('',#31445,#2197);
#1691=LINE('',#31448,#2198);
#1692=LINE('',#31449,#2199);
#1693=LINE('',#31452,#2200);
#1694=LINE('',#31454,#2201);
#1695=LINE('',#31455,#2202);
#1696=LINE('',#31458,#2203);
#1697=LINE('',#31459,#2204);
#1698=LINE('',#31461,#2205);
#1699=LINE('',#31462,#2206);
#1700=LINE('',#31469,#2207);
#1701=LINE('',#31471,#2208);
#1702=LINE('',#31473,#2209);
#1703=LINE('',#31474,#2210);
#1704=LINE('',#31477,#2211);
#1705=LINE('',#31479,#2212);
#1706=LINE('',#31480,#2213);
#1707=LINE('',#31483,#2214);
#1708=LINE('',#31485,#2215);
#1709=LINE('',#31486,#2216);
#1710=LINE('',#31488,#2217);
#1711=LINE('',#31489,#2218);
#1712=LINE('',#31497,#2219);
#1713=VECTOR('',#6288,1.);
#1714=VECTOR('',#6289,1.);
#1715=VECTOR('',#6290,1.);
#1716=VECTOR('',#6291,1.);
#1717=VECTOR('',#6294,1.);
#1718=VECTOR('',#6295,1.);
#1719=VECTOR('',#6296,1.);
#1720=VECTOR('',#6299,1.);
#1721=VECTOR('',#6300,1.);
#1722=VECTOR('',#6301,1.);
#1723=VECTOR('',#6304,1.);
#1724=VECTOR('',#6305,1.);
#1725=VECTOR('',#6314,1.);
#1726=VECTOR('',#6315,1.);
#1727=VECTOR('',#6316,1.);
#1728=VECTOR('',#6317,1.);
#1729=VECTOR('',#6322,1.);
#1730=VECTOR('',#6327,1.);
#1731=VECTOR('',#6328,1.);
#1732=VECTOR('',#6329,1.);
#1733=VECTOR('',#6340,0.225);
#1734=VECTOR('',#6347,0.225);
#1735=VECTOR('',#6352,1.);
#1736=VECTOR('',#6353,1.);
#1737=VECTOR('',#6354,1.);
#1738=VECTOR('',#6355,1.);
#1739=VECTOR('',#6358,1.);
#1740=VECTOR('',#6359,1.);
#1741=VECTOR('',#6360,1.);
#1742=VECTOR('',#6363,1.);
#1743=VECTOR('',#6364,1.);
#1744=VECTOR('',#6365,1.);
#1745=VECTOR('',#6368,1.);
#1746=VECTOR('',#6369,1.);
#1747=VECTOR('',#6380,0.225000000000001);
#1748=VECTOR('',#6387,0.224999999999994);
#1749=VECTOR('',#6392,1.);
#1750=VECTOR('',#6395,1.);
#1751=VECTOR('',#6396,1.);
#1752=VECTOR('',#6399,1.);
#1753=VECTOR('',#6402,1.);
#1754=VECTOR('',#6405,1.);
#1755=VECTOR('',#6406,1.);
#1756=VECTOR('',#6407,1.);
#1757=VECTOR('',#6410,1.);
#1758=VECTOR('',#6411,1.);
#1759=VECTOR('',#6412,1.);
#1760=VECTOR('',#6413,1.);
#1761=VECTOR('',#6414,1.);
#1762=VECTOR('',#6415,1.);
#1763=VECTOR('',#6416,1.);
#1764=VECTOR('',#6417,1.);
#1765=VECTOR('',#6418,1.);
#1766=VECTOR('',#6421,1.);
#1767=VECTOR('',#6422,1.);
#1768=VECTOR('',#6423,1.);
#1769=VECTOR('',#6424,1.);
#1770=VECTOR('',#6427,1.);
#1771=VECTOR('',#6428,1.);
#1772=VECTOR('',#6429,1.);
#1773=VECTOR('',#6430,1.);
#1774=VECTOR('',#6435,1.);
#1775=VECTOR('',#6442,1.);
#1776=VECTOR('',#6445,1.);
#1777=VECTOR('',#6450,1.);
#1778=VECTOR('',#6451,1.);
#1779=VECTOR('',#6452,1.);
#1780=VECTOR('',#6455,1.);
#1781=VECTOR('',#6456,1.);
#1782=VECTOR('',#6457,1.);
#1783=VECTOR('',#6458,1.);
#1784=VECTOR('',#6459,1.);
#1785=VECTOR('',#6460,1.);
#1786=VECTOR('',#6477,1.);
#1787=VECTOR('',#6486,0.225);
#1788=VECTOR('',#6493,0.225);
#1789=VECTOR('',#6498,1.);
#1790=VECTOR('',#6501,1.);
#1791=VECTOR('',#6504,1.);
#1792=VECTOR('',#6507,1.);
#1793=VECTOR('',#6510,1.);
#1794=VECTOR('',#6511,1.);
#1795=VECTOR('',#6512,1.);
#1796=VECTOR('',#6513,1.);
#1797=VECTOR('',#6514,1.);
#1798=VECTOR('',#6515,1.);
#1799=VECTOR('',#6516,1.);
#1800=VECTOR('',#6517,1.);
#1801=VECTOR('',#6518,1.);
#1802=VECTOR('',#6519,1.);
#1803=VECTOR('',#6522,1.);
#1804=VECTOR('',#6523,1.);
#1805=VECTOR('',#6524,1.);
#1806=VECTOR('',#6525,1.);
#1807=VECTOR('',#6526,1.);
#1808=VECTOR('',#6527,1.);
#1809=VECTOR('',#6528,1.);
#1810=VECTOR('',#6529,1.);
#1811=VECTOR('',#6540,1.);
#1812=VECTOR('',#6541,1.);
#1813=VECTOR('',#6552,0.22);
#1814=VECTOR('',#6561,1.);
#1815=VECTOR('',#6562,1.);
#1816=VECTOR('',#6565,1.);
#1817=VECTOR('',#6580,0.3);
#1818=VECTOR('',#6589,0.35);
#1819=VECTOR('',#6596,0.2);
#1820=VECTOR('',#6603,1.);
#1821=VECTOR('',#6604,1.);
#1822=VECTOR('',#6605,1.);
#1823=VECTOR('',#6606,1.);
#1824=VECTOR('',#6609,1.);
#1825=VECTOR('',#6610,1.);
#1826=VECTOR('',#6611,1.);
#1827=VECTOR('',#6614,1.);
#1828=VECTOR('',#6615,1.);
#1829=VECTOR('',#6616,1.);
#1830=VECTOR('',#6619,1.);
#1831=VECTOR('',#6620,1.);
#1832=VECTOR('',#6631,0.409999999999997);
#1833=VECTOR('',#6640,0.409999999999997);
#1834=VECTOR('',#6649,0.409999999999997);
#1835=VECTOR('',#6658,0.409999999999997);
#1836=VECTOR('',#6667,0.225000000000001);
#1837=VECTOR('',#6674,0.224999999999994);
#1838=VECTOR('',#6679,1.);
#1839=VECTOR('',#6680,1.);
#1840=VECTOR('',#6681,1.);
#1841=VECTOR('',#6682,1.);
#1842=VECTOR('',#6685,1.);
#1843=VECTOR('',#6686,1.);
#1844=VECTOR('',#6687,1.);
#1845=VECTOR('',#6688,1.);
#1846=VECTOR('',#6691,1.);
#1847=VECTOR('',#6692,1.);
#1848=VECTOR('',#6693,1.);
#1849=VECTOR('',#6694,1.);
#1850=VECTOR('',#6697,1.);
#1851=VECTOR('',#6698,1.);
#1852=VECTOR('',#6699,1.);
#1853=VECTOR('',#6700,1.);
#1854=VECTOR('',#6703,1.);
#1855=VECTOR('',#6704,1.);
#1856=VECTOR('',#6705,1.);
#1857=VECTOR('',#6706,1.);
#1858=VECTOR('',#6709,1.);
#1859=VECTOR('',#6710,1.);
#1860=VECTOR('',#6711,1.);
#1861=VECTOR('',#6712,1.);
#1862=VECTOR('',#6715,1.);
#1863=VECTOR('',#6716,1.);
#1864=VECTOR('',#6717,1.);
#1865=VECTOR('',#6718,1.);
#1866=VECTOR('',#6721,1.);
#1867=VECTOR('',#6722,1.);
#1868=VECTOR('',#6723,1.);
#1869=VECTOR('',#6724,1.);
#1870=VECTOR('',#6727,1.);
#1871=VECTOR('',#6728,1.);
#1872=VECTOR('',#6729,1.);
#1873=VECTOR('',#6730,1.);
#1874=VECTOR('',#6731,1.);
#1875=VECTOR('',#6732,1.);
#1876=VECTOR('',#6733,1.);
#1877=VECTOR('',#6734,1.);
#1878=VECTOR('',#6735,1.);
#1879=VECTOR('',#6736,1.);
#1880=VECTOR('',#6737,1.);
#1881=VECTOR('',#6738,1.);
#1882=VECTOR('',#6739,1.);
#1883=VECTOR('',#6740,1.);
#1884=VECTOR('',#6741,1.);
#1885=VECTOR('',#6742,1.);
#1886=VECTOR('',#6743,1.);
#1887=VECTOR('',#6744,1.);
#1888=VECTOR('',#6745,1.);
#1889=VECTOR('',#6746,1.);
#1890=VECTOR('',#6747,1.);
#1891=VECTOR('',#6748,1.);
#1892=VECTOR('',#6749,1.);
#1893=VECTOR('',#6750,1.);
#1894=VECTOR('',#6751,1.);
#1895=VECTOR('',#6752,1.);
#1896=VECTOR('',#6753,1.);
#1897=VECTOR('',#6754,1.);
#1898=VECTOR('',#6757,1.);
#1899=VECTOR('',#6758,1.);
#1900=VECTOR('',#6761,1.);
#1901=VECTOR('',#6762,1.);
#1902=VECTOR('',#6765,1.);
#1903=VECTOR('',#6766,1.);
#1904=VECTOR('',#6769,1.);
#1905=VECTOR('',#6770,1.);
#1906=VECTOR('',#6773,1.);
#1907=VECTOR('',#6776,1.);
#1908=VECTOR('',#6779,1.);
#1909=VECTOR('',#6780,1.);
#1910=VECTOR('',#6783,1.);
#1911=VECTOR('',#6784,1.);
#1912=VECTOR('',#6787,1.);
#1913=VECTOR('',#6788,1.);
#1914=VECTOR('',#6791,1.);
#1915=VECTOR('',#6792,1.);
#1916=VECTOR('',#6795,1.);
#1917=VECTOR('',#6798,1.);
#1918=VECTOR('',#6801,1.);
#1919=VECTOR('',#6802,1.);
#1920=VECTOR('',#6805,1.);
#1921=VECTOR('',#6806,1.);
#1922=VECTOR('',#6809,1.);
#1923=VECTOR('',#6810,1.);
#1924=VECTOR('',#6813,1.);
#1925=VECTOR('',#6814,1.);
#1926=VECTOR('',#6817,1.);
#1927=VECTOR('',#6820,1.);
#1928=VECTOR('',#6823,1.);
#1929=VECTOR('',#6824,1.);
#1930=VECTOR('',#6827,1.);
#1931=VECTOR('',#6828,1.);
#1932=VECTOR('',#6831,1.);
#1933=VECTOR('',#6832,1.);
#1934=VECTOR('',#6835,1.);
#1935=VECTOR('',#6836,1.);
#1936=VECTOR('',#6839,1.);
#1937=VECTOR('',#6842,1.);
#1938=VECTOR('',#6845,1.);
#1939=VECTOR('',#6846,1.);
#1940=VECTOR('',#6847,1.);
#1941=VECTOR('',#6850,1.);
#1942=VECTOR('',#6851,1.);
#1943=VECTOR('',#6854,1.);
#1944=VECTOR('',#6855,1.);
#1945=VECTOR('',#6858,1.);
#1946=VECTOR('',#6865,1.);
#1947=VECTOR('',#6866,1.);
#1948=VECTOR('',#6867,1.);
#1949=VECTOR('',#6868,1.);
#1950=VECTOR('',#6871,1.);
#1951=VECTOR('',#6872,1.);
#1952=VECTOR('',#6873,1.);
#1953=VECTOR('',#6874,1.);
#1954=VECTOR('',#6877,1.);
#1955=VECTOR('',#6878,1.);
#1956=VECTOR('',#6881,1.);
#1957=VECTOR('',#6882,1.);
#1958=VECTOR('',#6883,1.);
#1959=VECTOR('',#6884,1.);
#1960=VECTOR('',#6885,1.);
#1961=VECTOR('',#6888,1.);
#1962=VECTOR('',#6889,1.);
#1963=VECTOR('',#6892,1.);
#1964=VECTOR('',#6893,1.);
#1965=VECTOR('',#6894,1.);
#1966=VECTOR('',#6897,1.);
#1967=VECTOR('',#6898,1.);
#1968=VECTOR('',#6901,1.);
#1969=VECTOR('',#6902,1.);
#1970=VECTOR('',#6911,1.);
#1971=VECTOR('',#6912,1.);
#1972=VECTOR('',#6913,1.);
#1973=VECTOR('',#6914,1.);
#1974=VECTOR('',#6917,1.);
#1975=VECTOR('',#6918,1.);
#1976=VECTOR('',#6919,1.);
#1977=VECTOR('',#6922,1.);
#1978=VECTOR('',#6923,1.);
#1979=VECTOR('',#6924,1.);
#1980=VECTOR('',#6927,1.);
#1981=VECTOR('',#6928,1.);
#1982=VECTOR('',#6929,1.);
#1983=VECTOR('',#6932,1.);
#1984=VECTOR('',#6933,1.);
#1985=VECTOR('',#6934,1.);
#1986=VECTOR('',#6937,1.);
#1987=VECTOR('',#6938,1.);
#1988=VECTOR('',#6947,0.15555);
#1989=VECTOR('',#6952,0.15555);
#1990=VECTOR('',#6955,0.15555);
#1991=VECTOR('',#6958,0.15555);
#1992=VECTOR('',#6961,0.15555);
#1993=VECTOR('',#6964,0.15555);
#1994=VECTOR('',#6967,0.15555);
#1995=VECTOR('',#6970,0.15555);
#1996=VECTOR('',#6973,0.15555);
#1997=VECTOR('',#6976,0.15555);
#1998=VECTOR('',#6979,0.15555);
#1999=VECTOR('',#6982,0.15555);
#2000=VECTOR('',#6985,0.15555);
#2001=VECTOR('',#6988,0.15555);
#2002=VECTOR('',#6991,0.15555);
#2003=VECTOR('',#6994,0.15555);
#2004=VECTOR('',#6997,0.15555);
#2005=VECTOR('',#7000,0.15555);
#2006=VECTOR('',#7003,0.15555);
#2007=VECTOR('',#7006,0.15555);
#2008=VECTOR('',#7009,0.15555);
#2009=VECTOR('',#7012,0.15555);
#2010=VECTOR('',#7015,0.15555);
#2011=VECTOR('',#7018,0.15555);
#2012=VECTOR('',#7021,0.15555);
#2013=VECTOR('',#7024,0.15555);
#2014=VECTOR('',#7027,0.15555);
#2015=VECTOR('',#7030,0.15555);
#2016=VECTOR('',#7033,0.15555);
#2017=VECTOR('',#7036,0.15555);
#2018=VECTOR('',#7039,0.15555);
#2019=VECTOR('',#7042,0.15555);
#2020=VECTOR('',#7045,0.15555);
#2021=VECTOR('',#7048,0.15555);
#2022=VECTOR('',#7061,1.);
#2023=VECTOR('',#7062,1.);
#2024=VECTOR('',#7063,1.);
#2025=VECTOR('',#7064,1.);
#2026=VECTOR('',#7067,1.);
#2027=VECTOR('',#7068,1.);
#2028=VECTOR('',#7069,1.);
#2029=VECTOR('',#7072,1.);
#2030=VECTOR('',#7073,1.);
#2031=VECTOR('',#7074,1.);
#2032=VECTOR('',#7077,1.);
#2033=VECTOR('',#7078,1.);
#2034=VECTOR('',#7079,1.);
#2035=VECTOR('',#7082,1.);
#2036=VECTOR('',#7083,1.);
#2037=VECTOR('',#7084,1.);
#2038=VECTOR('',#7087,1.);
#2039=VECTOR('',#7088,1.);
#2040=VECTOR('',#7097,0.4);
#2041=VECTOR('',#7108,0.205475);
#2042=VECTOR('',#7113,0.205475);
#2043=VECTOR('',#7116,0.205475);
#2044=VECTOR('',#7119,0.205475);
#2045=VECTOR('',#7122,0.205475);
#2046=VECTOR('',#7125,0.205475);
#2047=VECTOR('',#7130,0.1666);
#2048=VECTOR('',#7135,0.1666);
#2049=VECTOR('',#7140,0.1666);
#2050=VECTOR('',#7143,0.1666);
#2051=VECTOR('',#7146,0.1666);
#2052=VECTOR('',#7149,0.1666);
#2053=VECTOR('',#7158,1.);
#2054=VECTOR('',#7159,1.);
#2055=VECTOR('',#7160,1.);
#2056=VECTOR('',#7161,1.);
#2057=VECTOR('',#7162,1.);
#2058=VECTOR('',#7163,1.);
#2059=VECTOR('',#7166,1.);
#2060=VECTOR('',#7167,1.);
#2061=VECTOR('',#7168,1.);
#2062=VECTOR('',#7171,1.);
#2063=VECTOR('',#7172,1.);
#2064=VECTOR('',#7175,1.);
#2065=VECTOR('',#7176,1.);
#2066=VECTOR('',#7179,1.);
#2067=VECTOR('',#7180,1.);
#2068=VECTOR('',#7183,1.);
#2069=VECTOR('',#7184,1.);
#2070=VECTOR('',#7187,1.);
#2071=VECTOR('',#7196,0.409999999999997);
#2072=VECTOR('',#7205,0.409999999999997);
#2073=VECTOR('',#7214,0.409999999999997);
#2074=VECTOR('',#7223,0.409999999999997);
#2075=VECTOR('',#7230,1.);
#2076=VECTOR('',#7231,1.);
#2077=VECTOR('',#7232,1.);
#2078=VECTOR('',#7233,1.);
#2079=VECTOR('',#7236,1.);
#2080=VECTOR('',#7237,1.);
#2081=VECTOR('',#7238,1.);
#2082=VECTOR('',#7239,1.);
#2083=VECTOR('',#7242,1.);
#2084=VECTOR('',#7243,1.);
#2085=VECTOR('',#7244,1.);
#2086=VECTOR('',#7245,1.);
#2087=VECTOR('',#7248,1.);
#2088=VECTOR('',#7249,1.);
#2089=VECTOR('',#7250,1.);
#2090=VECTOR('',#7251,1.);
#2091=VECTOR('',#7254,1.);
#2092=VECTOR('',#7255,1.);
#2093=VECTOR('',#7256,1.);
#2094=VECTOR('',#7257,1.);
#2095=VECTOR('',#7260,1.);
#2096=VECTOR('',#7261,1.);
#2097=VECTOR('',#7262,1.);
#2098=VECTOR('',#7263,1.);
#2099=VECTOR('',#7266,1.);
#2100=VECTOR('',#7267,1.);
#2101=VECTOR('',#7268,1.);
#2102=VECTOR('',#7269,1.);
#2103=VECTOR('',#7272,1.);
#2104=VECTOR('',#7273,1.);
#2105=VECTOR('',#7274,1.);
#2106=VECTOR('',#7275,1.);
#2107=VECTOR('',#7278,1.);
#2108=VECTOR('',#7279,1.);
#2109=VECTOR('',#7280,1.);
#2110=VECTOR('',#7281,1.);
#2111=VECTOR('',#7282,1.);
#2112=VECTOR('',#7283,1.);
#2113=VECTOR('',#7284,1.);
#2114=VECTOR('',#7285,1.);
#2115=VECTOR('',#7286,1.);
#2116=VECTOR('',#7287,1.);
#2117=VECTOR('',#7288,1.);
#2118=VECTOR('',#7289,1.);
#2119=VECTOR('',#7290,1.);
#2120=VECTOR('',#7291,1.);
#2121=VECTOR('',#7292,1.);
#2122=VECTOR('',#7293,1.);
#2123=VECTOR('',#7294,1.);
#2124=VECTOR('',#7295,1.);
#2125=VECTOR('',#7296,1.);
#2126=VECTOR('',#7297,1.);
#2127=VECTOR('',#7298,1.);
#2128=VECTOR('',#7299,1.);
#2129=VECTOR('',#7300,1.);
#2130=VECTOR('',#7301,1.);
#2131=VECTOR('',#7302,1.);
#2132=VECTOR('',#7303,1.);
#2133=VECTOR('',#7304,1.);
#2134=VECTOR('',#7305,1.);
#2135=VECTOR('',#7308,1.);
#2136=VECTOR('',#7309,1.);
#2137=VECTOR('',#7312,1.);
#2138=VECTOR('',#7313,1.);
#2139=VECTOR('',#7316,1.);
#2140=VECTOR('',#7317,1.);
#2141=VECTOR('',#7320,1.);
#2142=VECTOR('',#7321,1.);
#2143=VECTOR('',#7324,1.);
#2144=VECTOR('',#7327,1.);
#2145=VECTOR('',#7330,1.);
#2146=VECTOR('',#7331,1.);
#2147=VECTOR('',#7334,1.);
#2148=VECTOR('',#7335,1.);
#2149=VECTOR('',#7338,1.);
#2150=VECTOR('',#7339,1.);
#2151=VECTOR('',#7342,1.);
#2152=VECTOR('',#7343,1.);
#2153=VECTOR('',#7346,1.);
#2154=VECTOR('',#7349,1.);
#2155=VECTOR('',#7352,1.);
#2156=VECTOR('',#7353,1.);
#2157=VECTOR('',#7356,1.);
#2158=VECTOR('',#7357,1.);
#2159=VECTOR('',#7360,1.);
#2160=VECTOR('',#7361,1.);
#2161=VECTOR('',#7364,1.);
#2162=VECTOR('',#7365,1.);
#2163=VECTOR('',#7368,1.);
#2164=VECTOR('',#7371,1.);
#2165=VECTOR('',#7374,1.);
#2166=VECTOR('',#7375,1.);
#2167=VECTOR('',#7378,1.);
#2168=VECTOR('',#7379,1.);
#2169=VECTOR('',#7382,1.);
#2170=VECTOR('',#7383,1.);
#2171=VECTOR('',#7386,1.);
#2172=VECTOR('',#7387,1.);
#2173=VECTOR('',#7390,1.);
#2174=VECTOR('',#7393,1.);
#2175=VECTOR('',#7396,1.);
#2176=VECTOR('',#7397,1.);
#2177=VECTOR('',#7398,1.);
#2178=VECTOR('',#7401,1.);
#2179=VECTOR('',#7402,1.);
#2180=VECTOR('',#7405,1.);
#2181=VECTOR('',#7406,1.);
#2182=VECTOR('',#7409,1.);
#2183=VECTOR('',#7416,1.);
#2184=VECTOR('',#7417,1.);
#2185=VECTOR('',#7418,1.);
#2186=VECTOR('',#7419,1.);
#2187=VECTOR('',#7422,1.);
#2188=VECTOR('',#7423,1.);
#2189=VECTOR('',#7424,1.);
#2190=VECTOR('',#7425,1.);
#2191=VECTOR('',#7428,1.);
#2192=VECTOR('',#7429,1.);
#2193=VECTOR('',#7432,1.);
#2194=VECTOR('',#7433,1.);
#2195=VECTOR('',#7434,1.);
#2196=VECTOR('',#7435,1.);
#2197=VECTOR('',#7436,1.);
#2198=VECTOR('',#7439,1.);
#2199=VECTOR('',#7440,1.);
#2200=VECTOR('',#7443,1.);
#2201=VECTOR('',#7444,1.);
#2202=VECTOR('',#7445,1.);
#2203=VECTOR('',#7448,1.);
#2204=VECTOR('',#7449,1.);
#2205=VECTOR('',#7452,1.);
#2206=VECTOR('',#7453,1.);
#2207=VECTOR('',#7462,1.);
#2208=VECTOR('',#7463,1.);
#2209=VECTOR('',#7464,1.);
#2210=VECTOR('',#7465,1.);
#2211=VECTOR('',#7468,1.);
#2212=VECTOR('',#7469,1.);
#2213=VECTOR('',#7470,1.);
#2214=VECTOR('',#7473,1.);
#2215=VECTOR('',#7474,1.);
#2216=VECTOR('',#7475,1.);
#2217=VECTOR('',#7478,1.);
#2218=VECTOR('',#7479,1.);
#2219=VECTOR('',#7490,0.4);
#2220=VERTEX_POINT('',#7564);
#2221=VERTEX_POINT('',#7565);
#2222=VERTEX_POINT('',#7567);
#2223=VERTEX_POINT('',#7569);
#2224=VERTEX_POINT('',#7573);
#2225=VERTEX_POINT('',#7575);
#2226=VERTEX_POINT('',#7579);
#2227=VERTEX_POINT('',#7581);
#2228=VERTEX_POINT('',#7591);
#2229=VERTEX_POINT('',#7592);
#2230=VERTEX_POINT('',#7594);
#2231=VERTEX_POINT('',#7596);
#2232=VERTEX_POINT('',#7600);
#2233=VERTEX_POINT('',#7602);
#2234=VERTEX_POINT('',#7606);
#2235=VERTEX_POINT('',#7608);
#2236=VERTEX_POINT('',#7615);
#2237=VERTEX_POINT('',#7617);
#2238=VERTEX_POINT('',#7621);
#2239=VERTEX_POINT('',#7623);
#2240=VERTEX_POINT('',#7627);
#2241=VERTEX_POINT('',#7628);
#2242=VERTEX_POINT('',#7630);
#2243=VERTEX_POINT('',#7632);
#2244=VERTEX_POINT('',#7636);
#2245=VERTEX_POINT('',#7638);
#2246=VERTEX_POINT('',#7642);
#2247=VERTEX_POINT('',#7644);
#2248=VERTEX_POINT('',#7654);
#2249=VERTEX_POINT('',#7656);
#2250=VERTEX_POINT('',#7660);
#2251=VERTEX_POINT('',#7662);
#2252=VERTEX_POINT('',#7666);
#2253=VERTEX_POINT('',#7667);
#2254=VERTEX_POINT('',#7669);
#2255=VERTEX_POINT('',#7671);
#2256=VERTEX_POINT('',#7675);
#2257=VERTEX_POINT('',#7677);
#2258=VERTEX_POINT('',#7681);
#2259=VERTEX_POINT('',#7683);
#2260=VERTEX_POINT('',#7687);
#2261=VERTEX_POINT('',#7689);
#2262=VERTEX_POINT('',#7691);
#2263=VERTEX_POINT('',#7693);
#2264=VERTEX_POINT('',#7695);
#2265=VERTEX_POINT('',#7697);
#2266=VERTEX_POINT('',#7699);
#2267=VERTEX_POINT('',#7701);
#2268=VERTEX_POINT('',#7705);
#2269=VERTEX_POINT('',#7707);
#2270=VERTEX_POINT('',#7709);
#2271=VERTEX_POINT('',#7713);
#2272=VERTEX_POINT('',#7715);
#2273=VERTEX_POINT('',#7717);
#2274=VERTEX_POINT('',#7721);
#2275=VERTEX_POINT('',#7723);
#2276=VERTEX_POINT('',#7727);
#2277=VERTEX_POINT('',#7731);
#2278=VERTEX_POINT('',#7735);
#2279=VERTEX_POINT('',#7740);
#2280=VERTEX_POINT('',#7742);
#2281=VERTEX_POINT('',#7744);
#2282=VERTEX_POINT('',#7746);
#2283=VERTEX_POINT('',#7748);
#2284=VERTEX_POINT('',#7763);
#2285=VERTEX_POINT('',#7765);
#2286=VERTEX_POINT('',#7769);
#2287=VERTEX_POINT('',#7771);
#2288=VERTEX_POINT('',#7775);
#2289=VERTEX_POINT('',#7776);
#2290=VERTEX_POINT('',#7778);
#2291=VERTEX_POINT('',#7782);
#2292=VERTEX_POINT('',#7784);
#2293=VERTEX_POINT('',#7788);
#2294=VERTEX_POINT('',#7790);
#2295=VERTEX_POINT('',#7792);
#2296=VERTEX_POINT('',#7794);
#2297=VERTEX_POINT('',#7796);
#2298=VERTEX_POINT('',#7798);
#2299=VERTEX_POINT('',#7800);
#2300=VERTEX_POINT('',#7802);
#2301=VERTEX_POINT('',#7804);
#2302=VERTEX_POINT('',#7808);
#2303=VERTEX_POINT('',#7810);
#2304=VERTEX_POINT('',#7812);
#2305=VERTEX_POINT('',#7814);
#2306=VERTEX_POINT('',#7817);
#2307=VERTEX_POINT('',#7819);
#2308=VERTEX_POINT('',#7827);
#2309=VERTEX_POINT('',#7832);
#2310=VERTEX_POINT('',#7835);
#2311=VERTEX_POINT('',#7842);
#2312=VERTEX_POINT('',#7850);
#2313=VERTEX_POINT('',#7852);
#2314=VERTEX_POINT('',#7855);
#2315=VERTEX_POINT('',#7859);
#2316=VERTEX_POINT('',#7861);
#2317=VERTEX_POINT('',#7864);
#2318=VERTEX_POINT('',#7873);
#2319=VERTEX_POINT('',#7874);
#2320=VERTEX_POINT('',#7876);
#2321=VERTEX_POINT('',#7878);
#2322=VERTEX_POINT('',#7882);
#2323=VERTEX_POINT('',#7884);
#2324=VERTEX_POINT('',#7888);
#2325=VERTEX_POINT('',#7890);
#2326=VERTEX_POINT('',#7900);
#2327=VERTEX_POINT('',#7902);
#2328=VERTEX_POINT('',#7907);
#2329=VERTEX_POINT('',#7909);
#2330=VERTEX_POINT('',#7914);
#2331=VERTEX_POINT('',#7916);
#2332=VERTEX_POINT('',#7921);
#2333=VERTEX_POINT('',#7923);
#2334=VERTEX_POINT('',#7928);
#2335=VERTEX_POINT('',#7930);
#2336=VERTEX_POINT('',#7934);
#2337=VERTEX_POINT('',#7936);
#2338=VERTEX_POINT('',#7940);
#2339=VERTEX_POINT('',#7941);
#2340=VERTEX_POINT('',#7943);
#2341=VERTEX_POINT('',#7945);
#2342=VERTEX_POINT('',#7949);
#2343=VERTEX_POINT('',#7950);
#2344=VERTEX_POINT('',#7952);
#2345=VERTEX_POINT('',#7954);
#2346=VERTEX_POINT('',#7958);
#2347=VERTEX_POINT('',#7959);
#2348=VERTEX_POINT('',#7961);
#2349=VERTEX_POINT('',#7963);
#2350=VERTEX_POINT('',#7967);
#2351=VERTEX_POINT('',#7968);
#2352=VERTEX_POINT('',#7970);
#2353=VERTEX_POINT('',#7972);
#2354=VERTEX_POINT('',#7976);
#2355=VERTEX_POINT('',#7977);
#2356=VERTEX_POINT('',#7979);
#2357=VERTEX_POINT('',#7981);
#2358=VERTEX_POINT('',#7985);
#2359=VERTEX_POINT('',#7986);
#2360=VERTEX_POINT('',#7988);
#2361=VERTEX_POINT('',#7990);
#2362=VERTEX_POINT('',#7994);
#2363=VERTEX_POINT('',#7995);
#2364=VERTEX_POINT('',#7997);
#2365=VERTEX_POINT('',#7999);
#2366=VERTEX_POINT('',#8003);
#2367=VERTEX_POINT('',#8004);
#2368=VERTEX_POINT('',#8006);
#2369=VERTEX_POINT('',#8008);
#2370=VERTEX_POINT('',#8012);
#2371=VERTEX_POINT('',#8014);
#2372=VERTEX_POINT('',#8016);
#2373=VERTEX_POINT('',#8018);
#2374=VERTEX_POINT('',#8021);
#2375=VERTEX_POINT('',#8023);
#2376=VERTEX_POINT('',#8026);
#2377=VERTEX_POINT('',#8028);
#2378=VERTEX_POINT('',#8031);
#2379=VERTEX_POINT('',#8033);
#2380=VERTEX_POINT('',#8036);
#2381=VERTEX_POINT('',#8038);
#2382=VERTEX_POINT('',#8040);
#2383=VERTEX_POINT('',#8042);
#2384=VERTEX_POINT('',#8045);
#2385=VERTEX_POINT('',#8047);
#2386=VERTEX_POINT('',#8050);
#2387=VERTEX_POINT('',#8052);
#2388=VERTEX_POINT('',#8055);
#2389=VERTEX_POINT('',#8057);
#2390=VERTEX_POINT('',#8061);
#2391=VERTEX_POINT('',#8065);
#2392=VERTEX_POINT('',#8069);
#2393=VERTEX_POINT('',#8073);
#2394=VERTEX_POINT('',#8081);
#2395=VERTEX_POINT('',#8085);
#2396=VERTEX_POINT('',#8089);
#2397=VERTEX_POINT('',#8093);
#2398=VERTEX_POINT('',#8101);
#2399=VERTEX_POINT('',#8105);
#2400=VERTEX_POINT('',#8109);
#2401=VERTEX_POINT('',#8113);
#2402=VERTEX_POINT('',#8121);
#2403=VERTEX_POINT('',#8125);
#2404=VERTEX_POINT('',#8129);
#2405=VERTEX_POINT('',#8133);
#2406=VERTEX_POINT('',#8141);
#2407=VERTEX_POINT('',#8143);
#2408=VERTEX_POINT('',#8147);
#2409=VERTEX_POINT('',#8151);
#2410=VERTEX_POINT('',#8159);
#2411=VERTEX_POINT('',#8160);
#2412=VERTEX_POINT('',#8162);
#2413=VERTEX_POINT('',#8164);
#2414=VERTEX_POINT('',#8168);
#2415=VERTEX_POINT('',#8169);
#2416=VERTEX_POINT('',#8171);
#2417=VERTEX_POINT('',#8173);
#2418=VERTEX_POINT('',#8180);
#2419=VERTEX_POINT('',#8182);
#2420=VERTEX_POINT('',#8184);
#2421=VERTEX_POINT('',#8186);
#2422=VERTEX_POINT('',#8190);
#2423=VERTEX_POINT('',#8194);
#2424=VERTEX_POINT('',#8196);
#2425=VERTEX_POINT('',#8200);
#2426=VERTEX_POINT('',#8210);
#2427=VERTEX_POINT('',#8211);
#2428=VERTEX_POINT('',#8213);
#2429=VERTEX_POINT('',#8215);
#2430=VERTEX_POINT('',#8219);
#2431=VERTEX_POINT('',#8221);
#2432=VERTEX_POINT('',#8225);
#2433=VERTEX_POINT('',#8227);
#2434=VERTEX_POINT('',#8231);
#2435=VERTEX_POINT('',#8233);
#2436=VERTEX_POINT('',#8237);
#2437=VERTEX_POINT('',#8239);
#2438=VERTEX_POINT('',#8249);
#2439=VERTEX_POINT('',#8250);
#2440=VERTEX_POINT('',#8252);
#2441=VERTEX_POINT('',#8433);
#2442=VERTEX_POINT('',#8482);
#2443=VERTEX_POINT('',#8483);
#2444=VERTEX_POINT('',#8713);
#2445=VERTEX_POINT('',#8927);
#2446=VERTEX_POINT('',#8928);
#2447=VERTEX_POINT('',#8930);
#2448=VERTEX_POINT('',#9414);
#2449=VERTEX_POINT('',#9415);
#2450=VERTEX_POINT('',#9663);
#2451=VERTEX_POINT('',#9901);
#2452=VERTEX_POINT('',#9902);
#2453=VERTEX_POINT('',#9904);
#2454=VERTEX_POINT('',#10402);
#2455=VERTEX_POINT('',#10403);
#2456=VERTEX_POINT('',#10631);
#2457=VERTEX_POINT('',#10755);
#2458=VERTEX_POINT('',#10756);
#2459=VERTEX_POINT('',#10758);
#2460=VERTEX_POINT('',#10849);
#2461=VERTEX_POINT('',#10879);
#2462=VERTEX_POINT('',#10880);
#2463=VERTEX_POINT('',#10882);
#2464=VERTEX_POINT('',#10967);
#2465=VERTEX_POINT('',#11180);
#2466=VERTEX_POINT('',#11181);
#2467=VERTEX_POINT('',#11183);
#2468=VERTEX_POINT('',#11609);
#2469=VERTEX_POINT('',#11610);
#2470=VERTEX_POINT('',#11838);
#2471=VERTEX_POINT('',#12112);
#2472=VERTEX_POINT('',#12113);
#2473=VERTEX_POINT('',#12115);
#2474=VERTEX_POINT('',#12611);
#2475=VERTEX_POINT('',#12612);
#2476=VERTEX_POINT('',#12854);
#2477=VERTEX_POINT('',#13150);
#2478=VERTEX_POINT('',#13151);
#2479=VERTEX_POINT('',#13153);
#2480=VERTEX_POINT('',#13801);
#2481=VERTEX_POINT('',#13802);
#2482=VERTEX_POINT('',#14050);
#2483=VERTEX_POINT('',#14302);
#2484=VERTEX_POINT('',#14303);
#2485=VERTEX_POINT('',#14305);
#2486=VERTEX_POINT('',#14803);
#2487=VERTEX_POINT('',#14804);
#2488=VERTEX_POINT('',#15048);
#2489=VERTEX_POINT('',#15286);
#2490=VERTEX_POINT('',#15287);
#2491=VERTEX_POINT('',#15289);
#2492=VERTEX_POINT('',#15781);
#2493=VERTEX_POINT('',#15782);
#2494=VERTEX_POINT('',#16012);
#2495=VERTEX_POINT('',#16138);
#2496=VERTEX_POINT('',#16139);
#2497=VERTEX_POINT('',#16141);
#2498=VERTEX_POINT('',#16235);
#2499=VERTEX_POINT('',#16265);
#2500=VERTEX_POINT('',#16266);
#2501=VERTEX_POINT('',#16268);
#2502=VERTEX_POINT('',#16353);
#2503=VERTEX_POINT('',#16560);
#2504=VERTEX_POINT('',#16561);
#2505=VERTEX_POINT('',#16563);
#2506=VERTEX_POINT('',#17005);
#2507=VERTEX_POINT('',#17006);
#2508=VERTEX_POINT('',#17264);
#2509=VERTEX_POINT('',#17532);
#2510=VERTEX_POINT('',#17533);
#2511=VERTEX_POINT('',#17535);
#2512=VERTEX_POINT('',#18097);
#2513=VERTEX_POINT('',#18098);
#2514=VERTEX_POINT('',#18342);
#2515=VERTEX_POINT('',#18602);
#2516=VERTEX_POINT('',#18603);
#2517=VERTEX_POINT('',#18605);
#2518=VERTEX_POINT('',#19071);
#2519=VERTEX_POINT('',#19072);
#2520=VERTEX_POINT('',#19308);
#2521=VERTEX_POINT('',#19536);
#2522=VERTEX_POINT('',#19537);
#2523=VERTEX_POINT('',#19539);
#2524=VERTEX_POINT('',#20027);
#2525=VERTEX_POINT('',#20028);
#2526=VERTEX_POINT('',#20298);
#2527=VERTEX_POINT('',#20349);
#2528=VERTEX_POINT('',#20350);
#2529=VERTEX_POINT('',#20352);
#2530=VERTEX_POINT('',#20631);
#2531=VERTEX_POINT('',#20825);
#2532=VERTEX_POINT('',#20826);
#2533=VERTEX_POINT('',#21283);
#2534=VERTEX_POINT('',#21284);
#2535=VERTEX_POINT('',#21286);
#2536=VERTEX_POINT('',#21354);
#2537=VERTEX_POINT('',#21584);
#2538=VERTEX_POINT('',#21585);
#2539=VERTEX_POINT('',#21587);
#2540=VERTEX_POINT('',#21932);
#2541=VERTEX_POINT('',#21933);
#2542=VERTEX_POINT('',#21935);
#2543=VERTEX_POINT('',#22140);
#2544=VERTEX_POINT('',#22284);
#2545=VERTEX_POINT('',#22285);
#2546=VERTEX_POINT('',#22521);
#2547=VERTEX_POINT('',#22779);
#2548=VERTEX_POINT('',#22780);
#2549=VERTEX_POINT('',#22818);
#2550=VERTEX_POINT('',#22820);
#2551=VERTEX_POINT('',#22843);
#2552=VERTEX_POINT('',#22956);
#2553=VERTEX_POINT('',#22967);
#2554=VERTEX_POINT('',#22979);
#2555=VERTEX_POINT('',#23095);
#2556=VERTEX_POINT('',#23106);
#2557=VERTEX_POINT('',#23117);
#2558=VERTEX_POINT('',#23233);
#2559=VERTEX_POINT('',#23244);
#2560=VERTEX_POINT('',#23255);
#2561=VERTEX_POINT('',#23371);
#2562=VERTEX_POINT('',#23382);
#2563=VERTEX_POINT('',#23393);
#2564=VERTEX_POINT('',#23509);
#2565=VERTEX_POINT('',#23522);
#2566=VERTEX_POINT('',#23533);
#2567=VERTEX_POINT('',#23646);
#2568=VERTEX_POINT('',#23658);
#2569=VERTEX_POINT('',#23669);
#2570=VERTEX_POINT('',#23785);
#2571=VERTEX_POINT('',#23797);
#2572=VERTEX_POINT('',#23808);
#2573=VERTEX_POINT('',#23924);
#2574=VERTEX_POINT('',#23935);
#2575=VERTEX_POINT('',#23948);
#2576=VERTEX_POINT('',#24061);
#2577=VERTEX_POINT('',#24072);
#2578=VERTEX_POINT('',#24084);
#2579=VERTEX_POINT('',#24200);
#2580=VERTEX_POINT('',#24211);
#2581=VERTEX_POINT('',#24223);
#2582=VERTEX_POINT('',#24336);
#2583=VERTEX_POINT('',#24347);
#2584=VERTEX_POINT('',#24460);
#2585=VERTEX_POINT('',#24472);
#2586=VERTEX_POINT('',#24486);
#2587=VERTEX_POINT('',#24488);
#2588=VERTEX_POINT('',#24499);
#2589=VERTEX_POINT('',#24612);
#2590=VERTEX_POINT('',#24728);
#2591=VERTEX_POINT('',#24739);
#2592=VERTEX_POINT('',#24858);
#2593=VERTEX_POINT('',#24869);
#2594=VERTEX_POINT('',#24880);
#2595=VERTEX_POINT('',#24996);
#2596=VERTEX_POINT('',#25007);
#2597=VERTEX_POINT('',#25018);
#2598=VERTEX_POINT('',#25134);
#2599=VERTEX_POINT('',#25145);
#2600=VERTEX_POINT('',#25156);
#2601=VERTEX_POINT('',#25269);
#2602=VERTEX_POINT('',#25281);
#2603=VERTEX_POINT('',#25292);
#2604=VERTEX_POINT('',#25408);
#2605=VERTEX_POINT('',#25420);
#2606=VERTEX_POINT('',#25431);
#2607=VERTEX_POINT('',#25544);
#2608=VERTEX_POINT('',#25556);
#2609=VERTEX_POINT('',#25567);
#2610=VERTEX_POINT('',#25683);
#2611=VERTEX_POINT('',#25694);
#2612=VERTEX_POINT('',#25706);
#2613=VERTEX_POINT('',#25822);
#2614=VERTEX_POINT('',#25833);
#2615=VERTEX_POINT('',#25845);
#2616=VERTEX_POINT('',#25958);
#2617=VERTEX_POINT('',#25969);
#2618=VERTEX_POINT('',#26085);
#2619=VERTEX_POINT('',#26201);
#2620=VERTEX_POINT('',#26223);
#2621=VERTEX_POINT('',#26462);
#2622=VERTEX_POINT('',#26464);
#2623=VERTEX_POINT('',#27491);
#2624=VERTEX_POINT('',#28432);
#2625=VERTEX_POINT('',#28548);
#2626=VERTEX_POINT('',#28549);
#2627=VERTEX_POINT('',#28551);
#2628=VERTEX_POINT('',#28553);
#2629=VERTEX_POINT('',#28557);
#2630=VERTEX_POINT('',#28559);
#2631=VERTEX_POINT('',#28563);
#2632=VERTEX_POINT('',#28565);
#2633=VERTEX_POINT('',#28569);
#2634=VERTEX_POINT('',#28571);
#2635=VERTEX_POINT('',#28575);
#2636=VERTEX_POINT('',#28577);
#2637=VERTEX_POINT('',#28585);
#2638=VERTEX_POINT('',#28588);
#2639=VERTEX_POINT('',#28595);
#2640=VERTEX_POINT('',#28596);
#2641=VERTEX_POINT('',#28598);
#2642=VERTEX_POINT('',#28603);
#2643=VERTEX_POINT('',#28625);
#2644=VERTEX_POINT('',#28626);
#2645=VERTEX_POINT('',#28628);
#2646=VERTEX_POINT('',#28708);
#2647=VERTEX_POINT('',#28761);
#2648=VERTEX_POINT('',#28762);
#2649=VERTEX_POINT('',#28764);
#2650=VERTEX_POINT('',#28887);
#2651=VERTEX_POINT('',#28903);
#2652=VERTEX_POINT('',#28904);
#2653=VERTEX_POINT('',#28906);
#2654=VERTEX_POINT('',#28958);
#2655=VERTEX_POINT('',#29039);
#2656=VERTEX_POINT('',#29040);
#2657=VERTEX_POINT('',#29042);
#2658=VERTEX_POINT('',#29057);
#2659=VERTEX_POINT('',#29110);
#2660=VERTEX_POINT('',#29111);
#2661=VERTEX_POINT('',#29113);
#2662=VERTEX_POINT('',#29120);
#2663=VERTEX_POINT('',#29126);
#2664=VERTEX_POINT('',#29128);
#2665=VERTEX_POINT('',#29171);
#2666=VERTEX_POINT('',#29172);
#2667=VERTEX_POINT('',#29174);
#2668=VERTEX_POINT('',#29184);
#2669=VERTEX_POINT('',#29185);
#2670=VERTEX_POINT('',#29187);
#2671=VERTEX_POINT('',#29268);
#2672=VERTEX_POINT('',#29419);
#2673=VERTEX_POINT('',#29420);
#2674=VERTEX_POINT('',#29422);
#2675=VERTEX_POINT('',#29715);
#2676=VERTEX_POINT('',#29716);
#2677=VERTEX_POINT('',#29864);
#2678=VERTEX_POINT('',#30018);
#2679=VERTEX_POINT('',#30019);
#2680=VERTEX_POINT('',#30021);
#2681=VERTEX_POINT('',#30191);
#2682=VERTEX_POINT('',#30192);
#2683=VERTEX_POINT('',#30194);
#2684=VERTEX_POINT('',#30205);
#2685=VERTEX_POINT('',#30270);
#2686=VERTEX_POINT('',#30272);
#2687=VERTEX_POINT('',#30366);
#2688=VERTEX_POINT('',#30466);
#2689=VERTEX_POINT('',#30569);
#2690=VERTEX_POINT('',#30584);
#2691=VERTEX_POINT('',#31130);
#2692=VERTEX_POINT('',#31131);
#2693=VERTEX_POINT('',#31133);
#2694=VERTEX_POINT('',#31135);
#2695=VERTEX_POINT('',#31137);
#2696=VERTEX_POINT('',#31139);
#2697=VERTEX_POINT('',#31143);
#2698=VERTEX_POINT('',#31144);
#2699=VERTEX_POINT('',#31149);
#2700=VERTEX_POINT('',#31153);
#2701=VERTEX_POINT('',#31157);
#2702=VERTEX_POINT('',#31161);
#2703=VERTEX_POINT('',#31169);
#2704=VERTEX_POINT('',#31171);
#2705=VERTEX_POINT('',#31176);
#2706=VERTEX_POINT('',#31178);
#2707=VERTEX_POINT('',#31183);
#2708=VERTEX_POINT('',#31185);
#2709=VERTEX_POINT('',#31190);
#2710=VERTEX_POINT('',#31192);
#2711=VERTEX_POINT('',#31197);
#2712=VERTEX_POINT('',#31198);
#2713=VERTEX_POINT('',#31200);
#2714=VERTEX_POINT('',#31202);
#2715=VERTEX_POINT('',#31206);
#2716=VERTEX_POINT('',#31207);
#2717=VERTEX_POINT('',#31209);
#2718=VERTEX_POINT('',#31211);
#2719=VERTEX_POINT('',#31215);
#2720=VERTEX_POINT('',#31216);
#2721=VERTEX_POINT('',#31218);
#2722=VERTEX_POINT('',#31220);
#2723=VERTEX_POINT('',#31224);
#2724=VERTEX_POINT('',#31225);
#2725=VERTEX_POINT('',#31227);
#2726=VERTEX_POINT('',#31229);
#2727=VERTEX_POINT('',#31233);
#2728=VERTEX_POINT('',#31234);
#2729=VERTEX_POINT('',#31236);
#2730=VERTEX_POINT('',#31238);
#2731=VERTEX_POINT('',#31242);
#2732=VERTEX_POINT('',#31243);
#2733=VERTEX_POINT('',#31245);
#2734=VERTEX_POINT('',#31247);
#2735=VERTEX_POINT('',#31251);
#2736=VERTEX_POINT('',#31252);
#2737=VERTEX_POINT('',#31254);
#2738=VERTEX_POINT('',#31256);
#2739=VERTEX_POINT('',#31260);
#2740=VERTEX_POINT('',#31261);
#2741=VERTEX_POINT('',#31263);
#2742=VERTEX_POINT('',#31265);
#2743=VERTEX_POINT('',#31269);
#2744=VERTEX_POINT('',#31271);
#2745=VERTEX_POINT('',#31273);
#2746=VERTEX_POINT('',#31275);
#2747=VERTEX_POINT('',#31278);
#2748=VERTEX_POINT('',#31280);
#2749=VERTEX_POINT('',#31283);
#2750=VERTEX_POINT('',#31285);
#2751=VERTEX_POINT('',#31288);
#2752=VERTEX_POINT('',#31290);
#2753=VERTEX_POINT('',#31293);
#2754=VERTEX_POINT('',#31295);
#2755=VERTEX_POINT('',#31297);
#2756=VERTEX_POINT('',#31299);
#2757=VERTEX_POINT('',#31302);
#2758=VERTEX_POINT('',#31304);
#2759=VERTEX_POINT('',#31307);
#2760=VERTEX_POINT('',#31309);
#2761=VERTEX_POINT('',#31312);
#2762=VERTEX_POINT('',#31314);
#2763=VERTEX_POINT('',#31318);
#2764=VERTEX_POINT('',#31322);
#2765=VERTEX_POINT('',#31326);
#2766=VERTEX_POINT('',#31330);
#2767=VERTEX_POINT('',#31338);
#2768=VERTEX_POINT('',#31342);
#2769=VERTEX_POINT('',#31346);
#2770=VERTEX_POINT('',#31350);
#2771=VERTEX_POINT('',#31358);
#2772=VERTEX_POINT('',#31362);
#2773=VERTEX_POINT('',#31366);
#2774=VERTEX_POINT('',#31370);
#2775=VERTEX_POINT('',#31378);
#2776=VERTEX_POINT('',#31382);
#2777=VERTEX_POINT('',#31386);
#2778=VERTEX_POINT('',#31390);
#2779=VERTEX_POINT('',#31398);
#2780=VERTEX_POINT('',#31400);
#2781=VERTEX_POINT('',#31404);
#2782=VERTEX_POINT('',#31408);
#2783=VERTEX_POINT('',#31416);
#2784=VERTEX_POINT('',#31417);
#2785=VERTEX_POINT('',#31419);
#2786=VERTEX_POINT('',#31421);
#2787=VERTEX_POINT('',#31425);
#2788=VERTEX_POINT('',#31426);
#2789=VERTEX_POINT('',#31428);
#2790=VERTEX_POINT('',#31430);
#2791=VERTEX_POINT('',#31437);
#2792=VERTEX_POINT('',#31439);
#2793=VERTEX_POINT('',#31441);
#2794=VERTEX_POINT('',#31443);
#2795=VERTEX_POINT('',#31447);
#2796=VERTEX_POINT('',#31451);
#2797=VERTEX_POINT('',#31453);
#2798=VERTEX_POINT('',#31457);
#2799=VERTEX_POINT('',#31467);
#2800=VERTEX_POINT('',#31468);
#2801=VERTEX_POINT('',#31470);
#2802=VERTEX_POINT('',#31472);
#2803=VERTEX_POINT('',#31476);
#2804=VERTEX_POINT('',#31478);
#2805=VERTEX_POINT('',#31482);
#2806=VERTEX_POINT('',#31484);
#2807=VERTEX_POINT('',#31494);
#2808=VERTEX_POINT('',#31496);
#2809=EDGE_CURVE('',#2220,#2221,#1206,.T.);
#2810=EDGE_CURVE('',#2221,#2222,#1207,.T.);
#2811=EDGE_CURVE('',#2223,#2222,#1208,.T.);
#2812=EDGE_CURVE('',#2220,#2223,#1209,.T.);
#2813=EDGE_CURVE('',#2224,#2220,#1210,.T.);
#2814=EDGE_CURVE('',#2225,#2223,#1211,.T.);
#2815=EDGE_CURVE('',#2224,#2225,#1212,.T.);
#2816=EDGE_CURVE('',#2226,#2224,#1213,.T.);
#2817=EDGE_CURVE('',#2227,#2225,#1214,.T.);
#2818=EDGE_CURVE('',#2226,#2227,#1215,.T.);
#2819=EDGE_CURVE('',#2221,#2226,#1216,.T.);
#2820=EDGE_CURVE('',#2222,#2227,#1217,.T.);
#2821=EDGE_CURVE('',#2228,#2229,#1218,.T.);
#2822=EDGE_CURVE('',#2228,#2230,#1219,.T.);
#2823=EDGE_CURVE('',#2231,#2230,#1220,.T.);
#2824=EDGE_CURVE('',#2229,#2231,#1221,.T.);
#2825=EDGE_CURVE('',#2232,#2228,#417,.T.);
#2826=EDGE_CURVE('',#2232,#2233,#1222,.T.);
#2827=EDGE_CURVE('',#2230,#2233,#418,.T.);
#2828=EDGE_CURVE('',#2234,#2232,#1223,.T.);
#2829=EDGE_CURVE('',#2234,#2235,#1224,.T.);
#2830=EDGE_CURVE('',#2233,#2235,#1225,.T.);
#2831=EDGE_CURVE('',#2229,#2234,#419,.T.);
#2832=EDGE_CURVE('',#2235,#2231,#420,.T.);
#2833=EDGE_CURVE('',#2236,#2236,#421,.T.);
#2834=EDGE_CURVE('',#2236,#2237,#1226,.T.);
#2835=EDGE_CURVE('',#2237,#2237,#422,.T.);
#2836=EDGE_CURVE('',#2238,#2238,#423,.T.);
#2837=EDGE_CURVE('',#2238,#2239,#1227,.T.);
#2838=EDGE_CURVE('',#2239,#2239,#424,.T.);
#2839=EDGE_CURVE('',#2240,#2241,#1228,.T.);
#2840=EDGE_CURVE('',#2241,#2242,#1229,.T.);
#2841=EDGE_CURVE('',#2243,#2242,#1230,.T.);
#2842=EDGE_CURVE('',#2240,#2243,#1231,.T.);
#2843=EDGE_CURVE('',#2244,#2240,#1232,.T.);
#2844=EDGE_CURVE('',#2245,#2243,#1233,.T.);
#2845=EDGE_CURVE('',#2244,#2245,#1234,.T.);
#2846=EDGE_CURVE('',#2246,#2244,#1235,.T.);
#2847=EDGE_CURVE('',#2247,#2245,#1236,.T.);
#2848=EDGE_CURVE('',#2246,#2247,#1237,.T.);
#2849=EDGE_CURVE('',#2241,#2246,#1238,.T.);
#2850=EDGE_CURVE('',#2242,#2247,#1239,.T.);
#2851=EDGE_CURVE('',#2248,#2248,#425,.T.);
#2852=EDGE_CURVE('',#2248,#2249,#1240,.T.);
#2853=EDGE_CURVE('',#2249,#2249,#426,.T.);
#2854=EDGE_CURVE('',#2250,#2250,#427,.T.);
#2855=EDGE_CURVE('',#2250,#2251,#1241,.T.);
#2856=EDGE_CURVE('',#2251,#2251,#428,.T.);
#2857=EDGE_CURVE('',#2252,#2253,#1242,.T.);
#2858=EDGE_CURVE('',#2254,#2252,#429,.T.);
#2859=EDGE_CURVE('',#2255,#2254,#1243,.T.);
#2860=EDGE_CURVE('',#2253,#2255,#1244,.T.);
#2861=EDGE_CURVE('',#2256,#2252,#1245,.T.);
#2862=EDGE_CURVE('',#2257,#2256,#430,.T.);
#2863=EDGE_CURVE('',#2254,#2257,#1246,.T.);
#2864=EDGE_CURVE('',#2258,#2256,#1247,.T.);
#2865=EDGE_CURVE('',#2259,#2258,#1248,.T.);
#2866=EDGE_CURVE('',#2257,#2259,#1249,.T.);
#2867=EDGE_CURVE('',#2260,#2259,#1250,.T.);
#2868=EDGE_CURVE('',#2260,#2261,#1251,.T.);
#2869=EDGE_CURVE('',#2261,#2262,#1252,.T.);
#2870=EDGE_CURVE('',#2262,#2263,#1253,.T.);
#2871=EDGE_CURVE('',#2263,#2264,#1254,.T.);
#2872=EDGE_CURVE('',#2265,#2264,#1255,.T.);
#2873=EDGE_CURVE('',#2265,#2266,#1256,.T.);
#2874=EDGE_CURVE('',#2266,#2267,#1257,.T.);
#2875=EDGE_CURVE('',#2255,#2267,#1258,.T.);
#2876=EDGE_CURVE('',#2268,#2258,#1259,.T.);
#2877=EDGE_CURVE('',#2268,#2269,#1260,.T.);
#2878=EDGE_CURVE('',#2269,#2270,#1261,.T.);
#2879=EDGE_CURVE('',#2270,#2260,#1262,.T.);
#2880=EDGE_CURVE('',#2267,#2271,#1263,.T.);
#2881=EDGE_CURVE('',#2271,#2272,#1264,.T.);
#2882=EDGE_CURVE('',#2273,#2272,#1265,.T.);
#2883=EDGE_CURVE('',#2253,#2273,#1266,.T.);
#2884=EDGE_CURVE('',#2274,#2266,#431,.T.);
#2885=EDGE_CURVE('',#2275,#2274,#1267,.T.);
#2886=EDGE_CURVE('',#2271,#2275,#432,.T.);
#2887=EDGE_CURVE('',#2276,#2265,#433,.T.);
#2888=EDGE_CURVE('',#2274,#2276,#1268,.T.);
#2889=EDGE_CURVE('',#2277,#2275,#1269,.T.);
#2890=EDGE_CURVE('',#2272,#2277,#434,.T.);
#2891=EDGE_CURVE('',#2264,#2278,#1270,.T.);
#2892=EDGE_CURVE('',#2278,#2276,#1271,.T.);
#2893=EDGE_CURVE('',#2277,#2273,#1272,.T.);
#2894=EDGE_CURVE('',#2279,#2278,#1273,.T.);
#2895=EDGE_CURVE('',#2279,#2280,#1274,.T.);
#2896=EDGE_CURVE('',#2280,#2281,#1275,.T.);
#2897=EDGE_CURVE('',#2281,#2282,#1276,.T.);
#2898=EDGE_CURVE('',#2282,#2283,#1277,.T.);
#2899=EDGE_CURVE('',#2283,#2268,#1278,.T.);
#2900=EDGE_CURVE('',#2269,#2283,#435,.T.);
#2901=EDGE_CURVE('',#2270,#2282,#436,.T.);
#2902=EDGE_CURVE('',#2281,#2261,#437,.T.);
#2903=EDGE_CURVE('',#2280,#2262,#438,.T.);
#2904=EDGE_CURVE('',#2263,#2279,#1279,.T.);
#2905=EDGE_CURVE('',#2284,#2284,#439,.T.);
#2906=EDGE_CURVE('',#2284,#2285,#1280,.T.);
#2907=EDGE_CURVE('',#2285,#2285,#440,.T.);
#2908=EDGE_CURVE('',#2286,#2286,#441,.T.);
#2909=EDGE_CURVE('',#2286,#2287,#1281,.T.);
#2910=EDGE_CURVE('',#2287,#2287,#442,.T.);
#2911=EDGE_CURVE('',#2288,#2289,#1282,.T.);
#2912=EDGE_CURVE('',#2288,#2290,#443,.T.);
#2913=EDGE_CURVE('',#2289,#2290,#1283,.T.);
#2914=EDGE_CURVE('',#2291,#2288,#1284,.T.);
#2915=EDGE_CURVE('',#2292,#2291,#444,.T.);
#2916=EDGE_CURVE('',#2290,#2292,#1285,.T.);
#2917=EDGE_CURVE('',#2293,#2289,#1286,.T.);
#2918=EDGE_CURVE('',#2293,#2294,#1287,.T.);
#2919=EDGE_CURVE('',#2294,#2295,#1288,.T.);
#2920=EDGE_CURVE('',#2295,#2296,#1289,.T.);
#2921=EDGE_CURVE('',#2297,#2296,#1290,.T.);
#2922=EDGE_CURVE('',#2297,#2298,#1291,.T.);
#2923=EDGE_CURVE('',#2298,#2299,#1292,.T.);
#2924=EDGE_CURVE('',#2299,#2300,#1293,.T.);
#2925=EDGE_CURVE('',#2300,#2301,#1294,.T.);
#2926=EDGE_CURVE('',#2291,#2301,#1295,.T.);
#2927=EDGE_CURVE('',#2302,#2292,#1296,.T.);
#2928=EDGE_CURVE('',#2303,#2302,#1297,.T.);
#2929=EDGE_CURVE('',#2303,#2304,#1298,.T.);
#2930=EDGE_CURVE('',#2304,#2305,#1299,.T.);
#2931=EDGE_CURVE('',#2305,#2297,#1300,.T.);
#2932=EDGE_CURVE('',#2296,#2306,#1301,.T.);
#2933=EDGE_CURVE('',#2306,#2307,#1302,.T.);
#2934=EDGE_CURVE('',#2307,#2293,#1303,.T.);
#2935=EDGE_CURVE('',#2298,#2305,#445,.T.);
#2936=EDGE_CURVE('',#2299,#2304,#446,.T.);
#2937=EDGE_CURVE('',#2308,#2303,#1304,.T.);
#2938=EDGE_CURVE('',#2300,#2308,#1305,.T.);
#2939=EDGE_CURVE('',#2307,#2294,#447,.T.);
#2940=EDGE_CURVE('',#2309,#2309,#448,.T.);
#2941=EDGE_CURVE('',#2310,#2310,#449,.T.);
#2942=EDGE_CURVE('',#2310,#2309,#1306,.T.);
#2943=EDGE_CURVE('',#2306,#2295,#450,.T.);
#2944=EDGE_CURVE('',#2311,#2302,#1307,.T.);
#2945=EDGE_CURVE('',#2308,#2311,#1308,.T.);
#2946=EDGE_CURVE('',#2301,#2311,#1309,.T.);
#2947=EDGE_CURVE('',#2312,#2312,#451,.T.);
#2948=EDGE_CURVE('',#2313,#2313,#452,.T.);
#2949=EDGE_CURVE('',#2314,#2314,#453,.T.);
#2950=EDGE_CURVE('',#2314,#2312,#1310,.T.);
#2951=EDGE_CURVE('',#2315,#2315,#454,.T.);
#2952=EDGE_CURVE('',#2316,#2316,#455,.T.);
#2953=EDGE_CURVE('',#2315,#2317,#1311,.T.);
#2954=EDGE_CURVE('',#2317,#2317,#456,.T.);
#2955=EDGE_CURVE('',#2313,#2316,#1312,.T.);
#2956=EDGE_CURVE('',#2318,#2319,#1313,.T.);
#2957=EDGE_CURVE('',#2319,#2320,#1314,.T.);
#2958=EDGE_CURVE('',#2321,#2320,#1315,.T.);
#2959=EDGE_CURVE('',#2318,#2321,#1316,.T.);
#2960=EDGE_CURVE('',#2322,#2318,#1317,.T.);
#2961=EDGE_CURVE('',#2323,#2321,#1318,.T.);
#2962=EDGE_CURVE('',#2322,#2323,#1319,.T.);
#2963=EDGE_CURVE('',#2324,#2322,#1320,.T.);
#2964=EDGE_CURVE('',#2325,#2323,#1321,.T.);
#2965=EDGE_CURVE('',#2324,#2325,#1322,.T.);
#2966=EDGE_CURVE('',#2319,#2324,#1323,.T.);
#2967=EDGE_CURVE('',#2320,#2325,#1324,.T.);
#2968=EDGE_CURVE('',#2326,#2326,#457,.T.);
#2969=EDGE_CURVE('',#2326,#2327,#1325,.T.);
#2970=EDGE_CURVE('',#2327,#2327,#458,.T.);
#2971=EDGE_CURVE('',#2328,#2328,#459,.T.);
#2972=EDGE_CURVE('',#2328,#2329,#1326,.T.);
#2973=EDGE_CURVE('',#2329,#2329,#460,.T.);
#2974=EDGE_CURVE('',#2330,#2330,#461,.T.);
#2975=EDGE_CURVE('',#2330,#2331,#1327,.T.);
#2976=EDGE_CURVE('',#2331,#2331,#462,.T.);
#2977=EDGE_CURVE('',#2332,#2332,#463,.T.);
#2978=EDGE_CURVE('',#2332,#2333,#1328,.T.);
#2979=EDGE_CURVE('',#2333,#2333,#464,.T.);
#2980=EDGE_CURVE('',#2334,#2334,#465,.T.);
#2981=EDGE_CURVE('',#2334,#2335,#1329,.T.);
#2982=EDGE_CURVE('',#2335,#2335,#466,.T.);
#2983=EDGE_CURVE('',#2336,#2336,#467,.T.);
#2984=EDGE_CURVE('',#2336,#2337,#1330,.T.);
#2985=EDGE_CURVE('',#2337,#2337,#468,.T.);
#2986=EDGE_CURVE('',#2338,#2339,#1331,.T.);
#2987=EDGE_CURVE('',#2340,#2338,#1332,.T.);
#2988=EDGE_CURVE('',#2341,#2340,#1333,.T.);
#2989=EDGE_CURVE('',#2339,#2341,#1334,.T.);
#2990=EDGE_CURVE('',#2342,#2343,#1335,.T.);
#2991=EDGE_CURVE('',#2344,#2342,#1336,.T.);
#2992=EDGE_CURVE('',#2345,#2344,#1337,.T.);
#2993=EDGE_CURVE('',#2343,#2345,#1338,.T.);
#2994=EDGE_CURVE('',#2346,#2347,#1339,.T.);
#2995=EDGE_CURVE('',#2348,#2346,#1340,.T.);
#2996=EDGE_CURVE('',#2349,#2348,#1341,.T.);
#2997=EDGE_CURVE('',#2347,#2349,#1342,.T.);
#2998=EDGE_CURVE('',#2350,#2351,#1343,.T.);
#2999=EDGE_CURVE('',#2352,#2350,#1344,.T.);
#3000=EDGE_CURVE('',#2353,#2352,#1345,.T.);
#3001=EDGE_CURVE('',#2351,#2353,#1346,.T.);
#3002=EDGE_CURVE('',#2354,#2355,#1347,.T.);
#3003=EDGE_CURVE('',#2356,#2354,#1348,.T.);
#3004=EDGE_CURVE('',#2357,#2356,#1349,.T.);
#3005=EDGE_CURVE('',#2357,#2355,#1350,.T.);
#3006=EDGE_CURVE('',#2358,#2359,#1351,.T.);
#3007=EDGE_CURVE('',#2360,#2358,#1352,.T.);
#3008=EDGE_CURVE('',#2361,#2360,#1353,.T.);
#3009=EDGE_CURVE('',#2361,#2359,#1354,.T.);
#3010=EDGE_CURVE('',#2362,#2363,#1355,.T.);
#3011=EDGE_CURVE('',#2364,#2362,#1356,.T.);
#3012=EDGE_CURVE('',#2365,#2364,#1357,.T.);
#3013=EDGE_CURVE('',#2365,#2363,#1358,.T.);
#3014=EDGE_CURVE('',#2366,#2367,#1359,.T.);
#3015=EDGE_CURVE('',#2368,#2366,#1360,.T.);
#3016=EDGE_CURVE('',#2369,#2368,#1361,.T.);
#3017=EDGE_CURVE('',#2369,#2367,#1362,.T.);
#3018=EDGE_CURVE('',#2370,#2350,#1363,.T.);
#3019=EDGE_CURVE('',#2371,#2370,#1364,.T.);
#3020=EDGE_CURVE('',#2372,#2371,#1365,.T.);
#3021=EDGE_CURVE('',#2373,#2372,#1366,.T.);
#3022=EDGE_CURVE('',#2367,#2373,#1367,.T.);
#3023=EDGE_CURVE('',#2369,#2374,#1368,.T.);
#3024=EDGE_CURVE('',#2375,#2374,#1369,.T.);
#3025=EDGE_CURVE('',#2363,#2375,#1370,.T.);
#3026=EDGE_CURVE('',#2365,#2376,#1371,.T.);
#3027=EDGE_CURVE('',#2377,#2376,#1372,.T.);
#3028=EDGE_CURVE('',#2359,#2377,#1373,.T.);
#3029=EDGE_CURVE('',#2361,#2378,#1374,.T.);
#3030=EDGE_CURVE('',#2379,#2378,#1375,.T.);
#3031=EDGE_CURVE('',#2355,#2379,#1376,.T.);
#3032=EDGE_CURVE('',#2357,#2380,#1377,.T.);
#3033=EDGE_CURVE('',#2381,#2380,#1378,.T.);
#3034=EDGE_CURVE('',#2382,#2381,#1379,.T.);
#3035=EDGE_CURVE('',#2383,#2382,#1380,.T.);
#3036=EDGE_CURVE('',#2383,#2348,#1381,.T.);
#3037=EDGE_CURVE('',#2384,#2346,#1382,.T.);
#3038=EDGE_CURVE('',#2385,#2384,#1383,.T.);
#3039=EDGE_CURVE('',#2385,#2344,#1384,.T.);
#3040=EDGE_CURVE('',#2386,#2342,#1385,.T.);
#3041=EDGE_CURVE('',#2387,#2386,#1386,.T.);
#3042=EDGE_CURVE('',#2387,#2340,#1387,.T.);
#3043=EDGE_CURVE('',#2388,#2338,#1388,.T.);
#3044=EDGE_CURVE('',#2389,#2388,#1389,.T.);
#3045=EDGE_CURVE('',#2389,#2352,#1390,.T.);
#3046=EDGE_CURVE('',#2390,#2373,#1391,.T.);
#3047=EDGE_CURVE('',#2366,#2390,#1392,.T.);
#3048=EDGE_CURVE('',#2391,#2351,#1393,.T.);
#3049=EDGE_CURVE('',#2370,#2391,#1394,.T.);
#3050=EDGE_CURVE('',#2392,#2390,#1395,.T.);
#3051=EDGE_CURVE('',#2392,#2368,#1396,.T.);
#3052=EDGE_CURVE('',#2353,#2393,#1397,.T.);
#3053=EDGE_CURVE('',#2393,#2391,#1398,.T.);
#3054=EDGE_CURVE('',#2374,#2392,#1399,.T.);
#3055=EDGE_CURVE('',#2393,#2389,#1400,.T.);
#3056=EDGE_CURVE('',#2394,#2375,#1401,.T.);
#3057=EDGE_CURVE('',#2362,#2394,#1402,.T.);
#3058=EDGE_CURVE('',#2395,#2339,#1403,.T.);
#3059=EDGE_CURVE('',#2388,#2395,#1404,.T.);
#3060=EDGE_CURVE('',#2396,#2394,#1405,.T.);
#3061=EDGE_CURVE('',#2396,#2364,#1406,.T.);
#3062=EDGE_CURVE('',#2341,#2397,#1407,.T.);
#3063=EDGE_CURVE('',#2397,#2395,#1408,.T.);
#3064=EDGE_CURVE('',#2376,#2396,#1409,.T.);
#3065=EDGE_CURVE('',#2397,#2387,#1410,.T.);
#3066=EDGE_CURVE('',#2398,#2377,#1411,.T.);
#3067=EDGE_CURVE('',#2358,#2398,#1412,.T.);
#3068=EDGE_CURVE('',#2399,#2343,#1413,.T.);
#3069=EDGE_CURVE('',#2386,#2399,#1414,.T.);
#3070=EDGE_CURVE('',#2400,#2398,#1415,.T.);
#3071=EDGE_CURVE('',#2400,#2360,#1416,.T.);
#3072=EDGE_CURVE('',#2345,#2401,#1417,.T.);
#3073=EDGE_CURVE('',#2401,#2399,#1418,.T.);
#3074=EDGE_CURVE('',#2378,#2400,#1419,.T.);
#3075=EDGE_CURVE('',#2401,#2385,#1420,.T.);
#3076=EDGE_CURVE('',#2402,#2379,#1421,.T.);
#3077=EDGE_CURVE('',#2354,#2402,#1422,.T.);
#3078=EDGE_CURVE('',#2403,#2347,#1423,.T.);
#3079=EDGE_CURVE('',#2384,#2403,#1424,.T.);
#3080=EDGE_CURVE('',#2404,#2402,#1425,.T.);
#3081=EDGE_CURVE('',#2404,#2356,#1426,.T.);
#3082=EDGE_CURVE('',#2349,#2405,#1427,.T.);
#3083=EDGE_CURVE('',#2405,#2403,#1428,.T.);
#3084=EDGE_CURVE('',#2380,#2404,#1429,.T.);
#3085=EDGE_CURVE('',#2405,#2383,#1430,.T.);
#3086=EDGE_CURVE('',#2382,#2406,#1431,.T.);
#3087=EDGE_CURVE('',#2406,#2407,#1432,.T.);
#3088=EDGE_CURVE('',#2371,#2407,#1433,.T.);
#3089=EDGE_CURVE('',#2408,#2381,#1434,.T.);
#3090=EDGE_CURVE('',#2406,#2408,#1435,.T.);
#3091=EDGE_CURVE('',#2409,#2372,#1436,.T.);
#3092=EDGE_CURVE('',#2408,#2409,#1437,.T.);
#3093=EDGE_CURVE('',#2407,#2409,#1438,.T.);
#3094=EDGE_CURVE('',#2410,#2411,#1439,.T.);
#3095=EDGE_CURVE('',#2412,#2410,#1440,.T.);
#3096=EDGE_CURVE('',#2413,#2412,#1441,.T.);
#3097=EDGE_CURVE('',#2411,#2413,#1442,.T.);
#3098=EDGE_CURVE('',#2414,#2415,#1443,.T.);
#3099=EDGE_CURVE('',#2416,#2414,#1444,.T.);
#3100=EDGE_CURVE('',#2417,#2416,#1445,.T.);
#3101=EDGE_CURVE('',#2415,#2417,#1446,.T.);
#3102=EDGE_CURVE('',#2413,#2416,#1447,.T.);
#3103=EDGE_CURVE('',#2417,#2412,#1448,.T.);
#3104=EDGE_CURVE('',#2418,#2410,#1449,.T.);
#3105=EDGE_CURVE('',#2419,#2418,#1450,.T.);
#3106=EDGE_CURVE('',#2419,#2420,#1451,.T.);
#3107=EDGE_CURVE('',#2420,#2421,#1452,.T.);
#3108=EDGE_CURVE('',#2415,#2421,#1453,.T.);
#3109=EDGE_CURVE('',#2411,#2422,#1454,.T.);
#3110=EDGE_CURVE('',#2422,#2418,#1455,.T.);
#3111=EDGE_CURVE('',#2420,#2423,#1456,.T.);
#3112=EDGE_CURVE('',#2423,#2424,#1457,.T.);
#3113=EDGE_CURVE('',#2421,#2424,#1458,.T.);
#3114=EDGE_CURVE('',#2425,#2419,#1459,.T.);
#3115=EDGE_CURVE('',#2425,#2422,#1460,.T.);
#3116=EDGE_CURVE('',#2424,#2414,#1461,.T.);
#3117=EDGE_CURVE('',#2423,#2425,#1462,.T.);
#3118=EDGE_CURVE('',#2426,#2427,#1463,.T.);
#3119=EDGE_CURVE('',#2426,#2428,#1464,.T.);
#3120=EDGE_CURVE('',#2429,#2428,#1465,.T.);
#3121=EDGE_CURVE('',#2427,#2429,#1466,.T.);
#3122=EDGE_CURVE('',#2430,#2426,#1467,.T.);
#3123=EDGE_CURVE('',#2431,#2430,#1468,.T.);
#3124=EDGE_CURVE('',#2428,#2431,#1469,.T.);
#3125=EDGE_CURVE('',#2432,#2429,#1470,.T.);
#3126=EDGE_CURVE('',#2433,#2432,#1471,.T.);
#3127=EDGE_CURVE('',#2433,#2427,#1472,.T.);
#3128=EDGE_CURVE('',#2430,#2434,#1473,.T.);
#3129=EDGE_CURVE('',#2434,#2435,#1474,.T.);
#3130=EDGE_CURVE('',#2431,#2435,#1475,.T.);
#3131=EDGE_CURVE('',#2436,#2433,#1476,.T.);
#3132=EDGE_CURVE('',#2437,#2432,#1477,.T.);
#3133=EDGE_CURVE('',#2436,#2437,#1478,.T.);
#3134=EDGE_CURVE('',#2434,#2436,#1479,.T.);
#3135=EDGE_CURVE('',#2435,#2437,#1480,.T.);
#3136=EDGE_CURVE('',#2438,#2439,#1481,.T.);
#3137=EDGE_CURVE('',#2440,#2438,#143,.F.);
#3138=EDGE_CURVE('',#2441,#2440,#469,.T.);
#3139=EDGE_CURVE('',#2441,#2439,#144,.T.);
#3140=EDGE_CURVE('',#2442,#2443,#1482,.T.);
#3141=EDGE_CURVE('',#2438,#2442,#145,.F.);
#3142=EDGE_CURVE('',#2439,#2444,#146,.T.);
#3143=EDGE_CURVE('',#2444,#2443,#147,.T.);
#3144=EDGE_CURVE('',#2445,#2446,#1483,.T.);
#3145=EDGE_CURVE('',#2447,#2445,#148,.F.);
#3146=EDGE_CURVE('',#2442,#2447,#149,.F.);
#3147=EDGE_CURVE('',#2443,#2446,#150,.T.);
#3148=EDGE_CURVE('',#2448,#2449,#1484,.T.);
#3149=EDGE_CURVE('',#2445,#2448,#151,.F.);
#3150=EDGE_CURVE('',#2446,#2450,#152,.T.);
#3151=EDGE_CURVE('',#2450,#2449,#153,.T.);
#3152=EDGE_CURVE('',#2451,#2452,#1485,.T.);
#3153=EDGE_CURVE('',#2453,#2451,#154,.F.);
#3154=EDGE_CURVE('',#2448,#2453,#155,.F.);
#3155=EDGE_CURVE('',#2449,#2452,#156,.T.);
#3156=EDGE_CURVE('',#2454,#2455,#1486,.T.);
#3157=EDGE_CURVE('',#2451,#2454,#157,.F.);
#3158=EDGE_CURVE('',#2452,#2456,#158,.T.);
#3159=EDGE_CURVE('',#2456,#2455,#159,.T.);
#3160=EDGE_CURVE('',#2457,#2458,#1487,.T.);
#3161=EDGE_CURVE('',#2459,#2457,#160,.T.);
#3162=EDGE_CURVE('',#2454,#2459,#161,.F.);
#3163=EDGE_CURVE('',#2455,#2460,#162,.T.);
#3164=EDGE_CURVE('',#2460,#2458,#163,.T.);
#3165=EDGE_CURVE('',#2461,#2462,#1488,.T.);
#3166=EDGE_CURVE('',#2463,#2461,#164,.T.);
#3167=EDGE_CURVE('',#2457,#2463,#165,.T.);
#3168=EDGE_CURVE('',#2458,#2464,#166,.T.);
#3169=EDGE_CURVE('',#2464,#2462,#167,.T.);
#3170=EDGE_CURVE('',#2465,#2466,#1489,.T.);
#3171=EDGE_CURVE('',#2467,#2465,#168,.F.);
#3172=EDGE_CURVE('',#2461,#2467,#169,.T.);
#3173=EDGE_CURVE('',#2462,#2466,#170,.T.);
#3174=EDGE_CURVE('',#2468,#2469,#1490,.T.);
#3175=EDGE_CURVE('',#2465,#2468,#171,.F.);
#3176=EDGE_CURVE('',#2466,#2470,#172,.T.);
#3177=EDGE_CURVE('',#2470,#2469,#173,.T.);
#3178=EDGE_CURVE('',#2471,#2472,#1491,.T.);
#3179=EDGE_CURVE('',#2473,#2471,#174,.F.);
#3180=EDGE_CURVE('',#2468,#2473,#175,.F.);
#3181=EDGE_CURVE('',#2469,#2472,#176,.T.);
#3182=EDGE_CURVE('',#2474,#2475,#1492,.T.);
#3183=EDGE_CURVE('',#2471,#2474,#177,.F.);
#3184=EDGE_CURVE('',#2472,#2476,#178,.T.);
#3185=EDGE_CURVE('',#2476,#2475,#179,.T.);
#3186=EDGE_CURVE('',#2477,#2478,#1493,.T.);
#3187=EDGE_CURVE('',#2479,#2477,#180,.F.);
#3188=EDGE_CURVE('',#2474,#2479,#181,.F.);
#3189=EDGE_CURVE('',#2475,#2478,#182,.T.);
#3190=EDGE_CURVE('',#2480,#2481,#1494,.T.);
#3191=EDGE_CURVE('',#2477,#2480,#183,.F.);
#3192=EDGE_CURVE('',#2478,#2482,#184,.T.);
#3193=EDGE_CURVE('',#2482,#2481,#185,.T.);
#3194=EDGE_CURVE('',#2483,#2484,#1495,.T.);
#3195=EDGE_CURVE('',#2485,#2483,#186,.F.);
#3196=EDGE_CURVE('',#2480,#2485,#187,.F.);
#3197=EDGE_CURVE('',#2481,#2484,#188,.T.);
#3198=EDGE_CURVE('',#2486,#2487,#1496,.T.);
#3199=EDGE_CURVE('',#2483,#2486,#189,.F.);
#3200=EDGE_CURVE('',#2484,#2488,#190,.T.);
#3201=EDGE_CURVE('',#2488,#2487,#191,.T.);
#3202=EDGE_CURVE('',#2489,#2490,#1497,.T.);
#3203=EDGE_CURVE('',#2491,#2489,#192,.F.);
#3204=EDGE_CURVE('',#2486,#2491,#193,.F.);
#3205=EDGE_CURVE('',#2487,#2490,#194,.T.);
#3206=EDGE_CURVE('',#2492,#2493,#1498,.T.);
#3207=EDGE_CURVE('',#2489,#2492,#195,.F.);
#3208=EDGE_CURVE('',#2490,#2494,#196,.T.);
#3209=EDGE_CURVE('',#2494,#2493,#197,.T.);
#3210=EDGE_CURVE('',#2495,#2496,#1499,.T.);
#3211=EDGE_CURVE('',#2497,#2495,#198,.T.);
#3212=EDGE_CURVE('',#2492,#2497,#199,.F.);
#3213=EDGE_CURVE('',#2493,#2498,#200,.T.);
#3214=EDGE_CURVE('',#2498,#2496,#201,.T.);
#3215=EDGE_CURVE('',#2499,#2500,#1500,.T.);
#3216=EDGE_CURVE('',#2501,#2499,#202,.T.);
#3217=EDGE_CURVE('',#2495,#2501,#203,.T.);
#3218=EDGE_CURVE('',#2496,#2502,#204,.T.);
#3219=EDGE_CURVE('',#2502,#2500,#205,.T.);
#3220=EDGE_CURVE('',#2503,#2504,#1501,.T.);
#3221=EDGE_CURVE('',#2505,#2503,#206,.F.);
#3222=EDGE_CURVE('',#2499,#2505,#207,.T.);
#3223=EDGE_CURVE('',#2500,#2504,#208,.T.);
#3224=EDGE_CURVE('',#2506,#2507,#1502,.T.);
#3225=EDGE_CURVE('',#2503,#2506,#209,.F.);
#3226=EDGE_CURVE('',#2504,#2508,#210,.T.);
#3227=EDGE_CURVE('',#2508,#2507,#211,.T.);
#3228=EDGE_CURVE('',#2509,#2510,#1503,.T.);
#3229=EDGE_CURVE('',#2511,#2509,#212,.F.);
#3230=EDGE_CURVE('',#2506,#2511,#213,.F.);
#3231=EDGE_CURVE('',#2507,#2510,#214,.T.);
#3232=EDGE_CURVE('',#2512,#2513,#1504,.T.);
#3233=EDGE_CURVE('',#2509,#2512,#215,.F.);
#3234=EDGE_CURVE('',#2510,#2514,#216,.T.);
#3235=EDGE_CURVE('',#2514,#2513,#217,.T.);
#3236=EDGE_CURVE('',#2515,#2516,#1505,.T.);
#3237=EDGE_CURVE('',#2517,#2515,#218,.F.);
#3238=EDGE_CURVE('',#2512,#2517,#219,.F.);
#3239=EDGE_CURVE('',#2513,#2516,#220,.T.);
#3240=EDGE_CURVE('',#2518,#2519,#1506,.T.);
#3241=EDGE_CURVE('',#2515,#2518,#221,.F.);
#3242=EDGE_CURVE('',#2516,#2520,#222,.T.);
#3243=EDGE_CURVE('',#2520,#2519,#223,.T.);
#3244=EDGE_CURVE('',#2521,#2522,#1507,.T.);
#3245=EDGE_CURVE('',#2523,#2521,#224,.F.);
#3246=EDGE_CURVE('',#2518,#2523,#225,.F.);
#3247=EDGE_CURVE('',#2519,#2522,#226,.T.);
#3248=EDGE_CURVE('',#2524,#2525,#1508,.T.);
#3249=EDGE_CURVE('',#2521,#2524,#227,.F.);
#3250=EDGE_CURVE('',#2522,#2526,#228,.T.);
#3251=EDGE_CURVE('',#2526,#2525,#229,.T.);
#3252=EDGE_CURVE('',#2527,#2528,#1509,.T.);
#3253=EDGE_CURVE('',#2529,#2527,#230,.F.);
#3254=EDGE_CURVE('',#2524,#2529,#231,.F.);
#3255=EDGE_CURVE('',#2525,#2530,#232,.T.);
#3256=EDGE_CURVE('',#2530,#2528,#233,.T.);
#3257=EDGE_CURVE('',#2531,#2532,#1510,.T.);
#3258=EDGE_CURVE('',#2527,#2531,#234,.F.);
#3259=EDGE_CURVE('',#2528,#2532,#235,.T.);
#3260=EDGE_CURVE('',#2533,#2534,#1511,.T.);
#3261=EDGE_CURVE('',#2535,#2533,#236,.T.);
#3262=EDGE_CURVE('',#2531,#2535,#237,.F.);
#3263=EDGE_CURVE('',#2532,#2536,#238,.T.);
#3264=EDGE_CURVE('',#2536,#2534,#239,.T.);
#3265=EDGE_CURVE('',#2537,#2538,#1512,.T.);
#3266=EDGE_CURVE('',#2539,#2537,#240,.T.);
#3267=EDGE_CURVE('',#2533,#2539,#241,.T.);
#3268=EDGE_CURVE('',#2534,#2538,#242,.T.);
#3269=EDGE_CURVE('',#2540,#2541,#1513,.T.);
#3270=EDGE_CURVE('',#2542,#2540,#243,.F.);
#3271=EDGE_CURVE('',#2537,#2542,#244,.T.);
#3272=EDGE_CURVE('',#2538,#2543,#245,.T.);
#3273=EDGE_CURVE('',#2543,#2541,#246,.T.);
#3274=EDGE_CURVE('',#2544,#2545,#1514,.T.);
#3275=EDGE_CURVE('',#2540,#2544,#247,.F.);
#3276=EDGE_CURVE('',#2541,#2546,#248,.T.);
#3277=EDGE_CURVE('',#2546,#2545,#249,.F.);
#3278=EDGE_CURVE('',#2547,#2548,#250,.T.);
#3279=EDGE_CURVE('',#2548,#2549,#470,.F.);
#3280=EDGE_CURVE('',#2549,#2550,#251,.T.);
#3281=EDGE_CURVE('',#2550,#2551,#252,.T.);
#3282=EDGE_CURVE('',#2551,#2552,#253,.T.);
#3283=EDGE_CURVE('',#2552,#2553,#254,.T.);
#3284=EDGE_CURVE('',#2553,#2554,#255,.T.);
#3285=EDGE_CURVE('',#2554,#2555,#256,.T.);
#3286=EDGE_CURVE('',#2555,#2556,#257,.T.);
#3287=EDGE_CURVE('',#2556,#2557,#258,.T.);
#3288=EDGE_CURVE('',#2557,#2558,#259,.T.);
#3289=EDGE_CURVE('',#2558,#2559,#260,.T.);
#3290=EDGE_CURVE('',#2559,#2560,#261,.T.);
#3291=EDGE_CURVE('',#2560,#2561,#262,.T.);
#3292=EDGE_CURVE('',#2561,#2562,#263,.T.);
#3293=EDGE_CURVE('',#2562,#2563,#264,.T.);
#3294=EDGE_CURVE('',#2563,#2564,#265,.T.);
#3295=EDGE_CURVE('',#2564,#2565,#266,.T.);
#3296=EDGE_CURVE('',#2565,#2566,#267,.T.);
#3297=EDGE_CURVE('',#2566,#2567,#268,.T.);
#3298=EDGE_CURVE('',#2567,#2568,#269,.T.);
#3299=EDGE_CURVE('',#2568,#2569,#270,.T.);
#3300=EDGE_CURVE('',#2569,#2570,#271,.T.);
#3301=EDGE_CURVE('',#2570,#2571,#272,.T.);
#3302=EDGE_CURVE('',#2571,#2572,#273,.T.);
#3303=EDGE_CURVE('',#2572,#2573,#274,.T.);
#3304=EDGE_CURVE('',#2573,#2574,#275,.T.);
#3305=EDGE_CURVE('',#2574,#2575,#276,.T.);
#3306=EDGE_CURVE('',#2575,#2576,#277,.T.);
#3307=EDGE_CURVE('',#2576,#2577,#278,.T.);
#3308=EDGE_CURVE('',#2577,#2578,#279,.T.);
#3309=EDGE_CURVE('',#2578,#2579,#280,.T.);
#3310=EDGE_CURVE('',#2579,#2580,#281,.T.);
#3311=EDGE_CURVE('',#2580,#2581,#282,.T.);
#3312=EDGE_CURVE('',#2581,#2582,#283,.T.);
#3313=EDGE_CURVE('',#2582,#2583,#284,.T.);
#3314=EDGE_CURVE('',#2583,#2584,#285,.T.);
#3315=EDGE_CURVE('',#2584,#2585,#286,.T.);
#3316=EDGE_CURVE('',#2586,#2585,#471,.F.);
#3317=EDGE_CURVE('',#2586,#2587,#287,.T.);
#3318=EDGE_CURVE('',#2587,#2588,#288,.T.);
#3319=EDGE_CURVE('',#2588,#2589,#289,.T.);
#3320=EDGE_CURVE('',#2589,#2590,#290,.T.);
#3321=EDGE_CURVE('',#2590,#2591,#291,.T.);
#3322=EDGE_CURVE('',#2591,#2592,#292,.T.);
#3323=EDGE_CURVE('',#2592,#2593,#293,.T.);
#3324=EDGE_CURVE('',#2593,#2594,#294,.T.);
#3325=EDGE_CURVE('',#2594,#2595,#295,.T.);
#3326=EDGE_CURVE('',#2595,#2596,#296,.T.);
#3327=EDGE_CURVE('',#2596,#2597,#297,.T.);
#3328=EDGE_CURVE('',#2597,#2598,#298,.T.);
#3329=EDGE_CURVE('',#2598,#2599,#299,.T.);
#3330=EDGE_CURVE('',#2599,#2600,#300,.T.);
#3331=EDGE_CURVE('',#2600,#2601,#301,.T.);
#3332=EDGE_CURVE('',#2601,#2602,#302,.T.);
#3333=EDGE_CURVE('',#2602,#2603,#303,.T.);
#3334=EDGE_CURVE('',#2603,#2604,#304,.T.);
#3335=EDGE_CURVE('',#2604,#2605,#305,.T.);
#3336=EDGE_CURVE('',#2605,#2606,#306,.T.);
#3337=EDGE_CURVE('',#2606,#2607,#307,.T.);
#3338=EDGE_CURVE('',#2607,#2608,#308,.T.);
#3339=EDGE_CURVE('',#2608,#2609,#309,.T.);
#3340=EDGE_CURVE('',#2609,#2610,#310,.T.);
#3341=EDGE_CURVE('',#2610,#2611,#311,.T.);
#3342=EDGE_CURVE('',#2611,#2612,#312,.T.);
#3343=EDGE_CURVE('',#2612,#2613,#313,.T.);
#3344=EDGE_CURVE('',#2613,#2614,#314,.T.);
#3345=EDGE_CURVE('',#2614,#2615,#315,.T.);
#3346=EDGE_CURVE('',#2615,#2616,#316,.T.);
#3347=EDGE_CURVE('',#2616,#2617,#317,.T.);
#3348=EDGE_CURVE('',#2617,#2618,#318,.T.);
#3349=EDGE_CURVE('',#2618,#2619,#319,.T.);
#3350=EDGE_CURVE('',#2619,#2547,#320,.T.);
#3351=EDGE_CURVE('',#2545,#2620,#321,.F.);
#3352=EDGE_CURVE('',#2621,#2620,#472,.T.);
#3353=EDGE_CURVE('',#2622,#2621,#322,.T.);
#3354=EDGE_CURVE('',#2544,#2622,#323,.F.);
#3355=EDGE_CURVE('',#2585,#2621,#324,.T.);
#3356=EDGE_CURVE('',#2623,#2549,#325,.T.);
#3357=EDGE_CURVE('',#2623,#2440,#326,.T.);
#3358=EDGE_CURVE('',#2624,#2586,#327,.T.);
#3359=EDGE_CURVE('',#2620,#2624,#328,.T.);
#3360=EDGE_CURVE('',#2548,#2441,#329,.T.);
#3361=EDGE_CURVE('',#2625,#2626,#1515,.T.);
#3362=EDGE_CURVE('',#2625,#2627,#1516,.T.);
#3363=EDGE_CURVE('',#2627,#2628,#1517,.T.);
#3364=EDGE_CURVE('',#2626,#2628,#1518,.T.);
#3365=EDGE_CURVE('',#2629,#2625,#1519,.T.);
#3366=EDGE_CURVE('',#2629,#2630,#1520,.T.);
#3367=EDGE_CURVE('',#2630,#2627,#1521,.T.);
#3368=EDGE_CURVE('',#2631,#2629,#1522,.T.);
#3369=EDGE_CURVE('',#2631,#2632,#1523,.T.);
#3370=EDGE_CURVE('',#2632,#2630,#1524,.T.);
#3371=EDGE_CURVE('',#2633,#2631,#1525,.T.);
#3372=EDGE_CURVE('',#2633,#2634,#1526,.T.);
#3373=EDGE_CURVE('',#2634,#2632,#1527,.T.);
#3374=EDGE_CURVE('',#2635,#2633,#1528,.T.);
#3375=EDGE_CURVE('',#2635,#2636,#1529,.T.);
#3376=EDGE_CURVE('',#2636,#2634,#1530,.T.);
#3377=EDGE_CURVE('',#2626,#2635,#1531,.T.);
#3378=EDGE_CURVE('',#2628,#2636,#1532,.T.);
#3379=EDGE_CURVE('',#2637,#2637,#473,.T.);
#3380=EDGE_CURVE('',#2637,#2638,#1533,.T.);
#3381=EDGE_CURVE('',#2638,#2638,#474,.T.);
#3382=EDGE_CURVE('',#2639,#2640,#1534,.T.);
#3383=EDGE_CURVE('',#2640,#2641,#330,.T.);
#3384=EDGE_CURVE('',#2642,#2641,#475,.T.);
#3385=EDGE_CURVE('',#2639,#2642,#331,.T.);
#3386=EDGE_CURVE('',#2643,#2644,#1535,.T.);
#3387=EDGE_CURVE('',#2644,#2645,#332,.T.);
#3388=EDGE_CURVE('',#2645,#2640,#333,.T.);
#3389=EDGE_CURVE('',#2646,#2639,#334,.T.);
#3390=EDGE_CURVE('',#2643,#2646,#335,.T.);
#3391=EDGE_CURVE('',#2647,#2648,#1536,.T.);
#3392=EDGE_CURVE('',#2648,#2649,#336,.T.);
#3393=EDGE_CURVE('',#2649,#2644,#337,.T.);
#3394=EDGE_CURVE('',#2650,#2643,#338,.T.);
#3395=EDGE_CURVE('',#2647,#2650,#339,.T.);
#3396=EDGE_CURVE('',#2651,#2652,#1537,.T.);
#3397=EDGE_CURVE('',#2652,#2653,#340,.T.);
#3398=EDGE_CURVE('',#2653,#2648,#341,.T.);
#3399=EDGE_CURVE('',#2654,#2647,#342,.T.);
#3400=EDGE_CURVE('',#2651,#2654,#343,.T.);
#3401=EDGE_CURVE('',#2655,#2656,#1538,.T.);
#3402=EDGE_CURVE('',#2656,#2657,#344,.T.);
#3403=EDGE_CURVE('',#2657,#2652,#345,.T.);
#3404=EDGE_CURVE('',#2658,#2651,#346,.T.);
#3405=EDGE_CURVE('',#2655,#2658,#347,.T.);
#3406=EDGE_CURVE('',#2659,#2660,#1539,.T.);
#3407=EDGE_CURVE('',#2661,#2659,#348,.T.);
#3408=EDGE_CURVE('',#2662,#2661,#349,.T.);
#3409=EDGE_CURVE('',#2663,#2662,#476,.T.);
#3410=EDGE_CURVE('',#2663,#2664,#350,.T.);
#3411=EDGE_CURVE('',#2664,#2660,#351,.T.);
#3412=EDGE_CURVE('',#2665,#2666,#1540,.T.);
#3413=EDGE_CURVE('',#2667,#2666,#477,.F.);
#3414=EDGE_CURVE('',#2667,#2665,#352,.T.);
#3415=EDGE_CURVE('',#2668,#2669,#1541,.T.);
#3416=EDGE_CURVE('',#2669,#2670,#353,.T.);
#3417=EDGE_CURVE('',#2666,#2670,#478,.F.);
#3418=EDGE_CURVE('',#2665,#2671,#354,.T.);
#3419=EDGE_CURVE('',#2671,#2668,#355,.T.);
#3420=EDGE_CURVE('',#2672,#2673,#1542,.T.);
#3421=EDGE_CURVE('',#2673,#2674,#356,.T.);
#3422=EDGE_CURVE('',#2674,#2669,#357,.T.);
#3423=EDGE_CURVE('',#2668,#2672,#358,.T.);
#3424=EDGE_CURVE('',#2675,#2676,#1543,.T.);
#3425=EDGE_CURVE('',#2676,#2673,#359,.T.);
#3426=EDGE_CURVE('',#2672,#2677,#360,.T.);
#3427=EDGE_CURVE('',#2677,#2675,#361,.T.);
#3428=EDGE_CURVE('',#2678,#2679,#1544,.T.);
#3429=EDGE_CURVE('',#2679,#2680,#362,.T.);
#3430=EDGE_CURVE('',#2680,#2676,#363,.T.);
#3431=EDGE_CURVE('',#2675,#2678,#364,.T.);
#3432=EDGE_CURVE('',#2681,#2682,#1545,.T.);
#3433=EDGE_CURVE('',#2681,#2683,#365,.T.);
#3434=EDGE_CURVE('',#2683,#2684,#366,.T.);
#3435=EDGE_CURVE('',#2685,#2684,#479,.T.);
#3436=EDGE_CURVE('',#2685,#2686,#367,.T.);
#3437=EDGE_CURVE('',#2686,#2682,#368,.T.);
#3438=EDGE_CURVE('',#2682,#2687,#369,.T.);
#3439=EDGE_CURVE('',#2687,#2679,#370,.T.);
#3440=EDGE_CURVE('',#2678,#2688,#371,.T.);
#3441=EDGE_CURVE('',#2688,#2681,#372,.T.);
#3442=EDGE_CURVE('',#2660,#2689,#373,.T.);
#3443=EDGE_CURVE('',#2689,#2656,#374,.T.);
#3444=EDGE_CURVE('',#2690,#2655,#375,.T.);
#3445=EDGE_CURVE('',#2659,#2690,#376,.T.);
#3446=EDGE_CURVE('',#2641,#2667,#377,.T.);
#3447=EDGE_CURVE('',#2684,#2663,#378,.T.);
#3448=EDGE_CURVE('',#2670,#2642,#379,.T.);
#3449=EDGE_CURVE('',#2662,#2685,#380,.T.);
#3450=EDGE_CURVE('',#2691,#2692,#1546,.T.);
#3451=EDGE_CURVE('',#2692,#2693,#1547,.T.);
#3452=EDGE_CURVE('',#2693,#2694,#1548,.T.);
#3453=EDGE_CURVE('',#2694,#2695,#1549,.T.);
#3454=EDGE_CURVE('',#2695,#2696,#1550,.T.);
#3455=EDGE_CURVE('',#2696,#2691,#1551,.T.);
#3456=EDGE_CURVE('',#2697,#2698,#1552,.T.);
#3457=EDGE_CURVE('',#2698,#2691,#1553,.T.);
#3458=EDGE_CURVE('',#2697,#2696,#1554,.T.);
#3459=EDGE_CURVE('',#2699,#2697,#1555,.T.);
#3460=EDGE_CURVE('',#2699,#2695,#1556,.T.);
#3461=EDGE_CURVE('',#2700,#2699,#1557,.T.);
#3462=EDGE_CURVE('',#2700,#2694,#1558,.T.);
#3463=EDGE_CURVE('',#2701,#2700,#1559,.T.);
#3464=EDGE_CURVE('',#2701,#2693,#1560,.T.);
#3465=EDGE_CURVE('',#2702,#2701,#1561,.T.);
#3466=EDGE_CURVE('',#2702,#2692,#1562,.T.);
#3467=EDGE_CURVE('',#2698,#2702,#1563,.T.);
#3468=EDGE_CURVE('',#2703,#2703,#480,.T.);
#3469=EDGE_CURVE('',#2703,#2704,#1564,.T.);
#3470=EDGE_CURVE('',#2704,#2704,#481,.T.);
#3471=EDGE_CURVE('',#2705,#2705,#482,.T.);
#3472=EDGE_CURVE('',#2705,#2706,#1565,.T.);
#3473=EDGE_CURVE('',#2706,#2706,#483,.T.);
#3474=EDGE_CURVE('',#2707,#2707,#484,.T.);
#3475=EDGE_CURVE('',#2707,#2708,#1566,.T.);
#3476=EDGE_CURVE('',#2708,#2708,#485,.T.);
#3477=EDGE_CURVE('',#2709,#2709,#486,.T.);
#3478=EDGE_CURVE('',#2709,#2710,#1567,.T.);
#3479=EDGE_CURVE('',#2710,#2710,#487,.T.);
#3480=EDGE_CURVE('',#2711,#2712,#1568,.T.);
#3481=EDGE_CURVE('',#2713,#2711,#1569,.T.);
#3482=EDGE_CURVE('',#2714,#2713,#1570,.T.);
#3483=EDGE_CURVE('',#2712,#2714,#1571,.T.);
#3484=EDGE_CURVE('',#2715,#2716,#1572,.T.);
#3485=EDGE_CURVE('',#2717,#2715,#1573,.T.);
#3486=EDGE_CURVE('',#2718,#2717,#1574,.T.);
#3487=EDGE_CURVE('',#2716,#2718,#1575,.T.);
#3488=EDGE_CURVE('',#2719,#2720,#1576,.T.);
#3489=EDGE_CURVE('',#2721,#2719,#1577,.T.);
#3490=EDGE_CURVE('',#2722,#2721,#1578,.T.);
#3491=EDGE_CURVE('',#2720,#2722,#1579,.T.);
#3492=EDGE_CURVE('',#2723,#2724,#1580,.T.);
#3493=EDGE_CURVE('',#2725,#2723,#1581,.T.);
#3494=EDGE_CURVE('',#2726,#2725,#1582,.T.);
#3495=EDGE_CURVE('',#2724,#2726,#1583,.T.);
#3496=EDGE_CURVE('',#2727,#2728,#1584,.T.);
#3497=EDGE_CURVE('',#2729,#2727,#1585,.T.);
#3498=EDGE_CURVE('',#2730,#2729,#1586,.T.);
#3499=EDGE_CURVE('',#2730,#2728,#1587,.T.);
#3500=EDGE_CURVE('',#2731,#2732,#1588,.T.);
#3501=EDGE_CURVE('',#2733,#2731,#1589,.T.);
#3502=EDGE_CURVE('',#2734,#2733,#1590,.T.);
#3503=EDGE_CURVE('',#2734,#2732,#1591,.T.);
#3504=EDGE_CURVE('',#2735,#2736,#1592,.T.);
#3505=EDGE_CURVE('',#2737,#2735,#1593,.T.);
#3506=EDGE_CURVE('',#2738,#2737,#1594,.T.);
#3507=EDGE_CURVE('',#2738,#2736,#1595,.T.);
#3508=EDGE_CURVE('',#2739,#2740,#1596,.T.);
#3509=EDGE_CURVE('',#2741,#2739,#1597,.T.);
#3510=EDGE_CURVE('',#2742,#2741,#1598,.T.);
#3511=EDGE_CURVE('',#2742,#2740,#1599,.T.);
#3512=EDGE_CURVE('',#2743,#2723,#1600,.T.);
#3513=EDGE_CURVE('',#2744,#2743,#1601,.T.);
#3514=EDGE_CURVE('',#2745,#2744,#1602,.T.);
#3515=EDGE_CURVE('',#2746,#2745,#1603,.T.);
#3516=EDGE_CURVE('',#2740,#2746,#1604,.T.);
#3517=EDGE_CURVE('',#2742,#2747,#1605,.T.);
#3518=EDGE_CURVE('',#2748,#2747,#1606,.T.);
#3519=EDGE_CURVE('',#2736,#2748,#1607,.T.);
#3520=EDGE_CURVE('',#2738,#2749,#1608,.T.);
#3521=EDGE_CURVE('',#2750,#2749,#1609,.T.);
#3522=EDGE_CURVE('',#2732,#2750,#1610,.T.);
#3523=EDGE_CURVE('',#2734,#2751,#1611,.T.);
#3524=EDGE_CURVE('',#2752,#2751,#1612,.T.);
#3525=EDGE_CURVE('',#2728,#2752,#1613,.T.);
#3526=EDGE_CURVE('',#2730,#2753,#1614,.T.);
#3527=EDGE_CURVE('',#2754,#2753,#1615,.T.);
#3528=EDGE_CURVE('',#2755,#2754,#1616,.T.);
#3529=EDGE_CURVE('',#2756,#2755,#1617,.T.);
#3530=EDGE_CURVE('',#2756,#2721,#1618,.T.);
#3531=EDGE_CURVE('',#2757,#2719,#1619,.T.);
#3532=EDGE_CURVE('',#2758,#2757,#1620,.T.);
#3533=EDGE_CURVE('',#2758,#2717,#1621,.T.);
#3534=EDGE_CURVE('',#2759,#2715,#1622,.T.);
#3535=EDGE_CURVE('',#2760,#2759,#1623,.T.);
#3536=EDGE_CURVE('',#2760,#2713,#1624,.T.);
#3537=EDGE_CURVE('',#2761,#2711,#1625,.T.);
#3538=EDGE_CURVE('',#2762,#2761,#1626,.T.);
#3539=EDGE_CURVE('',#2762,#2725,#1627,.T.);
#3540=EDGE_CURVE('',#2763,#2746,#1628,.T.);
#3541=EDGE_CURVE('',#2739,#2763,#1629,.T.);
#3542=EDGE_CURVE('',#2764,#2724,#1630,.T.);
#3543=EDGE_CURVE('',#2743,#2764,#1631,.T.);
#3544=EDGE_CURVE('',#2765,#2763,#1632,.T.);
#3545=EDGE_CURVE('',#2765,#2741,#1633,.T.);
#3546=EDGE_CURVE('',#2726,#2766,#1634,.T.);
#3547=EDGE_CURVE('',#2766,#2764,#1635,.T.);
#3548=EDGE_CURVE('',#2747,#2765,#1636,.T.);
#3549=EDGE_CURVE('',#2766,#2762,#1637,.T.);
#3550=EDGE_CURVE('',#2767,#2748,#1638,.T.);
#3551=EDGE_CURVE('',#2735,#2767,#1639,.T.);
#3552=EDGE_CURVE('',#2768,#2712,#1640,.T.);
#3553=EDGE_CURVE('',#2761,#2768,#1641,.T.);
#3554=EDGE_CURVE('',#2769,#2767,#1642,.T.);
#3555=EDGE_CURVE('',#2769,#2737,#1643,.T.);
#3556=EDGE_CURVE('',#2714,#2770,#1644,.T.);
#3557=EDGE_CURVE('',#2770,#2768,#1645,.T.);
#3558=EDGE_CURVE('',#2749,#2769,#1646,.T.);
#3559=EDGE_CURVE('',#2770,#2760,#1647,.T.);
#3560=EDGE_CURVE('',#2771,#2750,#1648,.T.);
#3561=EDGE_CURVE('',#2731,#2771,#1649,.T.);
#3562=EDGE_CURVE('',#2772,#2716,#1650,.T.);
#3563=EDGE_CURVE('',#2759,#2772,#1651,.T.);
#3564=EDGE_CURVE('',#2773,#2771,#1652,.T.);
#3565=EDGE_CURVE('',#2773,#2733,#1653,.T.);
#3566=EDGE_CURVE('',#2718,#2774,#1654,.T.);
#3567=EDGE_CURVE('',#2774,#2772,#1655,.T.);
#3568=EDGE_CURVE('',#2751,#2773,#1656,.T.);
#3569=EDGE_CURVE('',#2774,#2758,#1657,.T.);
#3570=EDGE_CURVE('',#2775,#2752,#1658,.T.);
#3571=EDGE_CURVE('',#2727,#2775,#1659,.T.);
#3572=EDGE_CURVE('',#2776,#2720,#1660,.T.);
#3573=EDGE_CURVE('',#2757,#2776,#1661,.T.);
#3574=EDGE_CURVE('',#2777,#2775,#1662,.T.);
#3575=EDGE_CURVE('',#2777,#2729,#1663,.T.);
#3576=EDGE_CURVE('',#2722,#2778,#1664,.T.);
#3577=EDGE_CURVE('',#2778,#2776,#1665,.T.);
#3578=EDGE_CURVE('',#2753,#2777,#1666,.T.);
#3579=EDGE_CURVE('',#2778,#2756,#1667,.T.);
#3580=EDGE_CURVE('',#2755,#2779,#1668,.T.);
#3581=EDGE_CURVE('',#2779,#2780,#1669,.T.);
#3582=EDGE_CURVE('',#2744,#2780,#1670,.T.);
#3583=EDGE_CURVE('',#2781,#2754,#1671,.T.);
#3584=EDGE_CURVE('',#2779,#2781,#1672,.T.);
#3585=EDGE_CURVE('',#2782,#2745,#1673,.T.);
#3586=EDGE_CURVE('',#2781,#2782,#1674,.T.);
#3587=EDGE_CURVE('',#2780,#2782,#1675,.T.);
#3588=EDGE_CURVE('',#2783,#2784,#1676,.T.);
#3589=EDGE_CURVE('',#2785,#2783,#1677,.T.);
#3590=EDGE_CURVE('',#2786,#2785,#1678,.T.);
#3591=EDGE_CURVE('',#2784,#2786,#1679,.T.);
#3592=EDGE_CURVE('',#2787,#2788,#1680,.T.);
#3593=EDGE_CURVE('',#2789,#2787,#1681,.T.);
#3594=EDGE_CURVE('',#2790,#2789,#1682,.T.);
#3595=EDGE_CURVE('',#2788,#2790,#1683,.T.);
#3596=EDGE_CURVE('',#2786,#2789,#1684,.T.);
#3597=EDGE_CURVE('',#2790,#2785,#1685,.T.);
#3598=EDGE_CURVE('',#2791,#2783,#1686,.T.);
#3599=EDGE_CURVE('',#2792,#2791,#1687,.T.);
#3600=EDGE_CURVE('',#2792,#2793,#1688,.T.);
#3601=EDGE_CURVE('',#2793,#2794,#1689,.T.);
#3602=EDGE_CURVE('',#2788,#2794,#1690,.T.);
#3603=EDGE_CURVE('',#2784,#2795,#1691,.T.);
#3604=EDGE_CURVE('',#2795,#2791,#1692,.T.);
#3605=EDGE_CURVE('',#2793,#2796,#1693,.T.);
#3606=EDGE_CURVE('',#2796,#2797,#1694,.T.);
#3607=EDGE_CURVE('',#2794,#2797,#1695,.T.);
#3608=EDGE_CURVE('',#2798,#2792,#1696,.T.);
#3609=EDGE_CURVE('',#2798,#2795,#1697,.T.);
#3610=EDGE_CURVE('',#2797,#2787,#1698,.T.);
#3611=EDGE_CURVE('',#2796,#2798,#1699,.T.);
#3612=EDGE_CURVE('',#2799,#2800,#1700,.T.);
#3613=EDGE_CURVE('',#2800,#2801,#1701,.T.);
#3614=EDGE_CURVE('',#2802,#2801,#1702,.T.);
#3615=EDGE_CURVE('',#2799,#2802,#1703,.T.);
#3616=EDGE_CURVE('',#2803,#2799,#1704,.T.);
#3617=EDGE_CURVE('',#2804,#2802,#1705,.T.);
#3618=EDGE_CURVE('',#2803,#2804,#1706,.T.);
#3619=EDGE_CURVE('',#2805,#2803,#1707,.T.);
#3620=EDGE_CURVE('',#2806,#2804,#1708,.T.);
#3621=EDGE_CURVE('',#2805,#2806,#1709,.T.);
#3622=EDGE_CURVE('',#2800,#2805,#1710,.T.);
#3623=EDGE_CURVE('',#2801,#2806,#1711,.T.);
#3624=EDGE_CURVE('',#2807,#2807,#488,.T.);
#3625=EDGE_CURVE('',#2807,#2808,#1712,.T.);
#3626=EDGE_CURVE('',#2808,#2808,#489,.T.);
#3627=ORIENTED_EDGE('',*,*,#2809,.T.);
#3628=ORIENTED_EDGE('',*,*,#2810,.T.);
#3629=ORIENTED_EDGE('',*,*,#2811,.F.);
#3630=ORIENTED_EDGE('',*,*,#2812,.F.);
#3631=ORIENTED_EDGE('',*,*,#2813,.T.);
#3632=ORIENTED_EDGE('',*,*,#2812,.T.);
#3633=ORIENTED_EDGE('',*,*,#2814,.F.);
#3634=ORIENTED_EDGE('',*,*,#2815,.F.);
#3635=ORIENTED_EDGE('',*,*,#2816,.T.);
#3636=ORIENTED_EDGE('',*,*,#2815,.T.);
#3637=ORIENTED_EDGE('',*,*,#2817,.F.);
#3638=ORIENTED_EDGE('',*,*,#2818,.F.);
#3639=ORIENTED_EDGE('',*,*,#2819,.T.);
#3640=ORIENTED_EDGE('',*,*,#2818,.T.);
#3641=ORIENTED_EDGE('',*,*,#2820,.F.);
#3642=ORIENTED_EDGE('',*,*,#2810,.F.);
#3643=ORIENTED_EDGE('',*,*,#2820,.T.);
#3644=ORIENTED_EDGE('',*,*,#2817,.T.);
#3645=ORIENTED_EDGE('',*,*,#2814,.T.);
#3646=ORIENTED_EDGE('',*,*,#2811,.T.);
#3647=ORIENTED_EDGE('',*,*,#2819,.F.);
#3648=ORIENTED_EDGE('',*,*,#2809,.F.);
#3649=ORIENTED_EDGE('',*,*,#2813,.F.);
#3650=ORIENTED_EDGE('',*,*,#2816,.F.);
#3651=ORIENTED_EDGE('',*,*,#2821,.F.);
#3652=ORIENTED_EDGE('',*,*,#2822,.T.);
#3653=ORIENTED_EDGE('',*,*,#2823,.F.);
#3654=ORIENTED_EDGE('',*,*,#2824,.F.);
#3655=ORIENTED_EDGE('',*,*,#2825,.F.);
#3656=ORIENTED_EDGE('',*,*,#2826,.T.);
#3657=ORIENTED_EDGE('',*,*,#2827,.F.);
#3658=ORIENTED_EDGE('',*,*,#2822,.F.);
#3659=ORIENTED_EDGE('',*,*,#2828,.F.);
#3660=ORIENTED_EDGE('',*,*,#2829,.T.);
#3661=ORIENTED_EDGE('',*,*,#2830,.F.);
#3662=ORIENTED_EDGE('',*,*,#2826,.F.);
#3663=ORIENTED_EDGE('',*,*,#2831,.F.);
#3664=ORIENTED_EDGE('',*,*,#2824,.T.);
#3665=ORIENTED_EDGE('',*,*,#2832,.F.);
#3666=ORIENTED_EDGE('',*,*,#2829,.F.);
#3667=ORIENTED_EDGE('',*,*,#2833,.F.);
#3668=ORIENTED_EDGE('',*,*,#2834,.T.);
#3669=ORIENTED_EDGE('',*,*,#2835,.F.);
#3670=ORIENTED_EDGE('',*,*,#2834,.F.);
#3671=ORIENTED_EDGE('',*,*,#2836,.F.);
#3672=ORIENTED_EDGE('',*,*,#2837,.T.);
#3673=ORIENTED_EDGE('',*,*,#2838,.F.);
#3674=ORIENTED_EDGE('',*,*,#2837,.F.);
#3675=ORIENTED_EDGE('',*,*,#2839,.T.);
#3676=ORIENTED_EDGE('',*,*,#2840,.T.);
#3677=ORIENTED_EDGE('',*,*,#2841,.F.);
#3678=ORIENTED_EDGE('',*,*,#2842,.F.);
#3679=ORIENTED_EDGE('',*,*,#2821,.T.);
#3680=ORIENTED_EDGE('',*,*,#2831,.T.);
#3681=ORIENTED_EDGE('',*,*,#2828,.T.);
#3682=ORIENTED_EDGE('',*,*,#2825,.T.);
#3683=ORIENTED_EDGE('',*,*,#2833,.T.);
#3684=ORIENTED_EDGE('',*,*,#2836,.T.);
#3685=ORIENTED_EDGE('',*,*,#2843,.T.);
#3686=ORIENTED_EDGE('',*,*,#2842,.T.);
#3687=ORIENTED_EDGE('',*,*,#2844,.F.);
#3688=ORIENTED_EDGE('',*,*,#2845,.F.);
#3689=ORIENTED_EDGE('',*,*,#2846,.T.);
#3690=ORIENTED_EDGE('',*,*,#2845,.T.);
#3691=ORIENTED_EDGE('',*,*,#2847,.F.);
#3692=ORIENTED_EDGE('',*,*,#2848,.F.);
#3693=ORIENTED_EDGE('',*,*,#2823,.T.);
#3694=ORIENTED_EDGE('',*,*,#2827,.T.);
#3695=ORIENTED_EDGE('',*,*,#2830,.T.);
#3696=ORIENTED_EDGE('',*,*,#2832,.T.);
#3697=ORIENTED_EDGE('',*,*,#2835,.T.);
#3698=ORIENTED_EDGE('',*,*,#2838,.T.);
#3699=ORIENTED_EDGE('',*,*,#2849,.T.);
#3700=ORIENTED_EDGE('',*,*,#2848,.T.);
#3701=ORIENTED_EDGE('',*,*,#2850,.F.);
#3702=ORIENTED_EDGE('',*,*,#2840,.F.);
#3703=ORIENTED_EDGE('',*,*,#2850,.T.);
#3704=ORIENTED_EDGE('',*,*,#2847,.T.);
#3705=ORIENTED_EDGE('',*,*,#2844,.T.);
#3706=ORIENTED_EDGE('',*,*,#2841,.T.);
#3707=ORIENTED_EDGE('',*,*,#2849,.F.);
#3708=ORIENTED_EDGE('',*,*,#2839,.F.);
#3709=ORIENTED_EDGE('',*,*,#2843,.F.);
#3710=ORIENTED_EDGE('',*,*,#2846,.F.);
#3711=ORIENTED_EDGE('',*,*,#2851,.F.);
#3712=ORIENTED_EDGE('',*,*,#2852,.T.);
#3713=ORIENTED_EDGE('',*,*,#2853,.F.);
#3714=ORIENTED_EDGE('',*,*,#2852,.F.);
#3715=ORIENTED_EDGE('',*,*,#2854,.F.);
#3716=ORIENTED_EDGE('',*,*,#2855,.T.);
#3717=ORIENTED_EDGE('',*,*,#2856,.F.);
#3718=ORIENTED_EDGE('',*,*,#2855,.F.);
#3719=ORIENTED_EDGE('',*,*,#2857,.F.);
#3720=ORIENTED_EDGE('',*,*,#2858,.F.);
#3721=ORIENTED_EDGE('',*,*,#2859,.F.);
#3722=ORIENTED_EDGE('',*,*,#2860,.F.);
#3723=ORIENTED_EDGE('',*,*,#2861,.F.);
#3724=ORIENTED_EDGE('',*,*,#2862,.F.);
#3725=ORIENTED_EDGE('',*,*,#2863,.F.);
#3726=ORIENTED_EDGE('',*,*,#2858,.T.);
#3727=ORIENTED_EDGE('',*,*,#2864,.F.);
#3728=ORIENTED_EDGE('',*,*,#2865,.F.);
#3729=ORIENTED_EDGE('',*,*,#2866,.F.);
#3730=ORIENTED_EDGE('',*,*,#2862,.T.);
#3731=ORIENTED_EDGE('',*,*,#2859,.T.);
#3732=ORIENTED_EDGE('',*,*,#2863,.T.);
#3733=ORIENTED_EDGE('',*,*,#2866,.T.);
#3734=ORIENTED_EDGE('',*,*,#2867,.F.);
#3735=ORIENTED_EDGE('',*,*,#2868,.T.);
#3736=ORIENTED_EDGE('',*,*,#2869,.T.);
#3737=ORIENTED_EDGE('',*,*,#2870,.T.);
#3738=ORIENTED_EDGE('',*,*,#2871,.T.);
#3739=ORIENTED_EDGE('',*,*,#2872,.F.);
#3740=ORIENTED_EDGE('',*,*,#2873,.T.);
#3741=ORIENTED_EDGE('',*,*,#2874,.T.);
#3742=ORIENTED_EDGE('',*,*,#2875,.F.);
#3743=ORIENTED_EDGE('',*,*,#2853,.T.);
#3744=ORIENTED_EDGE('',*,*,#2856,.T.);
#3745=ORIENTED_EDGE('',*,*,#2865,.T.);
#3746=ORIENTED_EDGE('',*,*,#2876,.F.);
#3747=ORIENTED_EDGE('',*,*,#2877,.T.);
#3748=ORIENTED_EDGE('',*,*,#2878,.T.);
#3749=ORIENTED_EDGE('',*,*,#2879,.T.);
#3750=ORIENTED_EDGE('',*,*,#2867,.T.);
#3751=ORIENTED_EDGE('',*,*,#2860,.T.);
#3752=ORIENTED_EDGE('',*,*,#2875,.T.);
#3753=ORIENTED_EDGE('',*,*,#2880,.T.);
#3754=ORIENTED_EDGE('',*,*,#2881,.T.);
#3755=ORIENTED_EDGE('',*,*,#2882,.F.);
#3756=ORIENTED_EDGE('',*,*,#2883,.F.);
#3757=ORIENTED_EDGE('',*,*,#2880,.F.);
#3758=ORIENTED_EDGE('',*,*,#2874,.F.);
#3759=ORIENTED_EDGE('',*,*,#2884,.F.);
#3760=ORIENTED_EDGE('',*,*,#2885,.F.);
#3761=ORIENTED_EDGE('',*,*,#2886,.F.);
#3762=ORIENTED_EDGE('',*,*,#2873,.F.);
#3763=ORIENTED_EDGE('',*,*,#2887,.F.);
#3764=ORIENTED_EDGE('',*,*,#2888,.F.);
#3765=ORIENTED_EDGE('',*,*,#2884,.T.);
#3766=ORIENTED_EDGE('',*,*,#2881,.F.);
#3767=ORIENTED_EDGE('',*,*,#2886,.T.);
#3768=ORIENTED_EDGE('',*,*,#2889,.F.);
#3769=ORIENTED_EDGE('',*,*,#2890,.F.);
#3770=ORIENTED_EDGE('',*,*,#2872,.T.);
#3771=ORIENTED_EDGE('',*,*,#2891,.T.);
#3772=ORIENTED_EDGE('',*,*,#2892,.T.);
#3773=ORIENTED_EDGE('',*,*,#2887,.T.);
#3774=ORIENTED_EDGE('',*,*,#2890,.T.);
#3775=ORIENTED_EDGE('',*,*,#2893,.T.);
#3776=ORIENTED_EDGE('',*,*,#2882,.T.);
#3777=ORIENTED_EDGE('',*,*,#2857,.T.);
#3778=ORIENTED_EDGE('',*,*,#2883,.T.);
#3779=ORIENTED_EDGE('',*,*,#2893,.F.);
#3780=ORIENTED_EDGE('',*,*,#2889,.T.);
#3781=ORIENTED_EDGE('',*,*,#2885,.T.);
#3782=ORIENTED_EDGE('',*,*,#2888,.T.);
#3783=ORIENTED_EDGE('',*,*,#2892,.F.);
#3784=ORIENTED_EDGE('',*,*,#2894,.F.);
#3785=ORIENTED_EDGE('',*,*,#2895,.T.);
#3786=ORIENTED_EDGE('',*,*,#2896,.T.);
#3787=ORIENTED_EDGE('',*,*,#2897,.T.);
#3788=ORIENTED_EDGE('',*,*,#2898,.T.);
#3789=ORIENTED_EDGE('',*,*,#2899,.T.);
#3790=ORIENTED_EDGE('',*,*,#2876,.T.);
#3791=ORIENTED_EDGE('',*,*,#2864,.T.);
#3792=ORIENTED_EDGE('',*,*,#2861,.T.);
#3793=ORIENTED_EDGE('',*,*,#2851,.T.);
#3794=ORIENTED_EDGE('',*,*,#2854,.T.);
#3795=ORIENTED_EDGE('',*,*,#2878,.F.);
#3796=ORIENTED_EDGE('',*,*,#2900,.T.);
#3797=ORIENTED_EDGE('',*,*,#2898,.F.);
#3798=ORIENTED_EDGE('',*,*,#2901,.F.);
#3799=ORIENTED_EDGE('',*,*,#2869,.F.);
#3800=ORIENTED_EDGE('',*,*,#2902,.F.);
#3801=ORIENTED_EDGE('',*,*,#2896,.F.);
#3802=ORIENTED_EDGE('',*,*,#2903,.T.);
#3803=ORIENTED_EDGE('',*,*,#2879,.F.);
#3804=ORIENTED_EDGE('',*,*,#2901,.T.);
#3805=ORIENTED_EDGE('',*,*,#2897,.F.);
#3806=ORIENTED_EDGE('',*,*,#2902,.T.);
#3807=ORIENTED_EDGE('',*,*,#2868,.F.);
#3808=ORIENTED_EDGE('',*,*,#2904,.T.);
#3809=ORIENTED_EDGE('',*,*,#2894,.T.);
#3810=ORIENTED_EDGE('',*,*,#2891,.F.);
#3811=ORIENTED_EDGE('',*,*,#2871,.F.);
#3812=ORIENTED_EDGE('',*,*,#2903,.F.);
#3813=ORIENTED_EDGE('',*,*,#2895,.F.);
#3814=ORIENTED_EDGE('',*,*,#2904,.F.);
#3815=ORIENTED_EDGE('',*,*,#2870,.F.);
#3816=ORIENTED_EDGE('',*,*,#2877,.F.);
#3817=ORIENTED_EDGE('',*,*,#2899,.F.);
#3818=ORIENTED_EDGE('',*,*,#2900,.F.);
#3819=ORIENTED_EDGE('',*,*,#2905,.F.);
#3820=ORIENTED_EDGE('',*,*,#2906,.T.);
#3821=ORIENTED_EDGE('',*,*,#2907,.F.);
#3822=ORIENTED_EDGE('',*,*,#2906,.F.);
#3823=ORIENTED_EDGE('',*,*,#2908,.F.);
#3824=ORIENTED_EDGE('',*,*,#2909,.T.);
#3825=ORIENTED_EDGE('',*,*,#2910,.F.);
#3826=ORIENTED_EDGE('',*,*,#2909,.F.);
#3827=ORIENTED_EDGE('',*,*,#2911,.F.);
#3828=ORIENTED_EDGE('',*,*,#2912,.T.);
#3829=ORIENTED_EDGE('',*,*,#2913,.F.);
#3830=ORIENTED_EDGE('',*,*,#2914,.F.);
#3831=ORIENTED_EDGE('',*,*,#2915,.F.);
#3832=ORIENTED_EDGE('',*,*,#2916,.F.);
#3833=ORIENTED_EDGE('',*,*,#2912,.F.);
#3834=ORIENTED_EDGE('',*,*,#2914,.T.);
#3835=ORIENTED_EDGE('',*,*,#2911,.T.);
#3836=ORIENTED_EDGE('',*,*,#2917,.F.);
#3837=ORIENTED_EDGE('',*,*,#2918,.T.);
#3838=ORIENTED_EDGE('',*,*,#2919,.T.);
#3839=ORIENTED_EDGE('',*,*,#2920,.T.);
#3840=ORIENTED_EDGE('',*,*,#2921,.F.);
#3841=ORIENTED_EDGE('',*,*,#2922,.T.);
#3842=ORIENTED_EDGE('',*,*,#2923,.T.);
#3843=ORIENTED_EDGE('',*,*,#2924,.T.);
#3844=ORIENTED_EDGE('',*,*,#2925,.T.);
#3845=ORIENTED_EDGE('',*,*,#2926,.F.);
#3846=ORIENTED_EDGE('',*,*,#2907,.T.);
#3847=ORIENTED_EDGE('',*,*,#2910,.T.);
#3848=ORIENTED_EDGE('',*,*,#2913,.T.);
#3849=ORIENTED_EDGE('',*,*,#2916,.T.);
#3850=ORIENTED_EDGE('',*,*,#2927,.F.);
#3851=ORIENTED_EDGE('',*,*,#2928,.F.);
#3852=ORIENTED_EDGE('',*,*,#2929,.T.);
#3853=ORIENTED_EDGE('',*,*,#2930,.T.);
#3854=ORIENTED_EDGE('',*,*,#2931,.T.);
#3855=ORIENTED_EDGE('',*,*,#2921,.T.);
#3856=ORIENTED_EDGE('',*,*,#2932,.T.);
#3857=ORIENTED_EDGE('',*,*,#2933,.T.);
#3858=ORIENTED_EDGE('',*,*,#2934,.T.);
#3859=ORIENTED_EDGE('',*,*,#2917,.T.);
#3860=ORIENTED_EDGE('',*,*,#2923,.F.);
#3861=ORIENTED_EDGE('',*,*,#2935,.T.);
#3862=ORIENTED_EDGE('',*,*,#2930,.F.);
#3863=ORIENTED_EDGE('',*,*,#2936,.F.);
#3864=ORIENTED_EDGE('',*,*,#2922,.F.);
#3865=ORIENTED_EDGE('',*,*,#2931,.F.);
#3866=ORIENTED_EDGE('',*,*,#2935,.F.);
#3867=ORIENTED_EDGE('',*,*,#2936,.T.);
#3868=ORIENTED_EDGE('',*,*,#2929,.F.);
#3869=ORIENTED_EDGE('',*,*,#2937,.F.);
#3870=ORIENTED_EDGE('',*,*,#2938,.F.);
#3871=ORIENTED_EDGE('',*,*,#2924,.F.);
#3872=ORIENTED_EDGE('',*,*,#2918,.F.);
#3873=ORIENTED_EDGE('',*,*,#2934,.F.);
#3874=ORIENTED_EDGE('',*,*,#2939,.T.);
#3875=ORIENTED_EDGE('',*,*,#2940,.T.);
#3876=ORIENTED_EDGE('',*,*,#2941,.T.);
#3877=ORIENTED_EDGE('',*,*,#2942,.T.);
#3878=ORIENTED_EDGE('',*,*,#2940,.F.);
#3879=ORIENTED_EDGE('',*,*,#2942,.F.);
#3880=ORIENTED_EDGE('',*,*,#2919,.F.);
#3881=ORIENTED_EDGE('',*,*,#2939,.F.);
#3882=ORIENTED_EDGE('',*,*,#2933,.F.);
#3883=ORIENTED_EDGE('',*,*,#2943,.T.);
#3884=ORIENTED_EDGE('',*,*,#2920,.F.);
#3885=ORIENTED_EDGE('',*,*,#2943,.F.);
#3886=ORIENTED_EDGE('',*,*,#2932,.F.);
#3887=ORIENTED_EDGE('',*,*,#2941,.F.);
#3888=ORIENTED_EDGE('',*,*,#2937,.T.);
#3889=ORIENTED_EDGE('',*,*,#2928,.T.);
#3890=ORIENTED_EDGE('',*,*,#2944,.F.);
#3891=ORIENTED_EDGE('',*,*,#2945,.F.);
#3892=ORIENTED_EDGE('',*,*,#2905,.T.);
#3893=ORIENTED_EDGE('',*,*,#2908,.T.);
#3894=ORIENTED_EDGE('',*,*,#2938,.T.);
#3895=ORIENTED_EDGE('',*,*,#2945,.T.);
#3896=ORIENTED_EDGE('',*,*,#2946,.F.);
#3897=ORIENTED_EDGE('',*,*,#2925,.F.);
#3898=ORIENTED_EDGE('',*,*,#2915,.T.);
#3899=ORIENTED_EDGE('',*,*,#2926,.T.);
#3900=ORIENTED_EDGE('',*,*,#2946,.T.);
#3901=ORIENTED_EDGE('',*,*,#2944,.T.);
#3902=ORIENTED_EDGE('',*,*,#2927,.T.);
#3903=ORIENTED_EDGE('',*,*,#2947,.F.);
#3904=ORIENTED_EDGE('',*,*,#2948,.F.);
#3905=ORIENTED_EDGE('',*,*,#2949,.F.);
#3906=ORIENTED_EDGE('',*,*,#2950,.T.);
#3907=ORIENTED_EDGE('',*,*,#2947,.T.);
#3908=ORIENTED_EDGE('',*,*,#2950,.F.);
#3909=ORIENTED_EDGE('',*,*,#2951,.T.);
#3910=ORIENTED_EDGE('',*,*,#2952,.F.);
#3911=ORIENTED_EDGE('',*,*,#2951,.F.);
#3912=ORIENTED_EDGE('',*,*,#2953,.T.);
#3913=ORIENTED_EDGE('',*,*,#2954,.T.);
#3914=ORIENTED_EDGE('',*,*,#2953,.F.);
#3915=ORIENTED_EDGE('',*,*,#2954,.F.);
#3916=ORIENTED_EDGE('',*,*,#2948,.T.);
#3917=ORIENTED_EDGE('',*,*,#2955,.T.);
#3918=ORIENTED_EDGE('',*,*,#2952,.T.);
#3919=ORIENTED_EDGE('',*,*,#2955,.F.);
#3920=ORIENTED_EDGE('',*,*,#2949,.T.);
#3921=ORIENTED_EDGE('',*,*,#2956,.T.);
#3922=ORIENTED_EDGE('',*,*,#2957,.T.);
#3923=ORIENTED_EDGE('',*,*,#2958,.F.);
#3924=ORIENTED_EDGE('',*,*,#2959,.F.);
#3925=ORIENTED_EDGE('',*,*,#2960,.T.);
#3926=ORIENTED_EDGE('',*,*,#2959,.T.);
#3927=ORIENTED_EDGE('',*,*,#2961,.F.);
#3928=ORIENTED_EDGE('',*,*,#2962,.F.);
#3929=ORIENTED_EDGE('',*,*,#2963,.T.);
#3930=ORIENTED_EDGE('',*,*,#2962,.T.);
#3931=ORIENTED_EDGE('',*,*,#2964,.F.);
#3932=ORIENTED_EDGE('',*,*,#2965,.F.);
#3933=ORIENTED_EDGE('',*,*,#2966,.T.);
#3934=ORIENTED_EDGE('',*,*,#2965,.T.);
#3935=ORIENTED_EDGE('',*,*,#2967,.F.);
#3936=ORIENTED_EDGE('',*,*,#2957,.F.);
#3937=ORIENTED_EDGE('',*,*,#2967,.T.);
#3938=ORIENTED_EDGE('',*,*,#2964,.T.);
#3939=ORIENTED_EDGE('',*,*,#2961,.T.);
#3940=ORIENTED_EDGE('',*,*,#2958,.T.);
#3941=ORIENTED_EDGE('',*,*,#2966,.F.);
#3942=ORIENTED_EDGE('',*,*,#2956,.F.);
#3943=ORIENTED_EDGE('',*,*,#2960,.F.);
#3944=ORIENTED_EDGE('',*,*,#2963,.F.);
#3945=ORIENTED_EDGE('',*,*,#2968,.F.);
#3946=ORIENTED_EDGE('',*,*,#2969,.T.);
#3947=ORIENTED_EDGE('',*,*,#2970,.T.);
#3948=ORIENTED_EDGE('',*,*,#2969,.F.);
#3949=ORIENTED_EDGE('',*,*,#2970,.F.);
#3950=ORIENTED_EDGE('',*,*,#2971,.F.);
#3951=ORIENTED_EDGE('',*,*,#2972,.T.);
#3952=ORIENTED_EDGE('',*,*,#2973,.T.);
#3953=ORIENTED_EDGE('',*,*,#2972,.F.);
#3954=ORIENTED_EDGE('',*,*,#2973,.F.);
#3955=ORIENTED_EDGE('',*,*,#2974,.F.);
#3956=ORIENTED_EDGE('',*,*,#2975,.T.);
#3957=ORIENTED_EDGE('',*,*,#2976,.T.);
#3958=ORIENTED_EDGE('',*,*,#2975,.F.);
#3959=ORIENTED_EDGE('',*,*,#2976,.F.);
#3960=ORIENTED_EDGE('',*,*,#2977,.F.);
#3961=ORIENTED_EDGE('',*,*,#2978,.T.);
#3962=ORIENTED_EDGE('',*,*,#2979,.T.);
#3963=ORIENTED_EDGE('',*,*,#2978,.F.);
#3964=ORIENTED_EDGE('',*,*,#2979,.F.);
#3965=ORIENTED_EDGE('',*,*,#2980,.F.);
#3966=ORIENTED_EDGE('',*,*,#2981,.T.);
#3967=ORIENTED_EDGE('',*,*,#2982,.F.);
#3968=ORIENTED_EDGE('',*,*,#2981,.F.);
#3969=ORIENTED_EDGE('',*,*,#2983,.F.);
#3970=ORIENTED_EDGE('',*,*,#2984,.T.);
#3971=ORIENTED_EDGE('',*,*,#2985,.F.);
#3972=ORIENTED_EDGE('',*,*,#2984,.F.);
#3973=ORIENTED_EDGE('',*,*,#2986,.F.);
#3974=ORIENTED_EDGE('',*,*,#2987,.F.);
#3975=ORIENTED_EDGE('',*,*,#2988,.F.);
#3976=ORIENTED_EDGE('',*,*,#2989,.F.);
#3977=ORIENTED_EDGE('',*,*,#2990,.F.);
#3978=ORIENTED_EDGE('',*,*,#2991,.F.);
#3979=ORIENTED_EDGE('',*,*,#2992,.F.);
#3980=ORIENTED_EDGE('',*,*,#2993,.F.);
#3981=ORIENTED_EDGE('',*,*,#2994,.F.);
#3982=ORIENTED_EDGE('',*,*,#2995,.F.);
#3983=ORIENTED_EDGE('',*,*,#2996,.F.);
#3984=ORIENTED_EDGE('',*,*,#2997,.F.);
#3985=ORIENTED_EDGE('',*,*,#2998,.F.);
#3986=ORIENTED_EDGE('',*,*,#2999,.F.);
#3987=ORIENTED_EDGE('',*,*,#3000,.F.);
#3988=ORIENTED_EDGE('',*,*,#3001,.F.);
#3989=ORIENTED_EDGE('',*,*,#3002,.F.);
#3990=ORIENTED_EDGE('',*,*,#3003,.F.);
#3991=ORIENTED_EDGE('',*,*,#3004,.F.);
#3992=ORIENTED_EDGE('',*,*,#3005,.T.);
#3993=ORIENTED_EDGE('',*,*,#3006,.F.);
#3994=ORIENTED_EDGE('',*,*,#3007,.F.);
#3995=ORIENTED_EDGE('',*,*,#3008,.F.);
#3996=ORIENTED_EDGE('',*,*,#3009,.T.);
#3997=ORIENTED_EDGE('',*,*,#3010,.F.);
#3998=ORIENTED_EDGE('',*,*,#3011,.F.);
#3999=ORIENTED_EDGE('',*,*,#3012,.F.);
#4000=ORIENTED_EDGE('',*,*,#3013,.T.);
#4001=ORIENTED_EDGE('',*,*,#3014,.F.);
#4002=ORIENTED_EDGE('',*,*,#3015,.F.);
#4003=ORIENTED_EDGE('',*,*,#3016,.F.);
#4004=ORIENTED_EDGE('',*,*,#3017,.T.);
#4005=ORIENTED_EDGE('',*,*,#3018,.F.);
#4006=ORIENTED_EDGE('',*,*,#3019,.F.);
#4007=ORIENTED_EDGE('',*,*,#3020,.F.);
#4008=ORIENTED_EDGE('',*,*,#3021,.F.);
#4009=ORIENTED_EDGE('',*,*,#3022,.F.);
#4010=ORIENTED_EDGE('',*,*,#3017,.F.);
#4011=ORIENTED_EDGE('',*,*,#3023,.T.);
#4012=ORIENTED_EDGE('',*,*,#3024,.F.);
#4013=ORIENTED_EDGE('',*,*,#3025,.F.);
#4014=ORIENTED_EDGE('',*,*,#3013,.F.);
#4015=ORIENTED_EDGE('',*,*,#3026,.T.);
#4016=ORIENTED_EDGE('',*,*,#3027,.F.);
#4017=ORIENTED_EDGE('',*,*,#3028,.F.);
#4018=ORIENTED_EDGE('',*,*,#3009,.F.);
#4019=ORIENTED_EDGE('',*,*,#3029,.T.);
#4020=ORIENTED_EDGE('',*,*,#3030,.F.);
#4021=ORIENTED_EDGE('',*,*,#3031,.F.);
#4022=ORIENTED_EDGE('',*,*,#3005,.F.);
#4023=ORIENTED_EDGE('',*,*,#3032,.T.);
#4024=ORIENTED_EDGE('',*,*,#3033,.F.);
#4025=ORIENTED_EDGE('',*,*,#3034,.F.);
#4026=ORIENTED_EDGE('',*,*,#3035,.F.);
#4027=ORIENTED_EDGE('',*,*,#3036,.T.);
#4028=ORIENTED_EDGE('',*,*,#2995,.T.);
#4029=ORIENTED_EDGE('',*,*,#3037,.F.);
#4030=ORIENTED_EDGE('',*,*,#3038,.F.);
#4031=ORIENTED_EDGE('',*,*,#3039,.T.);
#4032=ORIENTED_EDGE('',*,*,#2991,.T.);
#4033=ORIENTED_EDGE('',*,*,#3040,.F.);
#4034=ORIENTED_EDGE('',*,*,#3041,.F.);
#4035=ORIENTED_EDGE('',*,*,#3042,.T.);
#4036=ORIENTED_EDGE('',*,*,#2987,.T.);
#4037=ORIENTED_EDGE('',*,*,#3043,.F.);
#4038=ORIENTED_EDGE('',*,*,#3044,.F.);
#4039=ORIENTED_EDGE('',*,*,#3045,.T.);
#4040=ORIENTED_EDGE('',*,*,#2999,.T.);
#4041=ORIENTED_EDGE('',*,*,#3014,.T.);
#4042=ORIENTED_EDGE('',*,*,#3022,.T.);
#4043=ORIENTED_EDGE('',*,*,#3046,.F.);
#4044=ORIENTED_EDGE('',*,*,#3047,.F.);
#4045=ORIENTED_EDGE('',*,*,#2998,.T.);
#4046=ORIENTED_EDGE('',*,*,#3048,.F.);
#4047=ORIENTED_EDGE('',*,*,#3049,.F.);
#4048=ORIENTED_EDGE('',*,*,#3018,.T.);
#4049=ORIENTED_EDGE('',*,*,#3015,.T.);
#4050=ORIENTED_EDGE('',*,*,#3047,.T.);
#4051=ORIENTED_EDGE('',*,*,#3050,.F.);
#4052=ORIENTED_EDGE('',*,*,#3051,.T.);
#4053=ORIENTED_EDGE('',*,*,#3001,.T.);
#4054=ORIENTED_EDGE('',*,*,#3052,.T.);
#4055=ORIENTED_EDGE('',*,*,#3053,.T.);
#4056=ORIENTED_EDGE('',*,*,#3048,.T.);
#4057=ORIENTED_EDGE('',*,*,#3016,.T.);
#4058=ORIENTED_EDGE('',*,*,#3051,.F.);
#4059=ORIENTED_EDGE('',*,*,#3054,.F.);
#4060=ORIENTED_EDGE('',*,*,#3023,.F.);
#4061=ORIENTED_EDGE('',*,*,#3000,.T.);
#4062=ORIENTED_EDGE('',*,*,#3045,.F.);
#4063=ORIENTED_EDGE('',*,*,#3055,.F.);
#4064=ORIENTED_EDGE('',*,*,#3052,.F.);
#4065=ORIENTED_EDGE('',*,*,#3010,.T.);
#4066=ORIENTED_EDGE('',*,*,#3025,.T.);
#4067=ORIENTED_EDGE('',*,*,#3056,.F.);
#4068=ORIENTED_EDGE('',*,*,#3057,.F.);
#4069=ORIENTED_EDGE('',*,*,#2986,.T.);
#4070=ORIENTED_EDGE('',*,*,#3058,.F.);
#4071=ORIENTED_EDGE('',*,*,#3059,.F.);
#4072=ORIENTED_EDGE('',*,*,#3043,.T.);
#4073=ORIENTED_EDGE('',*,*,#3011,.T.);
#4074=ORIENTED_EDGE('',*,*,#3057,.T.);
#4075=ORIENTED_EDGE('',*,*,#3060,.F.);
#4076=ORIENTED_EDGE('',*,*,#3061,.T.);
#4077=ORIENTED_EDGE('',*,*,#2983,.T.);
#4078=ORIENTED_EDGE('',*,*,#2989,.T.);
#4079=ORIENTED_EDGE('',*,*,#3062,.T.);
#4080=ORIENTED_EDGE('',*,*,#3063,.T.);
#4081=ORIENTED_EDGE('',*,*,#3058,.T.);
#4082=ORIENTED_EDGE('',*,*,#3012,.T.);
#4083=ORIENTED_EDGE('',*,*,#3061,.F.);
#4084=ORIENTED_EDGE('',*,*,#3064,.F.);
#4085=ORIENTED_EDGE('',*,*,#3026,.F.);
#4086=ORIENTED_EDGE('',*,*,#2988,.T.);
#4087=ORIENTED_EDGE('',*,*,#3042,.F.);
#4088=ORIENTED_EDGE('',*,*,#3065,.F.);
#4089=ORIENTED_EDGE('',*,*,#3062,.F.);
#4090=ORIENTED_EDGE('',*,*,#3006,.T.);
#4091=ORIENTED_EDGE('',*,*,#3028,.T.);
#4092=ORIENTED_EDGE('',*,*,#3066,.F.);
#4093=ORIENTED_EDGE('',*,*,#3067,.F.);
#4094=ORIENTED_EDGE('',*,*,#2990,.T.);
#4095=ORIENTED_EDGE('',*,*,#3068,.F.);
#4096=ORIENTED_EDGE('',*,*,#3069,.F.);
#4097=ORIENTED_EDGE('',*,*,#3040,.T.);
#4098=ORIENTED_EDGE('',*,*,#3007,.T.);
#4099=ORIENTED_EDGE('',*,*,#3067,.T.);
#4100=ORIENTED_EDGE('',*,*,#3070,.F.);
#4101=ORIENTED_EDGE('',*,*,#3071,.T.);
#4102=ORIENTED_EDGE('',*,*,#2980,.T.);
#4103=ORIENTED_EDGE('',*,*,#2993,.T.);
#4104=ORIENTED_EDGE('',*,*,#3072,.T.);
#4105=ORIENTED_EDGE('',*,*,#3073,.T.);
#4106=ORIENTED_EDGE('',*,*,#3068,.T.);
#4107=ORIENTED_EDGE('',*,*,#3008,.T.);
#4108=ORIENTED_EDGE('',*,*,#3071,.F.);
#4109=ORIENTED_EDGE('',*,*,#3074,.F.);
#4110=ORIENTED_EDGE('',*,*,#3029,.F.);
#4111=ORIENTED_EDGE('',*,*,#2992,.T.);
#4112=ORIENTED_EDGE('',*,*,#3039,.F.);
#4113=ORIENTED_EDGE('',*,*,#3075,.F.);
#4114=ORIENTED_EDGE('',*,*,#3072,.F.);
#4115=ORIENTED_EDGE('',*,*,#3002,.T.);
#4116=ORIENTED_EDGE('',*,*,#3031,.T.);
#4117=ORIENTED_EDGE('',*,*,#3076,.F.);
#4118=ORIENTED_EDGE('',*,*,#3077,.F.);
#4119=ORIENTED_EDGE('',*,*,#2994,.T.);
#4120=ORIENTED_EDGE('',*,*,#3078,.F.);
#4121=ORIENTED_EDGE('',*,*,#3079,.F.);
#4122=ORIENTED_EDGE('',*,*,#3037,.T.);
#4123=ORIENTED_EDGE('',*,*,#3003,.T.);
#4124=ORIENTED_EDGE('',*,*,#3077,.T.);
#4125=ORIENTED_EDGE('',*,*,#3080,.F.);
#4126=ORIENTED_EDGE('',*,*,#3081,.T.);
#4127=ORIENTED_EDGE('',*,*,#2997,.T.);
#4128=ORIENTED_EDGE('',*,*,#3082,.T.);
#4129=ORIENTED_EDGE('',*,*,#3083,.T.);
#4130=ORIENTED_EDGE('',*,*,#3078,.T.);
#4131=ORIENTED_EDGE('',*,*,#3004,.T.);
#4132=ORIENTED_EDGE('',*,*,#3081,.F.);
#4133=ORIENTED_EDGE('',*,*,#3084,.F.);
#4134=ORIENTED_EDGE('',*,*,#3032,.F.);
#4135=ORIENTED_EDGE('',*,*,#2996,.T.);
#4136=ORIENTED_EDGE('',*,*,#3036,.F.);
#4137=ORIENTED_EDGE('',*,*,#3085,.F.);
#4138=ORIENTED_EDGE('',*,*,#3082,.F.);
#4139=ORIENTED_EDGE('',*,*,#3055,.T.);
#4140=ORIENTED_EDGE('',*,*,#3044,.T.);
#4141=ORIENTED_EDGE('',*,*,#3059,.T.);
#4142=ORIENTED_EDGE('',*,*,#3063,.F.);
#4143=ORIENTED_EDGE('',*,*,#3065,.T.);
#4144=ORIENTED_EDGE('',*,*,#3041,.T.);
#4145=ORIENTED_EDGE('',*,*,#3069,.T.);
#4146=ORIENTED_EDGE('',*,*,#3073,.F.);
#4147=ORIENTED_EDGE('',*,*,#3075,.T.);
#4148=ORIENTED_EDGE('',*,*,#3038,.T.);
#4149=ORIENTED_EDGE('',*,*,#3079,.T.);
#4150=ORIENTED_EDGE('',*,*,#3083,.F.);
#4151=ORIENTED_EDGE('',*,*,#3085,.T.);
#4152=ORIENTED_EDGE('',*,*,#3035,.T.);
#4153=ORIENTED_EDGE('',*,*,#3086,.T.);
#4154=ORIENTED_EDGE('',*,*,#3087,.T.);
#4155=ORIENTED_EDGE('',*,*,#3088,.F.);
#4156=ORIENTED_EDGE('',*,*,#3019,.T.);
#4157=ORIENTED_EDGE('',*,*,#3049,.T.);
#4158=ORIENTED_EDGE('',*,*,#3053,.F.);
#4159=ORIENTED_EDGE('',*,*,#3034,.T.);
#4160=ORIENTED_EDGE('',*,*,#3089,.F.);
#4161=ORIENTED_EDGE('',*,*,#3090,.F.);
#4162=ORIENTED_EDGE('',*,*,#3086,.F.);
#4163=ORIENTED_EDGE('',*,*,#3054,.T.);
#4164=ORIENTED_EDGE('',*,*,#3050,.T.);
#4165=ORIENTED_EDGE('',*,*,#3046,.T.);
#4166=ORIENTED_EDGE('',*,*,#3021,.T.);
#4167=ORIENTED_EDGE('',*,*,#3091,.F.);
#4168=ORIENTED_EDGE('',*,*,#3092,.F.);
#4169=ORIENTED_EDGE('',*,*,#3089,.T.);
#4170=ORIENTED_EDGE('',*,*,#3033,.T.);
#4171=ORIENTED_EDGE('',*,*,#3084,.T.);
#4172=ORIENTED_EDGE('',*,*,#3080,.T.);
#4173=ORIENTED_EDGE('',*,*,#3076,.T.);
#4174=ORIENTED_EDGE('',*,*,#3030,.T.);
#4175=ORIENTED_EDGE('',*,*,#3074,.T.);
#4176=ORIENTED_EDGE('',*,*,#3070,.T.);
#4177=ORIENTED_EDGE('',*,*,#3066,.T.);
#4178=ORIENTED_EDGE('',*,*,#3027,.T.);
#4179=ORIENTED_EDGE('',*,*,#3064,.T.);
#4180=ORIENTED_EDGE('',*,*,#3060,.T.);
#4181=ORIENTED_EDGE('',*,*,#3056,.T.);
#4182=ORIENTED_EDGE('',*,*,#3024,.T.);
#4183=ORIENTED_EDGE('',*,*,#3090,.T.);
#4184=ORIENTED_EDGE('',*,*,#3092,.T.);
#4185=ORIENTED_EDGE('',*,*,#3093,.F.);
#4186=ORIENTED_EDGE('',*,*,#3087,.F.);
#4187=ORIENTED_EDGE('',*,*,#2985,.T.);
#4188=ORIENTED_EDGE('',*,*,#2982,.T.);
#4189=ORIENTED_EDGE('',*,*,#2977,.T.);
#4190=ORIENTED_EDGE('',*,*,#2974,.T.);
#4191=ORIENTED_EDGE('',*,*,#2971,.T.);
#4192=ORIENTED_EDGE('',*,*,#2968,.T.);
#4193=ORIENTED_EDGE('',*,*,#3020,.T.);
#4194=ORIENTED_EDGE('',*,*,#3088,.T.);
#4195=ORIENTED_EDGE('',*,*,#3093,.T.);
#4196=ORIENTED_EDGE('',*,*,#3091,.T.);
#4197=ORIENTED_EDGE('',*,*,#3094,.F.);
#4198=ORIENTED_EDGE('',*,*,#3095,.F.);
#4199=ORIENTED_EDGE('',*,*,#3096,.F.);
#4200=ORIENTED_EDGE('',*,*,#3097,.F.);
#4201=ORIENTED_EDGE('',*,*,#3098,.F.);
#4202=ORIENTED_EDGE('',*,*,#3099,.F.);
#4203=ORIENTED_EDGE('',*,*,#3100,.F.);
#4204=ORIENTED_EDGE('',*,*,#3101,.F.);
#4205=ORIENTED_EDGE('',*,*,#3102,.F.);
#4206=ORIENTED_EDGE('',*,*,#3096,.T.);
#4207=ORIENTED_EDGE('',*,*,#3103,.F.);
#4208=ORIENTED_EDGE('',*,*,#3100,.T.);
#4209=ORIENTED_EDGE('',*,*,#3101,.T.);
#4210=ORIENTED_EDGE('',*,*,#3103,.T.);
#4211=ORIENTED_EDGE('',*,*,#3095,.T.);
#4212=ORIENTED_EDGE('',*,*,#3104,.F.);
#4213=ORIENTED_EDGE('',*,*,#3105,.F.);
#4214=ORIENTED_EDGE('',*,*,#3106,.T.);
#4215=ORIENTED_EDGE('',*,*,#3107,.T.);
#4216=ORIENTED_EDGE('',*,*,#3108,.F.);
#4217=ORIENTED_EDGE('',*,*,#3094,.T.);
#4218=ORIENTED_EDGE('',*,*,#3109,.T.);
#4219=ORIENTED_EDGE('',*,*,#3110,.T.);
#4220=ORIENTED_EDGE('',*,*,#3104,.T.);
#4221=ORIENTED_EDGE('',*,*,#3111,.T.);
#4222=ORIENTED_EDGE('',*,*,#3112,.T.);
#4223=ORIENTED_EDGE('',*,*,#3113,.F.);
#4224=ORIENTED_EDGE('',*,*,#3107,.F.);
#4225=ORIENTED_EDGE('',*,*,#3114,.T.);
#4226=ORIENTED_EDGE('',*,*,#3105,.T.);
#4227=ORIENTED_EDGE('',*,*,#3110,.F.);
#4228=ORIENTED_EDGE('',*,*,#3115,.F.);
#4229=ORIENTED_EDGE('',*,*,#3099,.T.);
#4230=ORIENTED_EDGE('',*,*,#3116,.F.);
#4231=ORIENTED_EDGE('',*,*,#3112,.F.);
#4232=ORIENTED_EDGE('',*,*,#3117,.T.);
#4233=ORIENTED_EDGE('',*,*,#3115,.T.);
#4234=ORIENTED_EDGE('',*,*,#3109,.F.);
#4235=ORIENTED_EDGE('',*,*,#3097,.T.);
#4236=ORIENTED_EDGE('',*,*,#3102,.T.);
#4237=ORIENTED_EDGE('',*,*,#3098,.T.);
#4238=ORIENTED_EDGE('',*,*,#3108,.T.);
#4239=ORIENTED_EDGE('',*,*,#3113,.T.);
#4240=ORIENTED_EDGE('',*,*,#3116,.T.);
#4241=ORIENTED_EDGE('',*,*,#3117,.F.);
#4242=ORIENTED_EDGE('',*,*,#3111,.F.);
#4243=ORIENTED_EDGE('',*,*,#3106,.F.);
#4244=ORIENTED_EDGE('',*,*,#3114,.F.);
#4245=ORIENTED_EDGE('',*,*,#3118,.F.);
#4246=ORIENTED_EDGE('',*,*,#3119,.T.);
#4247=ORIENTED_EDGE('',*,*,#3120,.F.);
#4248=ORIENTED_EDGE('',*,*,#3121,.F.);
#4249=ORIENTED_EDGE('',*,*,#3122,.F.);
#4250=ORIENTED_EDGE('',*,*,#3123,.F.);
#4251=ORIENTED_EDGE('',*,*,#3124,.F.);
#4252=ORIENTED_EDGE('',*,*,#3119,.F.);
#4253=ORIENTED_EDGE('',*,*,#3121,.T.);
#4254=ORIENTED_EDGE('',*,*,#3125,.F.);
#4255=ORIENTED_EDGE('',*,*,#3126,.F.);
#4256=ORIENTED_EDGE('',*,*,#3127,.T.);
#4257=ORIENTED_EDGE('',*,*,#3123,.T.);
#4258=ORIENTED_EDGE('',*,*,#3128,.T.);
#4259=ORIENTED_EDGE('',*,*,#3129,.T.);
#4260=ORIENTED_EDGE('',*,*,#3130,.F.);
#4261=ORIENTED_EDGE('',*,*,#3131,.T.);
#4262=ORIENTED_EDGE('',*,*,#3126,.T.);
#4263=ORIENTED_EDGE('',*,*,#3132,.F.);
#4264=ORIENTED_EDGE('',*,*,#3133,.F.);
#4265=ORIENTED_EDGE('',*,*,#3134,.T.);
#4266=ORIENTED_EDGE('',*,*,#3133,.T.);
#4267=ORIENTED_EDGE('',*,*,#3135,.F.);
#4268=ORIENTED_EDGE('',*,*,#3129,.F.);
#4269=ORIENTED_EDGE('',*,*,#3124,.T.);
#4270=ORIENTED_EDGE('',*,*,#3130,.T.);
#4271=ORIENTED_EDGE('',*,*,#3135,.T.);
#4272=ORIENTED_EDGE('',*,*,#3132,.T.);
#4273=ORIENTED_EDGE('',*,*,#3125,.T.);
#4274=ORIENTED_EDGE('',*,*,#3120,.T.);
#4275=ORIENTED_EDGE('',*,*,#3118,.T.);
#4276=ORIENTED_EDGE('',*,*,#3127,.F.);
#4277=ORIENTED_EDGE('',*,*,#3131,.F.);
#4278=ORIENTED_EDGE('',*,*,#3134,.F.);
#4279=ORIENTED_EDGE('',*,*,#3128,.F.);
#4280=ORIENTED_EDGE('',*,*,#3122,.T.);
#4281=ORIENTED_EDGE('',*,*,#3136,.F.);
#4282=ORIENTED_EDGE('',*,*,#3137,.F.);
#4283=ORIENTED_EDGE('',*,*,#3138,.F.);
#4284=ORIENTED_EDGE('',*,*,#3139,.T.);
#4285=ORIENTED_EDGE('',*,*,#3140,.F.);
#4286=ORIENTED_EDGE('',*,*,#3141,.F.);
#4287=ORIENTED_EDGE('',*,*,#3136,.T.);
#4288=ORIENTED_EDGE('',*,*,#3142,.T.);
#4289=ORIENTED_EDGE('',*,*,#3143,.T.);
#4290=ORIENTED_EDGE('',*,*,#3144,.F.);
#4291=ORIENTED_EDGE('',*,*,#3145,.F.);
#4292=ORIENTED_EDGE('',*,*,#3146,.F.);
#4293=ORIENTED_EDGE('',*,*,#3140,.T.);
#4294=ORIENTED_EDGE('',*,*,#3147,.T.);
#4295=ORIENTED_EDGE('',*,*,#3148,.F.);
#4296=ORIENTED_EDGE('',*,*,#3149,.F.);
#4297=ORIENTED_EDGE('',*,*,#3144,.T.);
#4298=ORIENTED_EDGE('',*,*,#3150,.T.);
#4299=ORIENTED_EDGE('',*,*,#3151,.T.);
#4300=ORIENTED_EDGE('',*,*,#3152,.F.);
#4301=ORIENTED_EDGE('',*,*,#3153,.F.);
#4302=ORIENTED_EDGE('',*,*,#3154,.F.);
#4303=ORIENTED_EDGE('',*,*,#3148,.T.);
#4304=ORIENTED_EDGE('',*,*,#3155,.T.);
#4305=ORIENTED_EDGE('',*,*,#3156,.F.);
#4306=ORIENTED_EDGE('',*,*,#3157,.F.);
#4307=ORIENTED_EDGE('',*,*,#3152,.T.);
#4308=ORIENTED_EDGE('',*,*,#3158,.T.);
#4309=ORIENTED_EDGE('',*,*,#3159,.T.);
#4310=ORIENTED_EDGE('',*,*,#3160,.F.);
#4311=ORIENTED_EDGE('',*,*,#3161,.F.);
#4312=ORIENTED_EDGE('',*,*,#3162,.F.);
#4313=ORIENTED_EDGE('',*,*,#3156,.T.);
#4314=ORIENTED_EDGE('',*,*,#3163,.T.);
#4315=ORIENTED_EDGE('',*,*,#3164,.T.);
#4316=ORIENTED_EDGE('',*,*,#3165,.F.);
#4317=ORIENTED_EDGE('',*,*,#3166,.F.);
#4318=ORIENTED_EDGE('',*,*,#3167,.F.);
#4319=ORIENTED_EDGE('',*,*,#3160,.T.);
#4320=ORIENTED_EDGE('',*,*,#3168,.T.);
#4321=ORIENTED_EDGE('',*,*,#3169,.T.);
#4322=ORIENTED_EDGE('',*,*,#3170,.F.);
#4323=ORIENTED_EDGE('',*,*,#3171,.F.);
#4324=ORIENTED_EDGE('',*,*,#3172,.F.);
#4325=ORIENTED_EDGE('',*,*,#3165,.T.);
#4326=ORIENTED_EDGE('',*,*,#3173,.T.);
#4327=ORIENTED_EDGE('',*,*,#3174,.F.);
#4328=ORIENTED_EDGE('',*,*,#3175,.F.);
#4329=ORIENTED_EDGE('',*,*,#3170,.T.);
#4330=ORIENTED_EDGE('',*,*,#3176,.T.);
#4331=ORIENTED_EDGE('',*,*,#3177,.T.);
#4332=ORIENTED_EDGE('',*,*,#3178,.F.);
#4333=ORIENTED_EDGE('',*,*,#3179,.F.);
#4334=ORIENTED_EDGE('',*,*,#3180,.F.);
#4335=ORIENTED_EDGE('',*,*,#3174,.T.);
#4336=ORIENTED_EDGE('',*,*,#3181,.T.);
#4337=ORIENTED_EDGE('',*,*,#3182,.F.);
#4338=ORIENTED_EDGE('',*,*,#3183,.F.);
#4339=ORIENTED_EDGE('',*,*,#3178,.T.);
#4340=ORIENTED_EDGE('',*,*,#3184,.T.);
#4341=ORIENTED_EDGE('',*,*,#3185,.T.);
#4342=ORIENTED_EDGE('',*,*,#3186,.F.);
#4343=ORIENTED_EDGE('',*,*,#3187,.F.);
#4344=ORIENTED_EDGE('',*,*,#3188,.F.);
#4345=ORIENTED_EDGE('',*,*,#3182,.T.);
#4346=ORIENTED_EDGE('',*,*,#3189,.T.);
#4347=ORIENTED_EDGE('',*,*,#3190,.F.);
#4348=ORIENTED_EDGE('',*,*,#3191,.F.);
#4349=ORIENTED_EDGE('',*,*,#3186,.T.);
#4350=ORIENTED_EDGE('',*,*,#3192,.T.);
#4351=ORIENTED_EDGE('',*,*,#3193,.T.);
#4352=ORIENTED_EDGE('',*,*,#3194,.F.);
#4353=ORIENTED_EDGE('',*,*,#3195,.F.);
#4354=ORIENTED_EDGE('',*,*,#3196,.F.);
#4355=ORIENTED_EDGE('',*,*,#3190,.T.);
#4356=ORIENTED_EDGE('',*,*,#3197,.T.);
#4357=ORIENTED_EDGE('',*,*,#3198,.F.);
#4358=ORIENTED_EDGE('',*,*,#3199,.F.);
#4359=ORIENTED_EDGE('',*,*,#3194,.T.);
#4360=ORIENTED_EDGE('',*,*,#3200,.T.);
#4361=ORIENTED_EDGE('',*,*,#3201,.T.);
#4362=ORIENTED_EDGE('',*,*,#3202,.F.);
#4363=ORIENTED_EDGE('',*,*,#3203,.F.);
#4364=ORIENTED_EDGE('',*,*,#3204,.F.);
#4365=ORIENTED_EDGE('',*,*,#3198,.T.);
#4366=ORIENTED_EDGE('',*,*,#3205,.T.);
#4367=ORIENTED_EDGE('',*,*,#3206,.F.);
#4368=ORIENTED_EDGE('',*,*,#3207,.F.);
#4369=ORIENTED_EDGE('',*,*,#3202,.T.);
#4370=ORIENTED_EDGE('',*,*,#3208,.T.);
#4371=ORIENTED_EDGE('',*,*,#3209,.T.);
#4372=ORIENTED_EDGE('',*,*,#3210,.F.);
#4373=ORIENTED_EDGE('',*,*,#3211,.F.);
#4374=ORIENTED_EDGE('',*,*,#3212,.F.);
#4375=ORIENTED_EDGE('',*,*,#3206,.T.);
#4376=ORIENTED_EDGE('',*,*,#3213,.T.);
#4377=ORIENTED_EDGE('',*,*,#3214,.T.);
#4378=ORIENTED_EDGE('',*,*,#3215,.F.);
#4379=ORIENTED_EDGE('',*,*,#3216,.F.);
#4380=ORIENTED_EDGE('',*,*,#3217,.F.);
#4381=ORIENTED_EDGE('',*,*,#3210,.T.);
#4382=ORIENTED_EDGE('',*,*,#3218,.T.);
#4383=ORIENTED_EDGE('',*,*,#3219,.T.);
#4384=ORIENTED_EDGE('',*,*,#3220,.F.);
#4385=ORIENTED_EDGE('',*,*,#3221,.F.);
#4386=ORIENTED_EDGE('',*,*,#3222,.F.);
#4387=ORIENTED_EDGE('',*,*,#3215,.T.);
#4388=ORIENTED_EDGE('',*,*,#3223,.T.);
#4389=ORIENTED_EDGE('',*,*,#3224,.F.);
#4390=ORIENTED_EDGE('',*,*,#3225,.F.);
#4391=ORIENTED_EDGE('',*,*,#3220,.T.);
#4392=ORIENTED_EDGE('',*,*,#3226,.T.);
#4393=ORIENTED_EDGE('',*,*,#3227,.T.);
#4394=ORIENTED_EDGE('',*,*,#3228,.F.);
#4395=ORIENTED_EDGE('',*,*,#3229,.F.);
#4396=ORIENTED_EDGE('',*,*,#3230,.F.);
#4397=ORIENTED_EDGE('',*,*,#3224,.T.);
#4398=ORIENTED_EDGE('',*,*,#3231,.T.);
#4399=ORIENTED_EDGE('',*,*,#3232,.F.);
#4400=ORIENTED_EDGE('',*,*,#3233,.F.);
#4401=ORIENTED_EDGE('',*,*,#3228,.T.);
#4402=ORIENTED_EDGE('',*,*,#3234,.T.);
#4403=ORIENTED_EDGE('',*,*,#3235,.T.);
#4404=ORIENTED_EDGE('',*,*,#3236,.F.);
#4405=ORIENTED_EDGE('',*,*,#3237,.F.);
#4406=ORIENTED_EDGE('',*,*,#3238,.F.);
#4407=ORIENTED_EDGE('',*,*,#3232,.T.);
#4408=ORIENTED_EDGE('',*,*,#3239,.T.);
#4409=ORIENTED_EDGE('',*,*,#3240,.F.);
#4410=ORIENTED_EDGE('',*,*,#3241,.F.);
#4411=ORIENTED_EDGE('',*,*,#3236,.T.);
#4412=ORIENTED_EDGE('',*,*,#3242,.T.);
#4413=ORIENTED_EDGE('',*,*,#3243,.T.);
#4414=ORIENTED_EDGE('',*,*,#3244,.F.);
#4415=ORIENTED_EDGE('',*,*,#3245,.F.);
#4416=ORIENTED_EDGE('',*,*,#3246,.F.);
#4417=ORIENTED_EDGE('',*,*,#3240,.T.);
#4418=ORIENTED_EDGE('',*,*,#3247,.T.);
#4419=ORIENTED_EDGE('',*,*,#3248,.F.);
#4420=ORIENTED_EDGE('',*,*,#3249,.F.);
#4421=ORIENTED_EDGE('',*,*,#3244,.T.);
#4422=ORIENTED_EDGE('',*,*,#3250,.T.);
#4423=ORIENTED_EDGE('',*,*,#3251,.T.);
#4424=ORIENTED_EDGE('',*,*,#3252,.F.);
#4425=ORIENTED_EDGE('',*,*,#3253,.F.);
#4426=ORIENTED_EDGE('',*,*,#3254,.F.);
#4427=ORIENTED_EDGE('',*,*,#3248,.T.);
#4428=ORIENTED_EDGE('',*,*,#3255,.T.);
#4429=ORIENTED_EDGE('',*,*,#3256,.T.);
#4430=ORIENTED_EDGE('',*,*,#3257,.F.);
#4431=ORIENTED_EDGE('',*,*,#3258,.F.);
#4432=ORIENTED_EDGE('',*,*,#3252,.T.);
#4433=ORIENTED_EDGE('',*,*,#3259,.T.);
#4434=ORIENTED_EDGE('',*,*,#3260,.F.);
#4435=ORIENTED_EDGE('',*,*,#3261,.F.);
#4436=ORIENTED_EDGE('',*,*,#3262,.F.);
#4437=ORIENTED_EDGE('',*,*,#3257,.T.);
#4438=ORIENTED_EDGE('',*,*,#3263,.T.);
#4439=ORIENTED_EDGE('',*,*,#3264,.T.);
#4440=ORIENTED_EDGE('',*,*,#3265,.F.);
#4441=ORIENTED_EDGE('',*,*,#3266,.F.);
#4442=ORIENTED_EDGE('',*,*,#3267,.F.);
#4443=ORIENTED_EDGE('',*,*,#3260,.T.);
#4444=ORIENTED_EDGE('',*,*,#3268,.T.);
#4445=ORIENTED_EDGE('',*,*,#3269,.F.);
#4446=ORIENTED_EDGE('',*,*,#3270,.F.);
#4447=ORIENTED_EDGE('',*,*,#3271,.F.);
#4448=ORIENTED_EDGE('',*,*,#3265,.T.);
#4449=ORIENTED_EDGE('',*,*,#3272,.T.);
#4450=ORIENTED_EDGE('',*,*,#3273,.T.);
#4451=ORIENTED_EDGE('',*,*,#3274,.F.);
#4452=ORIENTED_EDGE('',*,*,#3275,.F.);
#4453=ORIENTED_EDGE('',*,*,#3269,.T.);
#4454=ORIENTED_EDGE('',*,*,#3276,.T.);
#4455=ORIENTED_EDGE('',*,*,#3277,.T.);
#4456=ORIENTED_EDGE('',*,*,#3278,.T.);
#4457=ORIENTED_EDGE('',*,*,#3279,.T.);
#4458=ORIENTED_EDGE('',*,*,#3280,.T.);
#4459=ORIENTED_EDGE('',*,*,#3281,.T.);
#4460=ORIENTED_EDGE('',*,*,#3282,.T.);
#4461=ORIENTED_EDGE('',*,*,#3283,.T.);
#4462=ORIENTED_EDGE('',*,*,#3284,.T.);
#4463=ORIENTED_EDGE('',*,*,#3285,.T.);
#4464=ORIENTED_EDGE('',*,*,#3286,.T.);
#4465=ORIENTED_EDGE('',*,*,#3287,.T.);
#4466=ORIENTED_EDGE('',*,*,#3288,.T.);
#4467=ORIENTED_EDGE('',*,*,#3289,.T.);
#4468=ORIENTED_EDGE('',*,*,#3290,.T.);
#4469=ORIENTED_EDGE('',*,*,#3291,.T.);
#4470=ORIENTED_EDGE('',*,*,#3292,.T.);
#4471=ORIENTED_EDGE('',*,*,#3293,.T.);
#4472=ORIENTED_EDGE('',*,*,#3294,.T.);
#4473=ORIENTED_EDGE('',*,*,#3295,.T.);
#4474=ORIENTED_EDGE('',*,*,#3296,.T.);
#4475=ORIENTED_EDGE('',*,*,#3297,.T.);
#4476=ORIENTED_EDGE('',*,*,#3298,.T.);
#4477=ORIENTED_EDGE('',*,*,#3299,.T.);
#4478=ORIENTED_EDGE('',*,*,#3300,.T.);
#4479=ORIENTED_EDGE('',*,*,#3301,.T.);
#4480=ORIENTED_EDGE('',*,*,#3302,.T.);
#4481=ORIENTED_EDGE('',*,*,#3303,.T.);
#4482=ORIENTED_EDGE('',*,*,#3304,.T.);
#4483=ORIENTED_EDGE('',*,*,#3305,.T.);
#4484=ORIENTED_EDGE('',*,*,#3306,.T.);
#4485=ORIENTED_EDGE('',*,*,#3307,.T.);
#4486=ORIENTED_EDGE('',*,*,#3308,.T.);
#4487=ORIENTED_EDGE('',*,*,#3309,.T.);
#4488=ORIENTED_EDGE('',*,*,#3310,.T.);
#4489=ORIENTED_EDGE('',*,*,#3311,.T.);
#4490=ORIENTED_EDGE('',*,*,#3312,.T.);
#4491=ORIENTED_EDGE('',*,*,#3313,.T.);
#4492=ORIENTED_EDGE('',*,*,#3314,.T.);
#4493=ORIENTED_EDGE('',*,*,#3315,.T.);
#4494=ORIENTED_EDGE('',*,*,#3316,.F.);
#4495=ORIENTED_EDGE('',*,*,#3317,.T.);
#4496=ORIENTED_EDGE('',*,*,#3318,.T.);
#4497=ORIENTED_EDGE('',*,*,#3319,.T.);
#4498=ORIENTED_EDGE('',*,*,#3320,.T.);
#4499=ORIENTED_EDGE('',*,*,#3321,.T.);
#4500=ORIENTED_EDGE('',*,*,#3322,.T.);
#4501=ORIENTED_EDGE('',*,*,#3323,.T.);
#4502=ORIENTED_EDGE('',*,*,#3324,.T.);
#4503=ORIENTED_EDGE('',*,*,#3325,.T.);
#4504=ORIENTED_EDGE('',*,*,#3326,.T.);
#4505=ORIENTED_EDGE('',*,*,#3327,.T.);
#4506=ORIENTED_EDGE('',*,*,#3328,.T.);
#4507=ORIENTED_EDGE('',*,*,#3329,.T.);
#4508=ORIENTED_EDGE('',*,*,#3330,.T.);
#4509=ORIENTED_EDGE('',*,*,#3331,.T.);
#4510=ORIENTED_EDGE('',*,*,#3332,.T.);
#4511=ORIENTED_EDGE('',*,*,#3333,.T.);
#4512=ORIENTED_EDGE('',*,*,#3334,.T.);
#4513=ORIENTED_EDGE('',*,*,#3335,.T.);
#4514=ORIENTED_EDGE('',*,*,#3336,.T.);
#4515=ORIENTED_EDGE('',*,*,#3337,.T.);
#4516=ORIENTED_EDGE('',*,*,#3338,.T.);
#4517=ORIENTED_EDGE('',*,*,#3339,.T.);
#4518=ORIENTED_EDGE('',*,*,#3340,.T.);
#4519=ORIENTED_EDGE('',*,*,#3341,.T.);
#4520=ORIENTED_EDGE('',*,*,#3342,.T.);
#4521=ORIENTED_EDGE('',*,*,#3343,.T.);
#4522=ORIENTED_EDGE('',*,*,#3344,.T.);
#4523=ORIENTED_EDGE('',*,*,#3345,.T.);
#4524=ORIENTED_EDGE('',*,*,#3346,.T.);
#4525=ORIENTED_EDGE('',*,*,#3347,.T.);
#4526=ORIENTED_EDGE('',*,*,#3348,.T.);
#4527=ORIENTED_EDGE('',*,*,#3349,.T.);
#4528=ORIENTED_EDGE('',*,*,#3350,.T.);
#4529=ORIENTED_EDGE('',*,*,#3274,.T.);
#4530=ORIENTED_EDGE('',*,*,#3351,.T.);
#4531=ORIENTED_EDGE('',*,*,#3352,.F.);
#4532=ORIENTED_EDGE('',*,*,#3353,.F.);
#4533=ORIENTED_EDGE('',*,*,#3354,.F.);
#4534=ORIENTED_EDGE('',*,*,#3355,.F.);
#4535=ORIENTED_EDGE('',*,*,#3315,.F.);
#4536=ORIENTED_EDGE('',*,*,#3314,.F.);
#4537=ORIENTED_EDGE('',*,*,#3313,.F.);
#4538=ORIENTED_EDGE('',*,*,#3312,.F.);
#4539=ORIENTED_EDGE('',*,*,#3311,.F.);
#4540=ORIENTED_EDGE('',*,*,#3310,.F.);
#4541=ORIENTED_EDGE('',*,*,#3309,.F.);
#4542=ORIENTED_EDGE('',*,*,#3308,.F.);
#4543=ORIENTED_EDGE('',*,*,#3307,.F.);
#4544=ORIENTED_EDGE('',*,*,#3306,.F.);
#4545=ORIENTED_EDGE('',*,*,#3305,.F.);
#4546=ORIENTED_EDGE('',*,*,#3304,.F.);
#4547=ORIENTED_EDGE('',*,*,#3303,.F.);
#4548=ORIENTED_EDGE('',*,*,#3302,.F.);
#4549=ORIENTED_EDGE('',*,*,#3301,.F.);
#4550=ORIENTED_EDGE('',*,*,#3300,.F.);
#4551=ORIENTED_EDGE('',*,*,#3299,.F.);
#4552=ORIENTED_EDGE('',*,*,#3298,.F.);
#4553=ORIENTED_EDGE('',*,*,#3297,.F.);
#4554=ORIENTED_EDGE('',*,*,#3296,.F.);
#4555=ORIENTED_EDGE('',*,*,#3295,.F.);
#4556=ORIENTED_EDGE('',*,*,#3294,.F.);
#4557=ORIENTED_EDGE('',*,*,#3293,.F.);
#4558=ORIENTED_EDGE('',*,*,#3292,.F.);
#4559=ORIENTED_EDGE('',*,*,#3291,.F.);
#4560=ORIENTED_EDGE('',*,*,#3290,.F.);
#4561=ORIENTED_EDGE('',*,*,#3289,.F.);
#4562=ORIENTED_EDGE('',*,*,#3288,.F.);
#4563=ORIENTED_EDGE('',*,*,#3287,.F.);
#4564=ORIENTED_EDGE('',*,*,#3286,.F.);
#4565=ORIENTED_EDGE('',*,*,#3285,.F.);
#4566=ORIENTED_EDGE('',*,*,#3284,.F.);
#4567=ORIENTED_EDGE('',*,*,#3283,.F.);
#4568=ORIENTED_EDGE('',*,*,#3282,.F.);
#4569=ORIENTED_EDGE('',*,*,#3281,.F.);
#4570=ORIENTED_EDGE('',*,*,#3280,.F.);
#4571=ORIENTED_EDGE('',*,*,#3356,.F.);
#4572=ORIENTED_EDGE('',*,*,#3357,.T.);
#4573=ORIENTED_EDGE('',*,*,#3137,.T.);
#4574=ORIENTED_EDGE('',*,*,#3141,.T.);
#4575=ORIENTED_EDGE('',*,*,#3146,.T.);
#4576=ORIENTED_EDGE('',*,*,#3145,.T.);
#4577=ORIENTED_EDGE('',*,*,#3149,.T.);
#4578=ORIENTED_EDGE('',*,*,#3154,.T.);
#4579=ORIENTED_EDGE('',*,*,#3153,.T.);
#4580=ORIENTED_EDGE('',*,*,#3157,.T.);
#4581=ORIENTED_EDGE('',*,*,#3162,.T.);
#4582=ORIENTED_EDGE('',*,*,#3161,.T.);
#4583=ORIENTED_EDGE('',*,*,#3167,.T.);
#4584=ORIENTED_EDGE('',*,*,#3166,.T.);
#4585=ORIENTED_EDGE('',*,*,#3172,.T.);
#4586=ORIENTED_EDGE('',*,*,#3171,.T.);
#4587=ORIENTED_EDGE('',*,*,#3175,.T.);
#4588=ORIENTED_EDGE('',*,*,#3180,.T.);
#4589=ORIENTED_EDGE('',*,*,#3179,.T.);
#4590=ORIENTED_EDGE('',*,*,#3183,.T.);
#4591=ORIENTED_EDGE('',*,*,#3188,.T.);
#4592=ORIENTED_EDGE('',*,*,#3187,.T.);
#4593=ORIENTED_EDGE('',*,*,#3191,.T.);
#4594=ORIENTED_EDGE('',*,*,#3196,.T.);
#4595=ORIENTED_EDGE('',*,*,#3195,.T.);
#4596=ORIENTED_EDGE('',*,*,#3199,.T.);
#4597=ORIENTED_EDGE('',*,*,#3204,.T.);
#4598=ORIENTED_EDGE('',*,*,#3203,.T.);
#4599=ORIENTED_EDGE('',*,*,#3207,.T.);
#4600=ORIENTED_EDGE('',*,*,#3212,.T.);
#4601=ORIENTED_EDGE('',*,*,#3211,.T.);
#4602=ORIENTED_EDGE('',*,*,#3217,.T.);
#4603=ORIENTED_EDGE('',*,*,#3216,.T.);
#4604=ORIENTED_EDGE('',*,*,#3222,.T.);
#4605=ORIENTED_EDGE('',*,*,#3221,.T.);
#4606=ORIENTED_EDGE('',*,*,#3225,.T.);
#4607=ORIENTED_EDGE('',*,*,#3230,.T.);
#4608=ORIENTED_EDGE('',*,*,#3229,.T.);
#4609=ORIENTED_EDGE('',*,*,#3233,.T.);
#4610=ORIENTED_EDGE('',*,*,#3238,.T.);
#4611=ORIENTED_EDGE('',*,*,#3237,.T.);
#4612=ORIENTED_EDGE('',*,*,#3241,.T.);
#4613=ORIENTED_EDGE('',*,*,#3246,.T.);
#4614=ORIENTED_EDGE('',*,*,#3245,.T.);
#4615=ORIENTED_EDGE('',*,*,#3249,.T.);
#4616=ORIENTED_EDGE('',*,*,#3254,.T.);
#4617=ORIENTED_EDGE('',*,*,#3253,.T.);
#4618=ORIENTED_EDGE('',*,*,#3258,.T.);
#4619=ORIENTED_EDGE('',*,*,#3262,.T.);
#4620=ORIENTED_EDGE('',*,*,#3261,.T.);
#4621=ORIENTED_EDGE('',*,*,#3267,.T.);
#4622=ORIENTED_EDGE('',*,*,#3266,.T.);
#4623=ORIENTED_EDGE('',*,*,#3271,.T.);
#4624=ORIENTED_EDGE('',*,*,#3270,.T.);
#4625=ORIENTED_EDGE('',*,*,#3275,.T.);
#4626=ORIENTED_EDGE('',*,*,#3354,.T.);
#4627=ORIENTED_EDGE('',*,*,#3353,.T.);
#4628=ORIENTED_EDGE('',*,*,#3358,.F.);
#4629=ORIENTED_EDGE('',*,*,#3359,.F.);
#4630=ORIENTED_EDGE('',*,*,#3351,.F.);
#4631=ORIENTED_EDGE('',*,*,#3277,.F.);
#4632=ORIENTED_EDGE('',*,*,#3276,.F.);
#4633=ORIENTED_EDGE('',*,*,#3273,.F.);
#4634=ORIENTED_EDGE('',*,*,#3272,.F.);
#4635=ORIENTED_EDGE('',*,*,#3268,.F.);
#4636=ORIENTED_EDGE('',*,*,#3264,.F.);
#4637=ORIENTED_EDGE('',*,*,#3263,.F.);
#4638=ORIENTED_EDGE('',*,*,#3259,.F.);
#4639=ORIENTED_EDGE('',*,*,#3256,.F.);
#4640=ORIENTED_EDGE('',*,*,#3255,.F.);
#4641=ORIENTED_EDGE('',*,*,#3251,.F.);
#4642=ORIENTED_EDGE('',*,*,#3250,.F.);
#4643=ORIENTED_EDGE('',*,*,#3247,.F.);
#4644=ORIENTED_EDGE('',*,*,#3243,.F.);
#4645=ORIENTED_EDGE('',*,*,#3242,.F.);
#4646=ORIENTED_EDGE('',*,*,#3239,.F.);
#4647=ORIENTED_EDGE('',*,*,#3235,.F.);
#4648=ORIENTED_EDGE('',*,*,#3234,.F.);
#4649=ORIENTED_EDGE('',*,*,#3231,.F.);
#4650=ORIENTED_EDGE('',*,*,#3227,.F.);
#4651=ORIENTED_EDGE('',*,*,#3226,.F.);
#4652=ORIENTED_EDGE('',*,*,#3223,.F.);
#4653=ORIENTED_EDGE('',*,*,#3219,.F.);
#4654=ORIENTED_EDGE('',*,*,#3218,.F.);
#4655=ORIENTED_EDGE('',*,*,#3214,.F.);
#4656=ORIENTED_EDGE('',*,*,#3213,.F.);
#4657=ORIENTED_EDGE('',*,*,#3209,.F.);
#4658=ORIENTED_EDGE('',*,*,#3208,.F.);
#4659=ORIENTED_EDGE('',*,*,#3205,.F.);
#4660=ORIENTED_EDGE('',*,*,#3201,.F.);
#4661=ORIENTED_EDGE('',*,*,#3200,.F.);
#4662=ORIENTED_EDGE('',*,*,#3197,.F.);
#4663=ORIENTED_EDGE('',*,*,#3193,.F.);
#4664=ORIENTED_EDGE('',*,*,#3192,.F.);
#4665=ORIENTED_EDGE('',*,*,#3189,.F.);
#4666=ORIENTED_EDGE('',*,*,#3185,.F.);
#4667=ORIENTED_EDGE('',*,*,#3184,.F.);
#4668=ORIENTED_EDGE('',*,*,#3181,.F.);
#4669=ORIENTED_EDGE('',*,*,#3177,.F.);
#4670=ORIENTED_EDGE('',*,*,#3176,.F.);
#4671=ORIENTED_EDGE('',*,*,#3173,.F.);
#4672=ORIENTED_EDGE('',*,*,#3169,.F.);
#4673=ORIENTED_EDGE('',*,*,#3168,.F.);
#4674=ORIENTED_EDGE('',*,*,#3164,.F.);
#4675=ORIENTED_EDGE('',*,*,#3163,.F.);
#4676=ORIENTED_EDGE('',*,*,#3159,.F.);
#4677=ORIENTED_EDGE('',*,*,#3158,.F.);
#4678=ORIENTED_EDGE('',*,*,#3155,.F.);
#4679=ORIENTED_EDGE('',*,*,#3151,.F.);
#4680=ORIENTED_EDGE('',*,*,#3150,.F.);
#4681=ORIENTED_EDGE('',*,*,#3147,.F.);
#4682=ORIENTED_EDGE('',*,*,#3143,.F.);
#4683=ORIENTED_EDGE('',*,*,#3142,.F.);
#4684=ORIENTED_EDGE('',*,*,#3139,.F.);
#4685=ORIENTED_EDGE('',*,*,#3360,.F.);
#4686=ORIENTED_EDGE('',*,*,#3278,.F.);
#4687=ORIENTED_EDGE('',*,*,#3350,.F.);
#4688=ORIENTED_EDGE('',*,*,#3349,.F.);
#4689=ORIENTED_EDGE('',*,*,#3348,.F.);
#4690=ORIENTED_EDGE('',*,*,#3347,.F.);
#4691=ORIENTED_EDGE('',*,*,#3346,.F.);
#4692=ORIENTED_EDGE('',*,*,#3345,.F.);
#4693=ORIENTED_EDGE('',*,*,#3344,.F.);
#4694=ORIENTED_EDGE('',*,*,#3343,.F.);
#4695=ORIENTED_EDGE('',*,*,#3342,.F.);
#4696=ORIENTED_EDGE('',*,*,#3341,.F.);
#4697=ORIENTED_EDGE('',*,*,#3340,.F.);
#4698=ORIENTED_EDGE('',*,*,#3339,.F.);
#4699=ORIENTED_EDGE('',*,*,#3338,.F.);
#4700=ORIENTED_EDGE('',*,*,#3337,.F.);
#4701=ORIENTED_EDGE('',*,*,#3336,.F.);
#4702=ORIENTED_EDGE('',*,*,#3335,.F.);
#4703=ORIENTED_EDGE('',*,*,#3334,.F.);
#4704=ORIENTED_EDGE('',*,*,#3333,.F.);
#4705=ORIENTED_EDGE('',*,*,#3332,.F.);
#4706=ORIENTED_EDGE('',*,*,#3331,.F.);
#4707=ORIENTED_EDGE('',*,*,#3330,.F.);
#4708=ORIENTED_EDGE('',*,*,#3329,.F.);
#4709=ORIENTED_EDGE('',*,*,#3328,.F.);
#4710=ORIENTED_EDGE('',*,*,#3327,.F.);
#4711=ORIENTED_EDGE('',*,*,#3326,.F.);
#4712=ORIENTED_EDGE('',*,*,#3325,.F.);
#4713=ORIENTED_EDGE('',*,*,#3324,.F.);
#4714=ORIENTED_EDGE('',*,*,#3323,.F.);
#4715=ORIENTED_EDGE('',*,*,#3322,.F.);
#4716=ORIENTED_EDGE('',*,*,#3321,.F.);
#4717=ORIENTED_EDGE('',*,*,#3320,.F.);
#4718=ORIENTED_EDGE('',*,*,#3319,.F.);
#4719=ORIENTED_EDGE('',*,*,#3318,.F.);
#4720=ORIENTED_EDGE('',*,*,#3317,.F.);
#4721=ORIENTED_EDGE('',*,*,#3361,.F.);
#4722=ORIENTED_EDGE('',*,*,#3362,.T.);
#4723=ORIENTED_EDGE('',*,*,#3363,.T.);
#4724=ORIENTED_EDGE('',*,*,#3364,.F.);
#4725=ORIENTED_EDGE('',*,*,#3365,.F.);
#4726=ORIENTED_EDGE('',*,*,#3366,.T.);
#4727=ORIENTED_EDGE('',*,*,#3367,.T.);
#4728=ORIENTED_EDGE('',*,*,#3362,.F.);
#4729=ORIENTED_EDGE('',*,*,#3368,.F.);
#4730=ORIENTED_EDGE('',*,*,#3369,.T.);
#4731=ORIENTED_EDGE('',*,*,#3370,.T.);
#4732=ORIENTED_EDGE('',*,*,#3366,.F.);
#4733=ORIENTED_EDGE('',*,*,#3371,.F.);
#4734=ORIENTED_EDGE('',*,*,#3372,.T.);
#4735=ORIENTED_EDGE('',*,*,#3373,.T.);
#4736=ORIENTED_EDGE('',*,*,#3369,.F.);
#4737=ORIENTED_EDGE('',*,*,#3374,.F.);
#4738=ORIENTED_EDGE('',*,*,#3375,.T.);
#4739=ORIENTED_EDGE('',*,*,#3376,.T.);
#4740=ORIENTED_EDGE('',*,*,#3372,.F.);
#4741=ORIENTED_EDGE('',*,*,#3377,.F.);
#4742=ORIENTED_EDGE('',*,*,#3364,.T.);
#4743=ORIENTED_EDGE('',*,*,#3378,.T.);
#4744=ORIENTED_EDGE('',*,*,#3375,.F.);
#4745=ORIENTED_EDGE('',*,*,#3378,.F.);
#4746=ORIENTED_EDGE('',*,*,#3363,.F.);
#4747=ORIENTED_EDGE('',*,*,#3367,.F.);
#4748=ORIENTED_EDGE('',*,*,#3370,.F.);
#4749=ORIENTED_EDGE('',*,*,#3373,.F.);
#4750=ORIENTED_EDGE('',*,*,#3376,.F.);
#4751=ORIENTED_EDGE('',*,*,#3379,.T.);
#4752=ORIENTED_EDGE('',*,*,#3360,.T.);
#4753=ORIENTED_EDGE('',*,*,#3138,.T.);
#4754=ORIENTED_EDGE('',*,*,#3357,.F.);
#4755=ORIENTED_EDGE('',*,*,#3356,.T.);
#4756=ORIENTED_EDGE('',*,*,#3279,.F.);
#4757=ORIENTED_EDGE('',*,*,#3379,.F.);
#4758=ORIENTED_EDGE('',*,*,#3380,.T.);
#4759=ORIENTED_EDGE('',*,*,#3381,.T.);
#4760=ORIENTED_EDGE('',*,*,#3380,.F.);
#4761=ORIENTED_EDGE('',*,*,#3381,.F.);
#4762=ORIENTED_EDGE('',*,*,#3361,.T.);
#4763=ORIENTED_EDGE('',*,*,#3377,.T.);
#4764=ORIENTED_EDGE('',*,*,#3374,.T.);
#4765=ORIENTED_EDGE('',*,*,#3371,.T.);
#4766=ORIENTED_EDGE('',*,*,#3368,.T.);
#4767=ORIENTED_EDGE('',*,*,#3365,.T.);
#4768=ORIENTED_EDGE('',*,*,#3358,.T.);
#4769=ORIENTED_EDGE('',*,*,#3316,.T.);
#4770=ORIENTED_EDGE('',*,*,#3355,.T.);
#4771=ORIENTED_EDGE('',*,*,#3352,.T.);
#4772=ORIENTED_EDGE('',*,*,#3359,.T.);
#4773=ORIENTED_EDGE('',*,*,#3382,.T.);
#4774=ORIENTED_EDGE('',*,*,#3383,.T.);
#4775=ORIENTED_EDGE('',*,*,#3384,.F.);
#4776=ORIENTED_EDGE('',*,*,#3385,.F.);
#4777=ORIENTED_EDGE('',*,*,#3386,.T.);
#4778=ORIENTED_EDGE('',*,*,#3387,.T.);
#4779=ORIENTED_EDGE('',*,*,#3388,.T.);
#4780=ORIENTED_EDGE('',*,*,#3382,.F.);
#4781=ORIENTED_EDGE('',*,*,#3389,.F.);
#4782=ORIENTED_EDGE('',*,*,#3390,.F.);
#4783=ORIENTED_EDGE('',*,*,#3391,.T.);
#4784=ORIENTED_EDGE('',*,*,#3392,.T.);
#4785=ORIENTED_EDGE('',*,*,#3393,.T.);
#4786=ORIENTED_EDGE('',*,*,#3386,.F.);
#4787=ORIENTED_EDGE('',*,*,#3394,.F.);
#4788=ORIENTED_EDGE('',*,*,#3395,.F.);
#4789=ORIENTED_EDGE('',*,*,#3396,.T.);
#4790=ORIENTED_EDGE('',*,*,#3397,.T.);
#4791=ORIENTED_EDGE('',*,*,#3398,.T.);
#4792=ORIENTED_EDGE('',*,*,#3391,.F.);
#4793=ORIENTED_EDGE('',*,*,#3399,.F.);
#4794=ORIENTED_EDGE('',*,*,#3400,.F.);
#4795=ORIENTED_EDGE('',*,*,#3401,.T.);
#4796=ORIENTED_EDGE('',*,*,#3402,.T.);
#4797=ORIENTED_EDGE('',*,*,#3403,.T.);
#4798=ORIENTED_EDGE('',*,*,#3396,.F.);
#4799=ORIENTED_EDGE('',*,*,#3404,.F.);
#4800=ORIENTED_EDGE('',*,*,#3405,.F.);
#4801=ORIENTED_EDGE('',*,*,#3406,.F.);
#4802=ORIENTED_EDGE('',*,*,#3407,.F.);
#4803=ORIENTED_EDGE('',*,*,#3408,.F.);
#4804=ORIENTED_EDGE('',*,*,#3409,.F.);
#4805=ORIENTED_EDGE('',*,*,#3410,.T.);
#4806=ORIENTED_EDGE('',*,*,#3411,.T.);
#4807=ORIENTED_EDGE('',*,*,#3412,.T.);
#4808=ORIENTED_EDGE('',*,*,#3413,.F.);
#4809=ORIENTED_EDGE('',*,*,#3414,.T.);
#4810=ORIENTED_EDGE('',*,*,#3415,.T.);
#4811=ORIENTED_EDGE('',*,*,#3416,.T.);
#4812=ORIENTED_EDGE('',*,*,#3417,.F.);
#4813=ORIENTED_EDGE('',*,*,#3412,.F.);
#4814=ORIENTED_EDGE('',*,*,#3418,.T.);
#4815=ORIENTED_EDGE('',*,*,#3419,.T.);
#4816=ORIENTED_EDGE('',*,*,#3420,.T.);
#4817=ORIENTED_EDGE('',*,*,#3421,.T.);
#4818=ORIENTED_EDGE('',*,*,#3422,.T.);
#4819=ORIENTED_EDGE('',*,*,#3415,.F.);
#4820=ORIENTED_EDGE('',*,*,#3423,.T.);
#4821=ORIENTED_EDGE('',*,*,#3424,.T.);
#4822=ORIENTED_EDGE('',*,*,#3425,.T.);
#4823=ORIENTED_EDGE('',*,*,#3420,.F.);
#4824=ORIENTED_EDGE('',*,*,#3426,.T.);
#4825=ORIENTED_EDGE('',*,*,#3427,.T.);
#4826=ORIENTED_EDGE('',*,*,#3428,.T.);
#4827=ORIENTED_EDGE('',*,*,#3429,.T.);
#4828=ORIENTED_EDGE('',*,*,#3430,.T.);
#4829=ORIENTED_EDGE('',*,*,#3424,.F.);
#4830=ORIENTED_EDGE('',*,*,#3431,.T.);
#4831=ORIENTED_EDGE('',*,*,#3432,.F.);
#4832=ORIENTED_EDGE('',*,*,#3433,.T.);
#4833=ORIENTED_EDGE('',*,*,#3434,.T.);
#4834=ORIENTED_EDGE('',*,*,#3435,.F.);
#4835=ORIENTED_EDGE('',*,*,#3436,.T.);
#4836=ORIENTED_EDGE('',*,*,#3437,.T.);
#4837=ORIENTED_EDGE('',*,*,#3432,.T.);
#4838=ORIENTED_EDGE('',*,*,#3438,.T.);
#4839=ORIENTED_EDGE('',*,*,#3439,.T.);
#4840=ORIENTED_EDGE('',*,*,#3428,.F.);
#4841=ORIENTED_EDGE('',*,*,#3440,.T.);
#4842=ORIENTED_EDGE('',*,*,#3441,.T.);
#4843=ORIENTED_EDGE('',*,*,#3406,.T.);
#4844=ORIENTED_EDGE('',*,*,#3442,.T.);
#4845=ORIENTED_EDGE('',*,*,#3443,.T.);
#4846=ORIENTED_EDGE('',*,*,#3401,.F.);
#4847=ORIENTED_EDGE('',*,*,#3444,.F.);
#4848=ORIENTED_EDGE('',*,*,#3445,.F.);
#4849=ORIENTED_EDGE('',*,*,#3446,.F.);
#4850=ORIENTED_EDGE('',*,*,#3383,.F.);
#4851=ORIENTED_EDGE('',*,*,#3388,.F.);
#4852=ORIENTED_EDGE('',*,*,#3387,.F.);
#4853=ORIENTED_EDGE('',*,*,#3393,.F.);
#4854=ORIENTED_EDGE('',*,*,#3392,.F.);
#4855=ORIENTED_EDGE('',*,*,#3398,.F.);
#4856=ORIENTED_EDGE('',*,*,#3397,.F.);
#4857=ORIENTED_EDGE('',*,*,#3403,.F.);
#4858=ORIENTED_EDGE('',*,*,#3402,.F.);
#4859=ORIENTED_EDGE('',*,*,#3443,.F.);
#4860=ORIENTED_EDGE('',*,*,#3442,.F.);
#4861=ORIENTED_EDGE('',*,*,#3411,.F.);
#4862=ORIENTED_EDGE('',*,*,#3410,.F.);
#4863=ORIENTED_EDGE('',*,*,#3447,.F.);
#4864=ORIENTED_EDGE('',*,*,#3434,.F.);
#4865=ORIENTED_EDGE('',*,*,#3433,.F.);
#4866=ORIENTED_EDGE('',*,*,#3441,.F.);
#4867=ORIENTED_EDGE('',*,*,#3440,.F.);
#4868=ORIENTED_EDGE('',*,*,#3431,.F.);
#4869=ORIENTED_EDGE('',*,*,#3427,.F.);
#4870=ORIENTED_EDGE('',*,*,#3426,.F.);
#4871=ORIENTED_EDGE('',*,*,#3423,.F.);
#4872=ORIENTED_EDGE('',*,*,#3419,.F.);
#4873=ORIENTED_EDGE('',*,*,#3418,.F.);
#4874=ORIENTED_EDGE('',*,*,#3414,.F.);
#4875=ORIENTED_EDGE('',*,*,#3448,.F.);
#4876=ORIENTED_EDGE('',*,*,#3416,.F.);
#4877=ORIENTED_EDGE('',*,*,#3422,.F.);
#4878=ORIENTED_EDGE('',*,*,#3421,.F.);
#4879=ORIENTED_EDGE('',*,*,#3425,.F.);
#4880=ORIENTED_EDGE('',*,*,#3430,.F.);
#4881=ORIENTED_EDGE('',*,*,#3429,.F.);
#4882=ORIENTED_EDGE('',*,*,#3439,.F.);
#4883=ORIENTED_EDGE('',*,*,#3438,.F.);
#4884=ORIENTED_EDGE('',*,*,#3437,.F.);
#4885=ORIENTED_EDGE('',*,*,#3436,.F.);
#4886=ORIENTED_EDGE('',*,*,#3449,.F.);
#4887=ORIENTED_EDGE('',*,*,#3408,.T.);
#4888=ORIENTED_EDGE('',*,*,#3407,.T.);
#4889=ORIENTED_EDGE('',*,*,#3445,.T.);
#4890=ORIENTED_EDGE('',*,*,#3444,.T.);
#4891=ORIENTED_EDGE('',*,*,#3405,.T.);
#4892=ORIENTED_EDGE('',*,*,#3404,.T.);
#4893=ORIENTED_EDGE('',*,*,#3400,.T.);
#4894=ORIENTED_EDGE('',*,*,#3399,.T.);
#4895=ORIENTED_EDGE('',*,*,#3395,.T.);
#4896=ORIENTED_EDGE('',*,*,#3394,.T.);
#4897=ORIENTED_EDGE('',*,*,#3390,.T.);
#4898=ORIENTED_EDGE('',*,*,#3389,.T.);
#4899=ORIENTED_EDGE('',*,*,#3385,.T.);
#4900=ORIENTED_EDGE('',*,*,#3450,.T.);
#4901=ORIENTED_EDGE('',*,*,#3451,.T.);
#4902=ORIENTED_EDGE('',*,*,#3452,.T.);
#4903=ORIENTED_EDGE('',*,*,#3453,.T.);
#4904=ORIENTED_EDGE('',*,*,#3454,.T.);
#4905=ORIENTED_EDGE('',*,*,#3455,.T.);
#4906=ORIENTED_EDGE('',*,*,#3447,.T.);
#4907=ORIENTED_EDGE('',*,*,#3409,.T.);
#4908=ORIENTED_EDGE('',*,*,#3449,.T.);
#4909=ORIENTED_EDGE('',*,*,#3435,.T.);
#4910=ORIENTED_EDGE('',*,*,#3456,.T.);
#4911=ORIENTED_EDGE('',*,*,#3457,.T.);
#4912=ORIENTED_EDGE('',*,*,#3455,.F.);
#4913=ORIENTED_EDGE('',*,*,#3458,.F.);
#4914=ORIENTED_EDGE('',*,*,#3459,.T.);
#4915=ORIENTED_EDGE('',*,*,#3458,.T.);
#4916=ORIENTED_EDGE('',*,*,#3454,.F.);
#4917=ORIENTED_EDGE('',*,*,#3460,.F.);
#4918=ORIENTED_EDGE('',*,*,#3461,.T.);
#4919=ORIENTED_EDGE('',*,*,#3460,.T.);
#4920=ORIENTED_EDGE('',*,*,#3453,.F.);
#4921=ORIENTED_EDGE('',*,*,#3462,.F.);
#4922=ORIENTED_EDGE('',*,*,#3463,.T.);
#4923=ORIENTED_EDGE('',*,*,#3462,.T.);
#4924=ORIENTED_EDGE('',*,*,#3452,.F.);
#4925=ORIENTED_EDGE('',*,*,#3464,.F.);
#4926=ORIENTED_EDGE('',*,*,#3465,.T.);
#4927=ORIENTED_EDGE('',*,*,#3464,.T.);
#4928=ORIENTED_EDGE('',*,*,#3451,.F.);
#4929=ORIENTED_EDGE('',*,*,#3466,.F.);
#4930=ORIENTED_EDGE('',*,*,#3467,.T.);
#4931=ORIENTED_EDGE('',*,*,#3466,.T.);
#4932=ORIENTED_EDGE('',*,*,#3450,.F.);
#4933=ORIENTED_EDGE('',*,*,#3457,.F.);
#4934=ORIENTED_EDGE('',*,*,#3467,.F.);
#4935=ORIENTED_EDGE('',*,*,#3456,.F.);
#4936=ORIENTED_EDGE('',*,*,#3459,.F.);
#4937=ORIENTED_EDGE('',*,*,#3461,.F.);
#4938=ORIENTED_EDGE('',*,*,#3463,.F.);
#4939=ORIENTED_EDGE('',*,*,#3465,.F.);
#4940=ORIENTED_EDGE('',*,*,#3446,.T.);
#4941=ORIENTED_EDGE('',*,*,#3413,.T.);
#4942=ORIENTED_EDGE('',*,*,#3417,.T.);
#4943=ORIENTED_EDGE('',*,*,#3448,.T.);
#4944=ORIENTED_EDGE('',*,*,#3384,.T.);
#4945=ORIENTED_EDGE('',*,*,#3468,.F.);
#4946=ORIENTED_EDGE('',*,*,#3469,.T.);
#4947=ORIENTED_EDGE('',*,*,#3470,.T.);
#4948=ORIENTED_EDGE('',*,*,#3469,.F.);
#4949=ORIENTED_EDGE('',*,*,#3470,.F.);
#4950=ORIENTED_EDGE('',*,*,#3471,.F.);
#4951=ORIENTED_EDGE('',*,*,#3472,.T.);
#4952=ORIENTED_EDGE('',*,*,#3473,.T.);
#4953=ORIENTED_EDGE('',*,*,#3472,.F.);
#4954=ORIENTED_EDGE('',*,*,#3473,.F.);
#4955=ORIENTED_EDGE('',*,*,#3474,.F.);
#4956=ORIENTED_EDGE('',*,*,#3475,.T.);
#4957=ORIENTED_EDGE('',*,*,#3476,.T.);
#4958=ORIENTED_EDGE('',*,*,#3475,.F.);
#4959=ORIENTED_EDGE('',*,*,#3476,.F.);
#4960=ORIENTED_EDGE('',*,*,#3477,.F.);
#4961=ORIENTED_EDGE('',*,*,#3478,.T.);
#4962=ORIENTED_EDGE('',*,*,#3479,.T.);
#4963=ORIENTED_EDGE('',*,*,#3478,.F.);
#4964=ORIENTED_EDGE('',*,*,#3479,.F.);
#4965=ORIENTED_EDGE('',*,*,#3480,.F.);
#4966=ORIENTED_EDGE('',*,*,#3481,.F.);
#4967=ORIENTED_EDGE('',*,*,#3482,.F.);
#4968=ORIENTED_EDGE('',*,*,#3483,.F.);
#4969=ORIENTED_EDGE('',*,*,#3484,.F.);
#4970=ORIENTED_EDGE('',*,*,#3485,.F.);
#4971=ORIENTED_EDGE('',*,*,#3486,.F.);
#4972=ORIENTED_EDGE('',*,*,#3487,.F.);
#4973=ORIENTED_EDGE('',*,*,#3488,.F.);
#4974=ORIENTED_EDGE('',*,*,#3489,.F.);
#4975=ORIENTED_EDGE('',*,*,#3490,.F.);
#4976=ORIENTED_EDGE('',*,*,#3491,.F.);
#4977=ORIENTED_EDGE('',*,*,#3492,.F.);
#4978=ORIENTED_EDGE('',*,*,#3493,.F.);
#4979=ORIENTED_EDGE('',*,*,#3494,.F.);
#4980=ORIENTED_EDGE('',*,*,#3495,.F.);
#4981=ORIENTED_EDGE('',*,*,#3496,.F.);
#4982=ORIENTED_EDGE('',*,*,#3497,.F.);
#4983=ORIENTED_EDGE('',*,*,#3498,.F.);
#4984=ORIENTED_EDGE('',*,*,#3499,.T.);
#4985=ORIENTED_EDGE('',*,*,#3500,.F.);
#4986=ORIENTED_EDGE('',*,*,#3501,.F.);
#4987=ORIENTED_EDGE('',*,*,#3502,.F.);
#4988=ORIENTED_EDGE('',*,*,#3503,.T.);
#4989=ORIENTED_EDGE('',*,*,#3504,.F.);
#4990=ORIENTED_EDGE('',*,*,#3505,.F.);
#4991=ORIENTED_EDGE('',*,*,#3506,.F.);
#4992=ORIENTED_EDGE('',*,*,#3507,.T.);
#4993=ORIENTED_EDGE('',*,*,#3508,.F.);
#4994=ORIENTED_EDGE('',*,*,#3509,.F.);
#4995=ORIENTED_EDGE('',*,*,#3510,.F.);
#4996=ORIENTED_EDGE('',*,*,#3511,.T.);
#4997=ORIENTED_EDGE('',*,*,#3512,.F.);
#4998=ORIENTED_EDGE('',*,*,#3513,.F.);
#4999=ORIENTED_EDGE('',*,*,#3514,.F.);
#5000=ORIENTED_EDGE('',*,*,#3515,.F.);
#5001=ORIENTED_EDGE('',*,*,#3516,.F.);
#5002=ORIENTED_EDGE('',*,*,#3511,.F.);
#5003=ORIENTED_EDGE('',*,*,#3517,.T.);
#5004=ORIENTED_EDGE('',*,*,#3518,.F.);
#5005=ORIENTED_EDGE('',*,*,#3519,.F.);
#5006=ORIENTED_EDGE('',*,*,#3507,.F.);
#5007=ORIENTED_EDGE('',*,*,#3520,.T.);
#5008=ORIENTED_EDGE('',*,*,#3521,.F.);
#5009=ORIENTED_EDGE('',*,*,#3522,.F.);
#5010=ORIENTED_EDGE('',*,*,#3503,.F.);
#5011=ORIENTED_EDGE('',*,*,#3523,.T.);
#5012=ORIENTED_EDGE('',*,*,#3524,.F.);
#5013=ORIENTED_EDGE('',*,*,#3525,.F.);
#5014=ORIENTED_EDGE('',*,*,#3499,.F.);
#5015=ORIENTED_EDGE('',*,*,#3526,.T.);
#5016=ORIENTED_EDGE('',*,*,#3527,.F.);
#5017=ORIENTED_EDGE('',*,*,#3528,.F.);
#5018=ORIENTED_EDGE('',*,*,#3529,.F.);
#5019=ORIENTED_EDGE('',*,*,#3530,.T.);
#5020=ORIENTED_EDGE('',*,*,#3489,.T.);
#5021=ORIENTED_EDGE('',*,*,#3531,.F.);
#5022=ORIENTED_EDGE('',*,*,#3532,.F.);
#5023=ORIENTED_EDGE('',*,*,#3533,.T.);
#5024=ORIENTED_EDGE('',*,*,#3485,.T.);
#5025=ORIENTED_EDGE('',*,*,#3534,.F.);
#5026=ORIENTED_EDGE('',*,*,#3535,.F.);
#5027=ORIENTED_EDGE('',*,*,#3536,.T.);
#5028=ORIENTED_EDGE('',*,*,#3481,.T.);
#5029=ORIENTED_EDGE('',*,*,#3537,.F.);
#5030=ORIENTED_EDGE('',*,*,#3538,.F.);
#5031=ORIENTED_EDGE('',*,*,#3539,.T.);
#5032=ORIENTED_EDGE('',*,*,#3493,.T.);
#5033=ORIENTED_EDGE('',*,*,#3508,.T.);
#5034=ORIENTED_EDGE('',*,*,#3516,.T.);
#5035=ORIENTED_EDGE('',*,*,#3540,.F.);
#5036=ORIENTED_EDGE('',*,*,#3541,.F.);
#5037=ORIENTED_EDGE('',*,*,#3492,.T.);
#5038=ORIENTED_EDGE('',*,*,#3542,.F.);
#5039=ORIENTED_EDGE('',*,*,#3543,.F.);
#5040=ORIENTED_EDGE('',*,*,#3512,.T.);
#5041=ORIENTED_EDGE('',*,*,#3509,.T.);
#5042=ORIENTED_EDGE('',*,*,#3541,.T.);
#5043=ORIENTED_EDGE('',*,*,#3544,.F.);
#5044=ORIENTED_EDGE('',*,*,#3545,.T.);
#5045=ORIENTED_EDGE('',*,*,#3495,.T.);
#5046=ORIENTED_EDGE('',*,*,#3546,.T.);
#5047=ORIENTED_EDGE('',*,*,#3547,.T.);
#5048=ORIENTED_EDGE('',*,*,#3542,.T.);
#5049=ORIENTED_EDGE('',*,*,#3510,.T.);
#5050=ORIENTED_EDGE('',*,*,#3545,.F.);
#5051=ORIENTED_EDGE('',*,*,#3548,.F.);
#5052=ORIENTED_EDGE('',*,*,#3517,.F.);
#5053=ORIENTED_EDGE('',*,*,#3494,.T.);
#5054=ORIENTED_EDGE('',*,*,#3539,.F.);
#5055=ORIENTED_EDGE('',*,*,#3549,.F.);
#5056=ORIENTED_EDGE('',*,*,#3546,.F.);
#5057=ORIENTED_EDGE('',*,*,#3504,.T.);
#5058=ORIENTED_EDGE('',*,*,#3519,.T.);
#5059=ORIENTED_EDGE('',*,*,#3550,.F.);
#5060=ORIENTED_EDGE('',*,*,#3551,.F.);
#5061=ORIENTED_EDGE('',*,*,#3480,.T.);
#5062=ORIENTED_EDGE('',*,*,#3552,.F.);
#5063=ORIENTED_EDGE('',*,*,#3553,.F.);
#5064=ORIENTED_EDGE('',*,*,#3537,.T.);
#5065=ORIENTED_EDGE('',*,*,#3505,.T.);
#5066=ORIENTED_EDGE('',*,*,#3551,.T.);
#5067=ORIENTED_EDGE('',*,*,#3554,.F.);
#5068=ORIENTED_EDGE('',*,*,#3555,.T.);
#5069=ORIENTED_EDGE('',*,*,#3483,.T.);
#5070=ORIENTED_EDGE('',*,*,#3556,.T.);
#5071=ORIENTED_EDGE('',*,*,#3557,.T.);
#5072=ORIENTED_EDGE('',*,*,#3552,.T.);
#5073=ORIENTED_EDGE('',*,*,#3506,.T.);
#5074=ORIENTED_EDGE('',*,*,#3555,.F.);
#5075=ORIENTED_EDGE('',*,*,#3558,.F.);
#5076=ORIENTED_EDGE('',*,*,#3520,.F.);
#5077=ORIENTED_EDGE('',*,*,#3482,.T.);
#5078=ORIENTED_EDGE('',*,*,#3536,.F.);
#5079=ORIENTED_EDGE('',*,*,#3559,.F.);
#5080=ORIENTED_EDGE('',*,*,#3556,.F.);
#5081=ORIENTED_EDGE('',*,*,#3500,.T.);
#5082=ORIENTED_EDGE('',*,*,#3522,.T.);
#5083=ORIENTED_EDGE('',*,*,#3560,.F.);
#5084=ORIENTED_EDGE('',*,*,#3561,.F.);
#5085=ORIENTED_EDGE('',*,*,#3484,.T.);
#5086=ORIENTED_EDGE('',*,*,#3562,.F.);
#5087=ORIENTED_EDGE('',*,*,#3563,.F.);
#5088=ORIENTED_EDGE('',*,*,#3534,.T.);
#5089=ORIENTED_EDGE('',*,*,#3501,.T.);
#5090=ORIENTED_EDGE('',*,*,#3561,.T.);
#5091=ORIENTED_EDGE('',*,*,#3564,.F.);
#5092=ORIENTED_EDGE('',*,*,#3565,.T.);
#5093=ORIENTED_EDGE('',*,*,#3487,.T.);
#5094=ORIENTED_EDGE('',*,*,#3566,.T.);
#5095=ORIENTED_EDGE('',*,*,#3567,.T.);
#5096=ORIENTED_EDGE('',*,*,#3562,.T.);
#5097=ORIENTED_EDGE('',*,*,#3502,.T.);
#5098=ORIENTED_EDGE('',*,*,#3565,.F.);
#5099=ORIENTED_EDGE('',*,*,#3568,.F.);
#5100=ORIENTED_EDGE('',*,*,#3523,.F.);
#5101=ORIENTED_EDGE('',*,*,#3486,.T.);
#5102=ORIENTED_EDGE('',*,*,#3533,.F.);
#5103=ORIENTED_EDGE('',*,*,#3569,.F.);
#5104=ORIENTED_EDGE('',*,*,#3566,.F.);
#5105=ORIENTED_EDGE('',*,*,#3496,.T.);
#5106=ORIENTED_EDGE('',*,*,#3525,.T.);
#5107=ORIENTED_EDGE('',*,*,#3570,.F.);
#5108=ORIENTED_EDGE('',*,*,#3571,.F.);
#5109=ORIENTED_EDGE('',*,*,#3488,.T.);
#5110=ORIENTED_EDGE('',*,*,#3572,.F.);
#5111=ORIENTED_EDGE('',*,*,#3573,.F.);
#5112=ORIENTED_EDGE('',*,*,#3531,.T.);
#5113=ORIENTED_EDGE('',*,*,#3497,.T.);
#5114=ORIENTED_EDGE('',*,*,#3571,.T.);
#5115=ORIENTED_EDGE('',*,*,#3574,.F.);
#5116=ORIENTED_EDGE('',*,*,#3575,.T.);
#5117=ORIENTED_EDGE('',*,*,#3491,.T.);
#5118=ORIENTED_EDGE('',*,*,#3576,.T.);
#5119=ORIENTED_EDGE('',*,*,#3577,.T.);
#5120=ORIENTED_EDGE('',*,*,#3572,.T.);
#5121=ORIENTED_EDGE('',*,*,#3498,.T.);
#5122=ORIENTED_EDGE('',*,*,#3575,.F.);
#5123=ORIENTED_EDGE('',*,*,#3578,.F.);
#5124=ORIENTED_EDGE('',*,*,#3526,.F.);
#5125=ORIENTED_EDGE('',*,*,#3490,.T.);
#5126=ORIENTED_EDGE('',*,*,#3530,.F.);
#5127=ORIENTED_EDGE('',*,*,#3579,.F.);
#5128=ORIENTED_EDGE('',*,*,#3576,.F.);
#5129=ORIENTED_EDGE('',*,*,#3549,.T.);
#5130=ORIENTED_EDGE('',*,*,#3538,.T.);
#5131=ORIENTED_EDGE('',*,*,#3553,.T.);
#5132=ORIENTED_EDGE('',*,*,#3557,.F.);
#5133=ORIENTED_EDGE('',*,*,#3559,.T.);
#5134=ORIENTED_EDGE('',*,*,#3535,.T.);
#5135=ORIENTED_EDGE('',*,*,#3563,.T.);
#5136=ORIENTED_EDGE('',*,*,#3567,.F.);
#5137=ORIENTED_EDGE('',*,*,#3569,.T.);
#5138=ORIENTED_EDGE('',*,*,#3532,.T.);
#5139=ORIENTED_EDGE('',*,*,#3573,.T.);
#5140=ORIENTED_EDGE('',*,*,#3577,.F.);
#5141=ORIENTED_EDGE('',*,*,#3579,.T.);
#5142=ORIENTED_EDGE('',*,*,#3529,.T.);
#5143=ORIENTED_EDGE('',*,*,#3580,.T.);
#5144=ORIENTED_EDGE('',*,*,#3581,.T.);
#5145=ORIENTED_EDGE('',*,*,#3582,.F.);
#5146=ORIENTED_EDGE('',*,*,#3513,.T.);
#5147=ORIENTED_EDGE('',*,*,#3543,.T.);
#5148=ORIENTED_EDGE('',*,*,#3547,.F.);
#5149=ORIENTED_EDGE('',*,*,#3528,.T.);
#5150=ORIENTED_EDGE('',*,*,#3583,.F.);
#5151=ORIENTED_EDGE('',*,*,#3584,.F.);
#5152=ORIENTED_EDGE('',*,*,#3580,.F.);
#5153=ORIENTED_EDGE('',*,*,#3548,.T.);
#5154=ORIENTED_EDGE('',*,*,#3544,.T.);
#5155=ORIENTED_EDGE('',*,*,#3540,.T.);
#5156=ORIENTED_EDGE('',*,*,#3515,.T.);
#5157=ORIENTED_EDGE('',*,*,#3585,.F.);
#5158=ORIENTED_EDGE('',*,*,#3586,.F.);
#5159=ORIENTED_EDGE('',*,*,#3583,.T.);
#5160=ORIENTED_EDGE('',*,*,#3527,.T.);
#5161=ORIENTED_EDGE('',*,*,#3578,.T.);
#5162=ORIENTED_EDGE('',*,*,#3574,.T.);
#5163=ORIENTED_EDGE('',*,*,#3570,.T.);
#5164=ORIENTED_EDGE('',*,*,#3524,.T.);
#5165=ORIENTED_EDGE('',*,*,#3568,.T.);
#5166=ORIENTED_EDGE('',*,*,#3564,.T.);
#5167=ORIENTED_EDGE('',*,*,#3560,.T.);
#5168=ORIENTED_EDGE('',*,*,#3521,.T.);
#5169=ORIENTED_EDGE('',*,*,#3558,.T.);
#5170=ORIENTED_EDGE('',*,*,#3554,.T.);
#5171=ORIENTED_EDGE('',*,*,#3550,.T.);
#5172=ORIENTED_EDGE('',*,*,#3518,.T.);
#5173=ORIENTED_EDGE('',*,*,#3584,.T.);
#5174=ORIENTED_EDGE('',*,*,#3586,.T.);
#5175=ORIENTED_EDGE('',*,*,#3587,.F.);
#5176=ORIENTED_EDGE('',*,*,#3581,.F.);
#5177=ORIENTED_EDGE('',*,*,#3468,.T.);
#5178=ORIENTED_EDGE('',*,*,#3471,.T.);
#5179=ORIENTED_EDGE('',*,*,#3474,.T.);
#5180=ORIENTED_EDGE('',*,*,#3477,.T.);
#5181=ORIENTED_EDGE('',*,*,#3514,.T.);
#5182=ORIENTED_EDGE('',*,*,#3582,.T.);
#5183=ORIENTED_EDGE('',*,*,#3587,.T.);
#5184=ORIENTED_EDGE('',*,*,#3585,.T.);
#5185=ORIENTED_EDGE('',*,*,#3588,.F.);
#5186=ORIENTED_EDGE('',*,*,#3589,.F.);
#5187=ORIENTED_EDGE('',*,*,#3590,.F.);
#5188=ORIENTED_EDGE('',*,*,#3591,.F.);
#5189=ORIENTED_EDGE('',*,*,#3592,.F.);
#5190=ORIENTED_EDGE('',*,*,#3593,.F.);
#5191=ORIENTED_EDGE('',*,*,#3594,.F.);
#5192=ORIENTED_EDGE('',*,*,#3595,.F.);
#5193=ORIENTED_EDGE('',*,*,#3596,.F.);
#5194=ORIENTED_EDGE('',*,*,#3590,.T.);
#5195=ORIENTED_EDGE('',*,*,#3597,.F.);
#5196=ORIENTED_EDGE('',*,*,#3594,.T.);
#5197=ORIENTED_EDGE('',*,*,#3595,.T.);
#5198=ORIENTED_EDGE('',*,*,#3597,.T.);
#5199=ORIENTED_EDGE('',*,*,#3589,.T.);
#5200=ORIENTED_EDGE('',*,*,#3598,.F.);
#5201=ORIENTED_EDGE('',*,*,#3599,.F.);
#5202=ORIENTED_EDGE('',*,*,#3600,.T.);
#5203=ORIENTED_EDGE('',*,*,#3601,.T.);
#5204=ORIENTED_EDGE('',*,*,#3602,.F.);
#5205=ORIENTED_EDGE('',*,*,#3588,.T.);
#5206=ORIENTED_EDGE('',*,*,#3603,.T.);
#5207=ORIENTED_EDGE('',*,*,#3604,.T.);
#5208=ORIENTED_EDGE('',*,*,#3598,.T.);
#5209=ORIENTED_EDGE('',*,*,#3605,.T.);
#5210=ORIENTED_EDGE('',*,*,#3606,.T.);
#5211=ORIENTED_EDGE('',*,*,#3607,.F.);
#5212=ORIENTED_EDGE('',*,*,#3601,.F.);
#5213=ORIENTED_EDGE('',*,*,#3608,.T.);
#5214=ORIENTED_EDGE('',*,*,#3599,.T.);
#5215=ORIENTED_EDGE('',*,*,#3604,.F.);
#5216=ORIENTED_EDGE('',*,*,#3609,.F.);
#5217=ORIENTED_EDGE('',*,*,#3593,.T.);
#5218=ORIENTED_EDGE('',*,*,#3610,.F.);
#5219=ORIENTED_EDGE('',*,*,#3606,.F.);
#5220=ORIENTED_EDGE('',*,*,#3611,.T.);
#5221=ORIENTED_EDGE('',*,*,#3609,.T.);
#5222=ORIENTED_EDGE('',*,*,#3603,.F.);
#5223=ORIENTED_EDGE('',*,*,#3591,.T.);
#5224=ORIENTED_EDGE('',*,*,#3596,.T.);
#5225=ORIENTED_EDGE('',*,*,#3592,.T.);
#5226=ORIENTED_EDGE('',*,*,#3602,.T.);
#5227=ORIENTED_EDGE('',*,*,#3607,.T.);
#5228=ORIENTED_EDGE('',*,*,#3610,.T.);
#5229=ORIENTED_EDGE('',*,*,#3611,.F.);
#5230=ORIENTED_EDGE('',*,*,#3605,.F.);
#5231=ORIENTED_EDGE('',*,*,#3600,.F.);
#5232=ORIENTED_EDGE('',*,*,#3608,.F.);
#5233=ORIENTED_EDGE('',*,*,#3612,.T.);
#5234=ORIENTED_EDGE('',*,*,#3613,.T.);
#5235=ORIENTED_EDGE('',*,*,#3614,.F.);
#5236=ORIENTED_EDGE('',*,*,#3615,.F.);
#5237=ORIENTED_EDGE('',*,*,#3616,.T.);
#5238=ORIENTED_EDGE('',*,*,#3615,.T.);
#5239=ORIENTED_EDGE('',*,*,#3617,.F.);
#5240=ORIENTED_EDGE('',*,*,#3618,.F.);
#5241=ORIENTED_EDGE('',*,*,#3619,.T.);
#5242=ORIENTED_EDGE('',*,*,#3618,.T.);
#5243=ORIENTED_EDGE('',*,*,#3620,.F.);
#5244=ORIENTED_EDGE('',*,*,#3621,.F.);
#5245=ORIENTED_EDGE('',*,*,#3622,.T.);
#5246=ORIENTED_EDGE('',*,*,#3621,.T.);
#5247=ORIENTED_EDGE('',*,*,#3623,.F.);
#5248=ORIENTED_EDGE('',*,*,#3613,.F.);
#5249=ORIENTED_EDGE('',*,*,#3623,.T.);
#5250=ORIENTED_EDGE('',*,*,#3620,.T.);
#5251=ORIENTED_EDGE('',*,*,#3617,.T.);
#5252=ORIENTED_EDGE('',*,*,#3614,.T.);
#5253=ORIENTED_EDGE('',*,*,#3622,.F.);
#5254=ORIENTED_EDGE('',*,*,#3612,.F.);
#5255=ORIENTED_EDGE('',*,*,#3616,.F.);
#5256=ORIENTED_EDGE('',*,*,#3619,.F.);
#5257=ORIENTED_EDGE('',*,*,#3624,.F.);
#5258=ORIENTED_EDGE('',*,*,#3625,.T.);
#5259=ORIENTED_EDGE('',*,*,#3626,.T.);
#5260=ORIENTED_EDGE('',*,*,#3625,.F.);
#5261=ORIENTED_EDGE('',*,*,#3624,.T.);
#5262=ORIENTED_EDGE('',*,*,#3626,.F.);
#5263=PLANE('',#5898);
#5264=PLANE('',#5899);
#5265=PLANE('',#5900);
#5266=PLANE('',#5901);
#5267=PLANE('',#5902);
#5268=PLANE('',#5903);
#5269=PLANE('',#5905);
#5270=PLANE('',#5909);
#5271=PLANE('',#5919);
#5272=PLANE('',#5920);
#5273=PLANE('',#5921);
#5274=PLANE('',#5922);
#5275=PLANE('',#5923);
#5276=PLANE('',#5924);
#5277=PLANE('',#5932);
#5278=PLANE('',#5936);
#5279=PLANE('',#5937);
#5280=PLANE('',#5938);
#5281=PLANE('',#5939);
#5282=PLANE('',#5940);
#5283=PLANE('',#5947);
#5284=PLANE('',#5948);
#5285=PLANE('',#5955);
#5286=PLANE('',#5956);
#5287=PLANE('',#5957);
#5288=PLANE('',#5965);
#5289=PLANE('',#5969);
#5290=PLANE('',#5970);
#5291=PLANE('',#5974);
#5292=PLANE('',#5975);
#5293=PLANE('',#5976);
#5294=PLANE('',#5983);
#5295=PLANE('',#5984);
#5296=PLANE('',#5985);
#5297=PLANE('',#5986);
#5298=PLANE('',#5988);
#5299=PLANE('',#5993);
#5300=PLANE('',#5998);
#5301=PLANE('',#6000);
#5302=PLANE('',#6002);
#5303=PLANE('',#6003);
#5304=PLANE('',#6004);
#5305=PLANE('',#6005);
#5306=PLANE('',#6006);
#5307=PLANE('',#6007);
#5308=PLANE('',#6012);
#5309=PLANE('',#6016);
#5310=PLANE('',#6020);
#5311=PLANE('',#6024);
#5312=PLANE('',#6031);
#5313=PLANE('',#6032);
#5314=PLANE('',#6033);
#5315=PLANE('',#6034);
#5316=PLANE('',#6035);
#5317=PLANE('',#6036);
#5318=PLANE('',#6037);
#5319=PLANE('',#6038);
#5320=PLANE('',#6039);
#5321=PLANE('',#6040);
#5322=PLANE('',#6041);
#5323=PLANE('',#6042);
#5324=PLANE('',#6043);
#5325=PLANE('',#6044);
#5326=PLANE('',#6045);
#5327=PLANE('',#6046);
#5328=PLANE('',#6047);
#5329=PLANE('',#6048);
#5330=PLANE('',#6049);
#5331=PLANE('',#6050);
#5332=PLANE('',#6051);
#5333=PLANE('',#6052);
#5334=PLANE('',#6053);
#5335=PLANE('',#6054);
#5336=PLANE('',#6055);
#5337=PLANE('',#6056);
#5338=PLANE('',#6057);
#5339=PLANE('',#6058);
#5340=PLANE('',#6059);
#5341=PLANE('',#6060);
#5342=PLANE('',#6061);
#5343=PLANE('',#6062);
#5344=PLANE('',#6063);
#5345=PLANE('',#6064);
#5346=PLANE('',#6065);
#5347=PLANE('',#6066);
#5348=PLANE('',#6067);
#5349=PLANE('',#6068);
#5350=PLANE('',#6070);
#5351=PLANE('',#6071);
#5352=PLANE('',#6072);
#5353=PLANE('',#6073);
#5354=PLANE('',#6074);
#5355=PLANE('',#6075);
#5356=PLANE('',#6076);
#5357=PLANE('',#6077);
#5358=PLANE('',#6078);
#5359=PLANE('',#6079);
#5360=PLANE('',#6081);
#5361=PLANE('',#6082);
#5362=PLANE('',#6083);
#5363=PLANE('',#6084);
#5364=PLANE('',#6085);
#5365=PLANE('',#6086);
#5366=PLANE('',#6087);
#5367=PLANE('',#6088);
#5368=PLANE('',#6130);
#5369=PLANE('',#6131);
#5370=PLANE('',#6132);
#5371=PLANE('',#6133);
#5372=PLANE('',#6134);
#5373=PLANE('',#6135);
#5374=PLANE('',#6136);
#5375=PLANE('',#6137);
#5376=PLANE('',#6141);
#5377=PLANE('',#6142);
#5378=PLANE('',#6163);
#5379=PLANE('',#6164);
#5380=PLANE('',#6165);
#5381=PLANE('',#6166);
#5382=PLANE('',#6167);
#5383=PLANE('',#6168);
#5384=PLANE('',#6169);
#5385=PLANE('',#6170);
#5386=PLANE('',#6175);
#5387=PLANE('',#6179);
#5388=PLANE('',#6183);
#5389=PLANE('',#6187);
#5390=PLANE('',#6188);
#5391=PLANE('',#6189);
#5392=PLANE('',#6190);
#5393=PLANE('',#6191);
#5394=PLANE('',#6192);
#5395=PLANE('',#6193);
#5396=PLANE('',#6194);
#5397=PLANE('',#6195);
#5398=PLANE('',#6196);
#5399=PLANE('',#6197);
#5400=PLANE('',#6198);
#5401=PLANE('',#6199);
#5402=PLANE('',#6200);
#5403=PLANE('',#6201);
#5404=PLANE('',#6202);
#5405=PLANE('',#6203);
#5406=PLANE('',#6204);
#5407=PLANE('',#6205);
#5408=PLANE('',#6206);
#5409=PLANE('',#6207);
#5410=PLANE('',#6208);
#5411=PLANE('',#6209);
#5412=PLANE('',#6210);
#5413=PLANE('',#6211);
#5414=PLANE('',#6212);
#5415=PLANE('',#6213);
#5416=PLANE('',#6214);
#5417=PLANE('',#6215);
#5418=PLANE('',#6216);
#5419=PLANE('',#6217);
#5420=PLANE('',#6218);
#5421=PLANE('',#6219);
#5422=PLANE('',#6220);
#5423=PLANE('',#6221);
#5424=PLANE('',#6222);
#5425=PLANE('',#6223);
#5426=PLANE('',#6224);
#5427=PLANE('',#6225);
#5428=PLANE('',#6227);
#5429=PLANE('',#6228);
#5430=PLANE('',#6229);
#5431=PLANE('',#6230);
#5432=PLANE('',#6231);
#5433=PLANE('',#6232);
#5434=PLANE('',#6233);
#5435=PLANE('',#6234);
#5436=PLANE('',#6235);
#5437=PLANE('',#6236);
#5438=PLANE('',#6238);
#5439=PLANE('',#6239);
#5440=PLANE('',#6240);
#5441=PLANE('',#6241);
#5442=PLANE('',#6242);
#5443=PLANE('',#6243);
#5444=PLANE('',#6248);
#5445=PLANE('',#6249);
#5446=ADVANCED_FACE('',(#632),#5263,.T.);
#5447=ADVANCED_FACE('',(#633),#5264,.T.);
#5448=ADVANCED_FACE('',(#634),#5265,.T.);
#5449=ADVANCED_FACE('',(#635),#5266,.T.);
#5450=ADVANCED_FACE('',(#636),#5267,.T.);
#5451=ADVANCED_FACE('',(#637),#5268,.F.);
#5452=ADVANCED_FACE('',(#638),#5269,.F.);
#5453=ADVANCED_FACE('',(#639),#490,.F.);
#5454=ADVANCED_FACE('',(#640),#5270,.F.);
#5455=ADVANCED_FACE('',(#641),#491,.F.);
#5456=ADVANCED_FACE('',(#642),#492,.F.);
#5457=ADVANCED_FACE('',(#643),#493,.F.);
#5458=ADVANCED_FACE('',(#644,#381,#382,#383),#5271,.T.);
#5459=ADVANCED_FACE('',(#645),#5272,.T.);
#5460=ADVANCED_FACE('',(#646,#384,#385,#386),#5273,.T.);
#5461=ADVANCED_FACE('',(#647),#5274,.T.);
#5462=ADVANCED_FACE('',(#648),#5275,.T.);
#5463=ADVANCED_FACE('',(#649),#5276,.F.);
#5464=ADVANCED_FACE('',(#650),#494,.F.);
#5465=ADVANCED_FACE('',(#651),#495,.F.);
#5466=ADVANCED_FACE('',(#652),#5277,.F.);
#5467=ADVANCED_FACE('',(#653),#496,.F.);
#5468=ADVANCED_FACE('',(#654),#5278,.T.);
#5469=ADVANCED_FACE('',(#655,#387,#388),#5279,.T.);
#5470=ADVANCED_FACE('',(#656),#5280,.T.);
#5471=ADVANCED_FACE('',(#657),#5281,.T.);
#5472=ADVANCED_FACE('',(#658),#5282,.F.);
#5473=ADVANCED_FACE('',(#659),#497,.T.);
#5474=ADVANCED_FACE('',(#660),#498,.F.);
#5475=ADVANCED_FACE('',(#661,#389),#5283,.T.);
#5476=ADVANCED_FACE('',(#662,#390,#391),#5284,.T.);
#5477=ADVANCED_FACE('',(#663),#499,.F.);
#5478=ADVANCED_FACE('',(#664),#500,.T.);
#5479=ADVANCED_FACE('',(#665),#5285,.T.);
#5480=ADVANCED_FACE('',(#666),#5286,.T.);
#5481=ADVANCED_FACE('',(#667,#392),#5287,.F.);
#5482=ADVANCED_FACE('',(#668),#501,.F.);
#5483=ADVANCED_FACE('',(#669),#502,.F.);
#5484=ADVANCED_FACE('',(#670),#5288,.T.);
#5485=ADVANCED_FACE('',(#671),#503,.F.);
#5486=ADVANCED_FACE('',(#672,#393,#394),#5289,.T.);
#5487=ADVANCED_FACE('',(#673),#5290,.T.);
#5488=ADVANCED_FACE('',(#674),#504,.F.);
#5489=ADVANCED_FACE('',(#675),#5291,.F.);
#5490=ADVANCED_FACE('',(#676),#5292,.F.);
#5491=ADVANCED_FACE('',(#677,#395),#5293,.T.);
#5492=ADVANCED_FACE('',(#678),#505,.F.);
#5493=ADVANCED_FACE('',(#679),#506,.T.);
#5494=ADVANCED_FACE('',(#680,#396),#5294,.F.);
#5495=ADVANCED_FACE('',(#681,#397,#398),#5295,.T.);
#5496=ADVANCED_FACE('',(#682),#5296,.T.);
#5497=ADVANCED_FACE('',(#683),#5297,.T.);
#5498=ADVANCED_FACE('',(#684,#399),#5298,.F.);
#5499=ADVANCED_FACE('',(#685),#507,.T.);
#5500=ADVANCED_FACE('',(#686,#400),#5299,.T.);
#5501=ADVANCED_FACE('',(#687),#508,.T.);
#5502=ADVANCED_FACE('',(#688),#5300,.F.);
#5503=ADVANCED_FACE('',(#689),#509,.T.);
#5504=ADVANCED_FACE('',(#690),#5301,.T.);
#5505=ADVANCED_FACE('',(#691),#5302,.T.);
#5506=ADVANCED_FACE('',(#692),#5303,.T.);
#5507=ADVANCED_FACE('',(#693),#5304,.T.);
#5508=ADVANCED_FACE('',(#694),#5305,.T.);
#5509=ADVANCED_FACE('',(#695),#5306,.T.);
#5510=ADVANCED_FACE('',(#696),#5307,.F.);
#5511=ADVANCED_FACE('',(#697),#510,.F.);
#5512=ADVANCED_FACE('',(#698),#5308,.F.);
#5513=ADVANCED_FACE('',(#699),#511,.F.);
#5514=ADVANCED_FACE('',(#700),#5309,.F.);
#5515=ADVANCED_FACE('',(#701),#512,.F.);
#5516=ADVANCED_FACE('',(#702),#5310,.F.);
#5517=ADVANCED_FACE('',(#703),#513,.F.);
#5518=ADVANCED_FACE('',(#704),#5311,.F.);
#5519=ADVANCED_FACE('',(#705),#514,.F.);
#5520=ADVANCED_FACE('',(#706),#515,.F.);
#5521=ADVANCED_FACE('',(#707),#5312,.F.);
#5522=ADVANCED_FACE('',(#708),#5313,.F.);
#5523=ADVANCED_FACE('',(#709),#5314,.F.);
#5524=ADVANCED_FACE('',(#710),#5315,.F.);
#5525=ADVANCED_FACE('',(#711),#5316,.F.);
#5526=ADVANCED_FACE('',(#712),#5317,.F.);
#5527=ADVANCED_FACE('',(#713),#5318,.F.);
#5528=ADVANCED_FACE('',(#714),#5319,.F.);
#5529=ADVANCED_FACE('',(#715),#5320,.F.);
#5530=ADVANCED_FACE('',(#716),#5321,.T.);
#5531=ADVANCED_FACE('',(#717),#5322,.T.);
#5532=ADVANCED_FACE('',(#718),#5323,.T.);
#5533=ADVANCED_FACE('',(#719),#5324,.T.);
#5534=ADVANCED_FACE('',(#720),#5325,.F.);
#5535=ADVANCED_FACE('',(#721),#5326,.F.);
#5536=ADVANCED_FACE('',(#722),#5327,.T.);
#5537=ADVANCED_FACE('',(#723),#5328,.T.);
#5538=ADVANCED_FACE('',(#724,#401),#5329,.T.);
#5539=ADVANCED_FACE('',(#725),#5330,.T.);
#5540=ADVANCED_FACE('',(#726),#5331,.F.);
#5541=ADVANCED_FACE('',(#727),#5332,.F.);
#5542=ADVANCED_FACE('',(#728),#5333,.T.);
#5543=ADVANCED_FACE('',(#729),#5334,.T.);
#5544=ADVANCED_FACE('',(#730,#402),#5335,.T.);
#5545=ADVANCED_FACE('',(#731),#5336,.T.);
#5546=ADVANCED_FACE('',(#732),#5337,.F.);
#5547=ADVANCED_FACE('',(#733),#5338,.F.);
#5548=ADVANCED_FACE('',(#734),#5339,.T.);
#5549=ADVANCED_FACE('',(#735),#5340,.T.);
#5550=ADVANCED_FACE('',(#736),#5341,.T.);
#5551=ADVANCED_FACE('',(#737),#5342,.T.);
#5552=ADVANCED_FACE('',(#738),#5343,.F.);
#5553=ADVANCED_FACE('',(#739),#5344,.F.);
#5554=ADVANCED_FACE('',(#740),#5345,.T.);
#5555=ADVANCED_FACE('',(#741),#5346,.F.);
#5556=ADVANCED_FACE('',(#742),#5347,.T.);
#5557=ADVANCED_FACE('',(#743,#403,#404,#405,#406,#407,#408),#5348,.T.);
#5558=ADVANCED_FACE('',(#744),#5349,.T.);
#5559=ADVANCED_FACE('',(#745),#5350,.F.);
#5560=ADVANCED_FACE('',(#746),#5351,.F.);
#5561=ADVANCED_FACE('',(#747),#5352,.T.);
#5562=ADVANCED_FACE('',(#748),#5353,.T.);
#5563=ADVANCED_FACE('',(#749),#5354,.T.);
#5564=ADVANCED_FACE('',(#750),#5355,.T.);
#5565=ADVANCED_FACE('',(#751),#5356,.T.);
#5566=ADVANCED_FACE('',(#752),#5357,.T.);
#5567=ADVANCED_FACE('',(#753),#5358,.T.);
#5568=ADVANCED_FACE('',(#754),#5359,.F.);
#5569=ADVANCED_FACE('',(#755),#5360,.F.);
#5570=ADVANCED_FACE('',(#756),#5361,.F.);
#5571=ADVANCED_FACE('',(#757),#5362,.T.);
#5572=ADVANCED_FACE('',(#758),#5363,.T.);
#5573=ADVANCED_FACE('',(#759),#5364,.T.);
#5574=ADVANCED_FACE('',(#760),#5365,.T.);
#5575=ADVANCED_FACE('',(#761),#5366,.T.);
#5576=ADVANCED_FACE('',(#762),#5367,.F.);
#5577=ADVANCED_FACE('',(#763),#516,.T.);
#5578=ADVANCED_FACE('',(#764),#517,.T.);
#5579=ADVANCED_FACE('',(#765),#518,.T.);
#5580=ADVANCED_FACE('',(#766),#519,.T.);
#5581=ADVANCED_FACE('',(#767),#520,.T.);
#5582=ADVANCED_FACE('',(#768),#521,.T.);
#5583=ADVANCED_FACE('',(#769),#522,.T.);
#5584=ADVANCED_FACE('',(#770),#523,.T.);
#5585=ADVANCED_FACE('',(#771),#524,.T.);
#5586=ADVANCED_FACE('',(#772),#525,.T.);
#5587=ADVANCED_FACE('',(#773),#526,.T.);
#5588=ADVANCED_FACE('',(#774),#527,.T.);
#5589=ADVANCED_FACE('',(#775),#528,.T.);
#5590=ADVANCED_FACE('',(#776),#529,.T.);
#5591=ADVANCED_FACE('',(#777),#530,.T.);
#5592=ADVANCED_FACE('',(#778),#531,.T.);
#5593=ADVANCED_FACE('',(#779),#532,.T.);
#5594=ADVANCED_FACE('',(#780),#533,.T.);
#5595=ADVANCED_FACE('',(#781),#534,.T.);
#5596=ADVANCED_FACE('',(#782),#535,.T.);
#5597=ADVANCED_FACE('',(#783),#536,.T.);
#5598=ADVANCED_FACE('',(#784),#537,.T.);
#5599=ADVANCED_FACE('',(#785),#538,.T.);
#5600=ADVANCED_FACE('',(#786),#539,.T.);
#5601=ADVANCED_FACE('',(#787),#540,.T.);
#5602=ADVANCED_FACE('',(#788),#541,.T.);
#5603=ADVANCED_FACE('',(#789),#542,.T.);
#5604=ADVANCED_FACE('',(#790),#543,.T.);
#5605=ADVANCED_FACE('',(#791),#544,.T.);
#5606=ADVANCED_FACE('',(#792),#545,.T.);
#5607=ADVANCED_FACE('',(#793),#546,.T.);
#5608=ADVANCED_FACE('',(#794),#547,.T.);
#5609=ADVANCED_FACE('',(#795),#548,.T.);
#5610=ADVANCED_FACE('',(#796),#549,.T.);
#5611=ADVANCED_FACE('',(#797),#550,.T.);
#5612=ADVANCED_FACE('',(#798),#551,.T.);
#5613=ADVANCED_FACE('',(#799),#139,.F.);
#5614=ADVANCED_FACE('',(#800),#140,.F.);
#5615=ADVANCED_FACE('',(#801),#5368,.F.);
#5616=ADVANCED_FACE('',(#802),#5369,.F.);
#5617=ADVANCED_FACE('',(#803),#5370,.F.);
#5618=ADVANCED_FACE('',(#804),#5371,.F.);
#5619=ADVANCED_FACE('',(#805),#5372,.F.);
#5620=ADVANCED_FACE('',(#806),#5373,.F.);
#5621=ADVANCED_FACE('',(#807),#5374,.F.);
#5622=ADVANCED_FACE('',(#808,#409),#5375,.T.);
#5623=ADVANCED_FACE('',(#809),#552,.T.);
#5624=ADVANCED_FACE('',(#810,#410),#5376,.F.);
#5625=ADVANCED_FACE('',(#811),#5377,.T.);
#5626=ADVANCED_FACE('',(#812),#553,.F.);
#5627=ADVANCED_FACE('',(#813),#554,.F.);
#5628=ADVANCED_FACE('',(#814),#555,.F.);
#5629=ADVANCED_FACE('',(#815),#556,.F.);
#5630=ADVANCED_FACE('',(#816),#557,.F.);
#5631=ADVANCED_FACE('',(#817),#558,.F.);
#5632=ADVANCED_FACE('',(#818),#559,.F.);
#5633=ADVANCED_FACE('',(#819),#560,.F.);
#5634=ADVANCED_FACE('',(#820),#561,.F.);
#5635=ADVANCED_FACE('',(#821),#562,.F.);
#5636=ADVANCED_FACE('',(#822),#563,.F.);
#5637=ADVANCED_FACE('',(#823),#564,.F.);
#5638=ADVANCED_FACE('',(#824),#565,.F.);
#5639=ADVANCED_FACE('',(#825),#566,.F.);
#5640=ADVANCED_FACE('',(#826),#141,.F.);
#5641=ADVANCED_FACE('',(#827),#142,.F.);
#5642=ADVANCED_FACE('',(#828,#411),#5378,.T.);
#5643=ADVANCED_FACE('',(#829),#5379,.T.);
#5644=ADVANCED_FACE('',(#830),#5380,.T.);
#5645=ADVANCED_FACE('',(#831),#5381,.T.);
#5646=ADVANCED_FACE('',(#832),#5382,.T.);
#5647=ADVANCED_FACE('',(#833),#5383,.T.);
#5648=ADVANCED_FACE('',(#834),#5384,.T.);
#5649=ADVANCED_FACE('',(#835,#412),#5385,.F.);
#5650=ADVANCED_FACE('',(#836),#567,.F.);
#5651=ADVANCED_FACE('',(#837),#5386,.F.);
#5652=ADVANCED_FACE('',(#838),#568,.F.);
#5653=ADVANCED_FACE('',(#839),#5387,.F.);
#5654=ADVANCED_FACE('',(#840),#569,.F.);
#5655=ADVANCED_FACE('',(#841),#5388,.F.);
#5656=ADVANCED_FACE('',(#842),#570,.F.);
#5657=ADVANCED_FACE('',(#843),#5389,.F.);
#5658=ADVANCED_FACE('',(#844),#5390,.F.);
#5659=ADVANCED_FACE('',(#845),#5391,.F.);
#5660=ADVANCED_FACE('',(#846),#5392,.F.);
#5661=ADVANCED_FACE('',(#847),#5393,.F.);
#5662=ADVANCED_FACE('',(#848),#5394,.F.);
#5663=ADVANCED_FACE('',(#849),#5395,.F.);
#5664=ADVANCED_FACE('',(#850),#5396,.F.);
#5665=ADVANCED_FACE('',(#851),#5397,.F.);
#5666=ADVANCED_FACE('',(#852),#5398,.F.);
#5667=ADVANCED_FACE('',(#853),#5399,.T.);
#5668=ADVANCED_FACE('',(#854),#5400,.T.);
#5669=ADVANCED_FACE('',(#855),#5401,.T.);
#5670=ADVANCED_FACE('',(#856),#5402,.T.);
#5671=ADVANCED_FACE('',(#857),#5403,.F.);
#5672=ADVANCED_FACE('',(#858),#5404,.F.);
#5673=ADVANCED_FACE('',(#859),#5405,.T.);
#5674=ADVANCED_FACE('',(#860),#5406,.T.);
#5675=ADVANCED_FACE('',(#861),#5407,.T.);
#5676=ADVANCED_FACE('',(#862),#5408,.T.);
#5677=ADVANCED_FACE('',(#863),#5409,.F.);
#5678=ADVANCED_FACE('',(#864),#5410,.F.);
#5679=ADVANCED_FACE('',(#865),#5411,.T.);
#5680=ADVANCED_FACE('',(#866),#5412,.T.);
#5681=ADVANCED_FACE('',(#867),#5413,.T.);
#5682=ADVANCED_FACE('',(#868),#5414,.T.);
#5683=ADVANCED_FACE('',(#869),#5415,.F.);
#5684=ADVANCED_FACE('',(#870),#5416,.F.);
#5685=ADVANCED_FACE('',(#871),#5417,.T.);
#5686=ADVANCED_FACE('',(#872),#5418,.T.);
#5687=ADVANCED_FACE('',(#873),#5419,.T.);
#5688=ADVANCED_FACE('',(#874),#5420,.T.);
#5689=ADVANCED_FACE('',(#875),#5421,.F.);
#5690=ADVANCED_FACE('',(#876),#5422,.F.);
#5691=ADVANCED_FACE('',(#877),#5423,.T.);
#5692=ADVANCED_FACE('',(#878),#5424,.F.);
#5693=ADVANCED_FACE('',(#879),#5425,.T.);
#5694=ADVANCED_FACE('',(#880,#413,#414,#415,#416),#5426,.T.);
#5695=ADVANCED_FACE('',(#881),#5427,.T.);
#5696=ADVANCED_FACE('',(#882),#5428,.F.);
#5697=ADVANCED_FACE('',(#883),#5429,.F.);
#5698=ADVANCED_FACE('',(#884),#5430,.T.);
#5699=ADVANCED_FACE('',(#885),#5431,.T.);
#5700=ADVANCED_FACE('',(#886),#5432,.T.);
#5701=ADVANCED_FACE('',(#887),#5433,.T.);
#5702=ADVANCED_FACE('',(#888),#5434,.T.);
#5703=ADVANCED_FACE('',(#889),#5435,.T.);
#5704=ADVANCED_FACE('',(#890),#5436,.T.);
#5705=ADVANCED_FACE('',(#891),#5437,.F.);
#5706=ADVANCED_FACE('',(#892),#5438,.T.);
#5707=ADVANCED_FACE('',(#893),#5439,.T.);
#5708=ADVANCED_FACE('',(#894),#5440,.T.);
#5709=ADVANCED_FACE('',(#895),#5441,.T.);
#5710=ADVANCED_FACE('',(#896),#5442,.T.);
#5711=ADVANCED_FACE('',(#897),#5443,.F.);
#5712=ADVANCED_FACE('',(#898),#571,.T.);
#5713=ADVANCED_FACE('',(#899),#5444,.T.);
#5714=ADVANCED_FACE('',(#900),#5445,.F.);
#5715=CLOSED_SHELL('',(#5446,#5447,#5448,#5449,#5450,#5451));
#5716=CLOSED_SHELL('',(#5452,#5453,#5454,#5455,#5456,#5457,#5458,#5459,
#5460,#5461,#5462,#5463));
#5717=CLOSED_SHELL('',(#5464,#5465,#5466,#5467,#5468,#5469,#5470,#5471,
#5472,#5473,#5474,#5475,#5476,#5477,#5478,#5479,#5480,#5481));
#5718=CLOSED_SHELL('',(#5482,#5483,#5484,#5485,#5486,#5487,#5488,#5489,
#5490,#5491,#5492,#5493,#5494,#5495,#5496,#5497));
#5719=CLOSED_SHELL('',(#5498,#5499,#5500,#5501,#5502,#5503,#5504));
#5720=CLOSED_SHELL('',(#5505,#5506,#5507,#5508,#5509,#5510));
#5721=CLOSED_SHELL('',(#5511,#5512,#5513,#5514,#5515,#5516,#5517,#5518,
#5519,#5520,#5521,#5522,#5523,#5524,#5525,#5526,#5527,#5528,#5529,#5530,
#5531,#5532,#5533,#5534,#5535,#5536,#5537,#5538,#5539,#5540,#5541,#5542,
#5543,#5544,#5545,#5546,#5547,#5548,#5549,#5550,#5551,#5552,#5553,#5554,
#5555,#5556,#5557,#5558));
#5722=CLOSED_SHELL('',(#5559,#5560,#5561,#5562,#5563,#5564,#5565,#5566,
#5567,#5568));
#5723=CLOSED_SHELL('',(#5569,#5570,#5571,#5572,#5573,#5574,#5575,#5576));
#5724=CLOSED_SHELL('',(#5577,#5578,#5579,#5580,#5581,#5582,#5583,#5584,
#5585,#5586,#5587,#5588,#5589,#5590,#5591,#5592,#5593,#5594,#5595,#5596,
#5597,#5598,#5599,#5600,#5601,#5602,#5603,#5604,#5605,#5606,#5607,#5608,
#5609,#5610,#5611,#5612,#5613,#5614,#5615,#5616,#5617,#5618,#5619,#5620,
#5621,#5622,#5623,#5624,#5625));
#5725=CLOSED_SHELL('',(#5626,#5627,#5628,#5629,#5630,#5631,#5632,#5633,
#5634,#5635,#5636,#5637,#5638,#5639,#5640,#5641,#5642,#5643,#5644,#5645,
#5646,#5647,#5648,#5649));
#5726=CLOSED_SHELL('',(#5650,#5651,#5652,#5653,#5654,#5655,#5656,#5657,
#5658,#5659,#5660,#5661,#5662,#5663,#5664,#5665,#5666,#5667,#5668,#5669,
#5670,#5671,#5672,#5673,#5674,#5675,#5676,#5677,#5678,#5679,#5680,#5681,
#5682,#5683,#5684,#5685,#5686,#5687,#5688,#5689,#5690,#5691,#5692,#5693,
#5694,#5695));
#5727=CLOSED_SHELL('',(#5696,#5697,#5698,#5699,#5700,#5701,#5702,#5703,
#5704,#5705));
#5728=CLOSED_SHELL('',(#5706,#5707,#5708,#5709,#5710,#5711));
#5729=CLOSED_SHELL('',(#5712,#5713,#5714));
#5730=DERIVED_UNIT_ELEMENT(#5760,1.);
#5731=DERIVED_UNIT_ELEMENT(#31568,-3.);
#5732=DERIVED_UNIT_ELEMENT(#5760,1.);
#5733=DERIVED_UNIT_ELEMENT(#31568,-3.);
#5734=DERIVED_UNIT_ELEMENT(#5760,1.);
#5735=DERIVED_UNIT_ELEMENT(#31568,-3.);
#5736=DERIVED_UNIT_ELEMENT(#5760,1.);
#5737=DERIVED_UNIT_ELEMENT(#31568,-3.);
#5738=DERIVED_UNIT_ELEMENT(#5760,1.);
#5739=DERIVED_UNIT_ELEMENT(#31568,-3.);
#5740=DERIVED_UNIT_ELEMENT(#5760,1.);
#5741=DERIVED_UNIT_ELEMENT(#31568,-3.);
#5742=DERIVED_UNIT_ELEMENT(#5760,1.);
#5743=DERIVED_UNIT_ELEMENT(#31568,-3.);
#5744=DERIVED_UNIT_ELEMENT(#5760,1.);
#5745=DERIVED_UNIT_ELEMENT(#31568,-3.);
#5746=DERIVED_UNIT_ELEMENT(#5760,1.);
#5747=DERIVED_UNIT_ELEMENT(#31568,-3.);
#5748=DERIVED_UNIT_ELEMENT(#5760,1.);
#5749=DERIVED_UNIT_ELEMENT(#31568,-3.);
#5750=DERIVED_UNIT_ELEMENT(#5760,1.);
#5751=DERIVED_UNIT_ELEMENT(#31568,-3.);
#5752=DERIVED_UNIT_ELEMENT(#5760,1.);
#5753=DERIVED_UNIT_ELEMENT(#31568,-3.);
#5754=DERIVED_UNIT_ELEMENT(#5760,1.);
#5755=DERIVED_UNIT_ELEMENT(#31568,-3.);
#5756=DERIVED_UNIT_ELEMENT(#5760,1.);
#5757=DERIVED_UNIT_ELEMENT(#31568,-3.);
#5758=DERIVED_UNIT_ELEMENT(#5760,1.);
#5759=DERIVED_UNIT_ELEMENT(#31568,-3.);
#5760=(
MASS_UNIT()
NAMED_UNIT(*)
SI_UNIT(.KILO.,.GRAM.)
);
#5761=DERIVED_UNIT((#5730,#5731));
#5762=DERIVED_UNIT((#5732,#5733));
#5763=DERIVED_UNIT((#5734,#5735));
#5764=DERIVED_UNIT((#5736,#5737));
#5765=DERIVED_UNIT((#5738,#5739));
#5766=DERIVED_UNIT((#5740,#5741));
#5767=DERIVED_UNIT((#5742,#5743));
#5768=DERIVED_UNIT((#5744,#5745));
#5769=DERIVED_UNIT((#5746,#5747));
#5770=DERIVED_UNIT((#5748,#5749));
#5771=DERIVED_UNIT((#5750,#5751));
#5772=DERIVED_UNIT((#5752,#5753));
#5773=DERIVED_UNIT((#5754,#5755));
#5774=DERIVED_UNIT((#5756,#5757));
#5775=DERIVED_UNIT((#5758,#5759));
#5776=MEASURE_REPRESENTATION_ITEM('density measure',
POSITIVE_RATIO_MEASURE(7850.),#5761);
#5777=MEASURE_REPRESENTATION_ITEM('density measure',
POSITIVE_RATIO_MEASURE(7850.),#5762);
#5778=MEASURE_REPRESENTATION_ITEM('density measure',
POSITIVE_RATIO_MEASURE(7850.),#5763);
#5779=MEASURE_REPRESENTATION_ITEM('density measure',
POSITIVE_RATIO_MEASURE(7850.),#5764);
#5780=MEASURE_REPRESENTATION_ITEM('density measure',
POSITIVE_RATIO_MEASURE(7850.),#5765);
#5781=MEASURE_REPRESENTATION_ITEM('density measure',
POSITIVE_RATIO_MEASURE(7850.),#5766);
#5782=MEASURE_REPRESENTATION_ITEM('density measure',
POSITIVE_RATIO_MEASURE(7850.),#5767);
#5783=MEASURE_REPRESENTATION_ITEM('density measure',
POSITIVE_RATIO_MEASURE(7850.),#5768);
#5784=MEASURE_REPRESENTATION_ITEM('density measure',
POSITIVE_RATIO_MEASURE(7850.),#5769);
#5785=MEASURE_REPRESENTATION_ITEM('density measure',
POSITIVE_RATIO_MEASURE(7850.),#5770);
#5786=MEASURE_REPRESENTATION_ITEM('density measure',
POSITIVE_RATIO_MEASURE(7850.),#5771);
#5787=MEASURE_REPRESENTATION_ITEM('density measure',
POSITIVE_RATIO_MEASURE(7850.),#5772);
#5788=MEASURE_REPRESENTATION_ITEM('density measure',
POSITIVE_RATIO_MEASURE(7850.),#5773);
#5789=MEASURE_REPRESENTATION_ITEM('density measure',
POSITIVE_RATIO_MEASURE(7850.),#5774);
#5790=MEASURE_REPRESENTATION_ITEM('density measure',
POSITIVE_RATIO_MEASURE(7850.),#5775);
#5791=PROPERTY_DEFINITION_REPRESENTATION(#5866,#5821);
#5792=PROPERTY_DEFINITION_REPRESENTATION(#5867,#5822);
#5793=PROPERTY_DEFINITION_REPRESENTATION(#5868,#5823);
#5794=PROPERTY_DEFINITION_REPRESENTATION(#5869,#5824);
#5795=PROPERTY_DEFINITION_REPRESENTATION(#5870,#5825);
#5796=PROPERTY_DEFINITION_REPRESENTATION(#5871,#5826);
#5797=PROPERTY_DEFINITION_REPRESENTATION(#5872,#5827);
#5798=PROPERTY_DEFINITION_REPRESENTATION(#5873,#5828);
#5799=PROPERTY_DEFINITION_REPRESENTATION(#5874,#5829);
#5800=PROPERTY_DEFINITION_REPRESENTATION(#5875,#5830);
#5801=PROPERTY_DEFINITION_REPRESENTATION(#5876,#5831);
#5802=PROPERTY_DEFINITION_REPRESENTATION(#5877,#5832);
#5803=PROPERTY_DEFINITION_REPRESENTATION(#5878,#5833);
#5804=PROPERTY_DEFINITION_REPRESENTATION(#5879,#5834);
#5805=PROPERTY_DEFINITION_REPRESENTATION(#5880,#5835);
#5806=PROPERTY_DEFINITION_REPRESENTATION(#5881,#5836);
#5807=PROPERTY_DEFINITION_REPRESENTATION(#5882,#5837);
#5808=PROPERTY_DEFINITION_REPRESENTATION(#5883,#5838);
#5809=PROPERTY_DEFINITION_REPRESENTATION(#5884,#5839);
#5810=PROPERTY_DEFINITION_REPRESENTATION(#5885,#5840);
#5811=PROPERTY_DEFINITION_REPRESENTATION(#5886,#5841);
#5812=PROPERTY_DEFINITION_REPRESENTATION(#5887,#5842);
#5813=PROPERTY_DEFINITION_REPRESENTATION(#5888,#5843);
#5814=PROPERTY_DEFINITION_REPRESENTATION(#5889,#5844);
#5815=PROPERTY_DEFINITION_REPRESENTATION(#5890,#5845);
#5816=PROPERTY_DEFINITION_REPRESENTATION(#5891,#5846);
#5817=PROPERTY_DEFINITION_REPRESENTATION(#5892,#5847);
#5818=PROPERTY_DEFINITION_REPRESENTATION(#5893,#5848);
#5819=PROPERTY_DEFINITION_REPRESENTATION(#5894,#5849);
#5820=PROPERTY_DEFINITION_REPRESENTATION(#5895,#5850);
#5821=REPRESENTATION('material name',(#5851),#31551);
#5822=REPRESENTATION('density',(#5776),#31551);
#5823=REPRESENTATION('material name',(#5852),#31552);
#5824=REPRESENTATION('density',(#5777),#31552);
#5825=REPRESENTATION('material name',(#5853),#31553);
#5826=REPRESENTATION('density',(#5778),#31553);
#5827=REPRESENTATION('material name',(#5854),#31554);
#5828=REPRESENTATION('density',(#5779),#31554);
#5829=REPRESENTATION('material name',(#5855),#31555);
#5830=REPRESENTATION('density',(#5780),#31555);
#5831=REPRESENTATION('material name',(#5856),#31556);
#5832=REPRESENTATION('density',(#5781),#31556);
#5833=REPRESENTATION('material name',(#5857),#31557);
#5834=REPRESENTATION('density',(#5782),#31557);
#5835=REPRESENTATION('material name',(#5858),#31558);
#5836=REPRESENTATION('density',(#5783),#31558);
#5837=REPRESENTATION('material name',(#5859),#31559);
#5838=REPRESENTATION('density',(#5784),#31559);
#5839=REPRESENTATION('material name',(#5860),#31560);
#5840=REPRESENTATION('density',(#5785),#31560);
#5841=REPRESENTATION('material name',(#5861),#31561);
#5842=REPRESENTATION('density',(#5786),#31561);
#5843=REPRESENTATION('material name',(#5862),#31562);
#5844=REPRESENTATION('density',(#5787),#31562);
#5845=REPRESENTATION('material name',(#5863),#31563);
#5846=REPRESENTATION('density',(#5788),#31563);
#5847=REPRESENTATION('material name',(#5864),#31564);
#5848=REPRESENTATION('density',(#5789),#31564);
#5849=REPRESENTATION('material name',(#5865),#31565);
#5850=REPRESENTATION('density',(#5790),#31565);
#5851=DESCRIPTIVE_REPRESENTATION_ITEM('Steel','Steel');
#5852=DESCRIPTIVE_REPRESENTATION_ITEM('Steel','Steel');
#5853=DESCRIPTIVE_REPRESENTATION_ITEM('Steel','Steel');
#5854=DESCRIPTIVE_REPRESENTATION_ITEM('Steel','Steel');
#5855=DESCRIPTIVE_REPRESENTATION_ITEM('Steel','Steel');
#5856=DESCRIPTIVE_REPRESENTATION_ITEM('Steel','Steel');
#5857=DESCRIPTIVE_REPRESENTATION_ITEM('Steel','Steel');
#5858=DESCRIPTIVE_REPRESENTATION_ITEM('Steel','Steel');
#5859=DESCRIPTIVE_REPRESENTATION_ITEM('Steel','Steel');
#5860=DESCRIPTIVE_REPRESENTATION_ITEM('Steel','Steel');
#5861=DESCRIPTIVE_REPRESENTATION_ITEM('Steel','Steel');
#5862=DESCRIPTIVE_REPRESENTATION_ITEM('Steel','Steel');
#5863=DESCRIPTIVE_REPRESENTATION_ITEM('Steel','Steel');
#5864=DESCRIPTIVE_REPRESENTATION_ITEM('Steel','Steel');
#5865=DESCRIPTIVE_REPRESENTATION_ITEM('Steel','Steel');
#5866=PROPERTY_DEFINITION('material property','material name',#31653);
#5867=PROPERTY_DEFINITION('material property','density of part',#31653);
#5868=PROPERTY_DEFINITION('material property','material name',#31654);
#5869=PROPERTY_DEFINITION('material property','density of part',#31654);
#5870=PROPERTY_DEFINITION('material property','material name',#31655);
#5871=PROPERTY_DEFINITION('material property','density of part',#31655);
#5872=PROPERTY_DEFINITION('material property','material name',#31656);
#5873=PROPERTY_DEFINITION('material property','density of part',#31656);
#5874=PROPERTY_DEFINITION('material property','material name',#31657);
#5875=PROPERTY_DEFINITION('material property','density of part',#31657);
#5876=PROPERTY_DEFINITION('material property','material name',#31658);
#5877=PROPERTY_DEFINITION('material property','density of part',#31658);
#5878=PROPERTY_DEFINITION('material property','material name',#31659);
#5879=PROPERTY_DEFINITION('material property','density of part',#31659);
#5880=PROPERTY_DEFINITION('material property','material name',#31660);
#5881=PROPERTY_DEFINITION('material property','density of part',#31660);
#5882=PROPERTY_DEFINITION('material property','material name',#31661);
#5883=PROPERTY_DEFINITION('material property','density of part',#31661);
#5884=PROPERTY_DEFINITION('material property','material name',#31662);
#5885=PROPERTY_DEFINITION('material property','density of part',#31662);
#5886=PROPERTY_DEFINITION('material property','material name',#31663);
#5887=PROPERTY_DEFINITION('material property','density of part',#31663);
#5888=PROPERTY_DEFINITION('material property','material name',#31664);
#5889=PROPERTY_DEFINITION('material property','density of part',#31664);
#5890=PROPERTY_DEFINITION('material property','material name',#31665);
#5891=PROPERTY_DEFINITION('material property','density of part',#31665);
#5892=PROPERTY_DEFINITION('material property','material name',#31666);
#5893=PROPERTY_DEFINITION('material property','density of part',#31666);
#5894=PROPERTY_DEFINITION('material property','material name',#31667);
#5895=PROPERTY_DEFINITION('material property','density of part',#31667);
#5896=AXIS2_PLACEMENT_3D('',#7561,#6282,#6283);
#5897=AXIS2_PLACEMENT_3D('',#7562,#6284,#6285);
#5898=AXIS2_PLACEMENT_3D('',#7563,#6286,#6287);
#5899=AXIS2_PLACEMENT_3D('',#7572,#6292,#6293);
#5900=AXIS2_PLACEMENT_3D('',#7578,#6297,#6298);
#5901=AXIS2_PLACEMENT_3D('',#7584,#6302,#6303);
#5902=AXIS2_PLACEMENT_3D('',#7587,#6306,#6307);
#5903=AXIS2_PLACEMENT_3D('',#7588,#6308,#6309);
#5904=AXIS2_PLACEMENT_3D('',#7589,#6310,#6311);
#5905=AXIS2_PLACEMENT_3D('',#7590,#6312,#6313);
#5906=AXIS2_PLACEMENT_3D('',#7599,#6318,#6319);
#5907=AXIS2_PLACEMENT_3D('',#7601,#6320,#6321);
#5908=AXIS2_PLACEMENT_3D('',#7604,#6323,#6324);
#5909=AXIS2_PLACEMENT_3D('',#7605,#6325,#6326);
#5910=AXIS2_PLACEMENT_3D('',#7611,#6330,#6331);
#5911=AXIS2_PLACEMENT_3D('',#7612,#6332,#6333);
#5912=AXIS2_PLACEMENT_3D('',#7613,#6334,#6335);
#5913=AXIS2_PLACEMENT_3D('',#7614,#6336,#6337);
#5914=AXIS2_PLACEMENT_3D('',#7616,#6338,#6339);
#5915=AXIS2_PLACEMENT_3D('',#7619,#6341,#6342);
#5916=AXIS2_PLACEMENT_3D('',#7620,#6343,#6344);
#5917=AXIS2_PLACEMENT_3D('',#7622,#6345,#6346);
#5918=AXIS2_PLACEMENT_3D('',#7625,#6348,#6349);
#5919=AXIS2_PLACEMENT_3D('',#7626,#6350,#6351);
#5920=AXIS2_PLACEMENT_3D('',#7635,#6356,#6357);
#5921=AXIS2_PLACEMENT_3D('',#7641,#6361,#6362);
#5922=AXIS2_PLACEMENT_3D('',#7647,#6366,#6367);
#5923=AXIS2_PLACEMENT_3D('',#7650,#6370,#6371);
#5924=AXIS2_PLACEMENT_3D('',#7651,#6372,#6373);
#5925=AXIS2_PLACEMENT_3D('',#7652,#6374,#6375);
#5926=AXIS2_PLACEMENT_3D('',#7653,#6376,#6377);
#5927=AXIS2_PLACEMENT_3D('',#7655,#6378,#6379);
#5928=AXIS2_PLACEMENT_3D('',#7658,#6381,#6382);
#5929=AXIS2_PLACEMENT_3D('',#7659,#6383,#6384);
#5930=AXIS2_PLACEMENT_3D('',#7661,#6385,#6386);
#5931=AXIS2_PLACEMENT_3D('',#7664,#6388,#6389);
#5932=AXIS2_PLACEMENT_3D('',#7665,#6390,#6391);
#5933=AXIS2_PLACEMENT_3D('',#7670,#6393,#6394);
#5934=AXIS2_PLACEMENT_3D('',#7674,#6397,#6398);
#5935=AXIS2_PLACEMENT_3D('',#7678,#6400,#6401);
#5936=AXIS2_PLACEMENT_3D('',#7680,#6403,#6404);
#5937=AXIS2_PLACEMENT_3D('',#7686,#6408,#6409);
#5938=AXIS2_PLACEMENT_3D('',#7704,#6419,#6420);
#5939=AXIS2_PLACEMENT_3D('',#7712,#6425,#6426);
#5940=AXIS2_PLACEMENT_3D('',#7720,#6431,#6432);
#5941=AXIS2_PLACEMENT_3D('',#7722,#6433,#6434);
#5942=AXIS2_PLACEMENT_3D('',#7725,#6436,#6437);
#5943=AXIS2_PLACEMENT_3D('',#7726,#6438,#6439);
#5944=AXIS2_PLACEMENT_3D('',#7728,#6440,#6441);
#5945=AXIS2_PLACEMENT_3D('',#7730,#6443,#6444);
#5946=AXIS2_PLACEMENT_3D('',#7733,#6446,#6447);
#5947=AXIS2_PLACEMENT_3D('',#7734,#6448,#6449);
#5948=AXIS2_PLACEMENT_3D('',#7739,#6453,#6454);
#5949=AXIS2_PLACEMENT_3D('',#7751,#6461,#6462);
#5950=AXIS2_PLACEMENT_3D('',#7752,#6463,#6464);
#5951=AXIS2_PLACEMENT_3D('',#7753,#6465,#6466);
#5952=AXIS2_PLACEMENT_3D('',#7754,#6467,#6468);
#5953=AXIS2_PLACEMENT_3D('',#7755,#6469,#6470);
#5954=AXIS2_PLACEMENT_3D('',#7756,#6471,#6472);
#5955=AXIS2_PLACEMENT_3D('',#7757,#6473,#6474);
#5956=AXIS2_PLACEMENT_3D('',#7758,#6475,#6476);
#5957=AXIS2_PLACEMENT_3D('',#7760,#6478,#6479);
#5958=AXIS2_PLACEMENT_3D('',#7761,#6480,#6481);
#5959=AXIS2_PLACEMENT_3D('',#7762,#6482,#6483);
#5960=AXIS2_PLACEMENT_3D('',#7764,#6484,#6485);
#5961=AXIS2_PLACEMENT_3D('',#7767,#6487,#6488);
#5962=AXIS2_PLACEMENT_3D('',#7768,#6489,#6490);
#5963=AXIS2_PLACEMENT_3D('',#7770,#6491,#6492);
#5964=AXIS2_PLACEMENT_3D('',#7773,#6494,#6495);
#5965=AXIS2_PLACEMENT_3D('',#7774,#6496,#6497);
#5966=AXIS2_PLACEMENT_3D('',#7779,#6499,#6500);
#5967=AXIS2_PLACEMENT_3D('',#7781,#6502,#6503);
#5968=AXIS2_PLACEMENT_3D('',#7785,#6505,#6506);
#5969=AXIS2_PLACEMENT_3D('',#7787,#6508,#6509);
#5970=AXIS2_PLACEMENT_3D('',#7807,#6520,#6521);
#5971=AXIS2_PLACEMENT_3D('',#7822,#6530,#6531);
#5972=AXIS2_PLACEMENT_3D('',#7823,#6532,#6533);
#5973=AXIS2_PLACEMENT_3D('',#7824,#6534,#6535);
#5974=AXIS2_PLACEMENT_3D('',#7825,#6536,#6537);
#5975=AXIS2_PLACEMENT_3D('',#7826,#6538,#6539);
#5976=AXIS2_PLACEMENT_3D('',#7830,#6542,#6543);
#5977=AXIS2_PLACEMENT_3D('',#7831,#6544,#6545);
#5978=AXIS2_PLACEMENT_3D('',#7833,#6546,#6547);
#5979=AXIS2_PLACEMENT_3D('',#7834,#6548,#6549);
#5980=AXIS2_PLACEMENT_3D('',#7836,#6550,#6551);
#5981=AXIS2_PLACEMENT_3D('',#7838,#6553,#6554);
#5982=AXIS2_PLACEMENT_3D('',#7839,#6555,#6556);
#5983=AXIS2_PLACEMENT_3D('',#7840,#6557,#6558);
#5984=AXIS2_PLACEMENT_3D('',#7841,#6559,#6560);
#5985=AXIS2_PLACEMENT_3D('',#7845,#6563,#6564);
#5986=AXIS2_PLACEMENT_3D('',#7847,#6566,#6567);
#5987=AXIS2_PLACEMENT_3D('',#7848,#6568,#6569);
#5988=AXIS2_PLACEMENT_3D('',#7849,#6570,#6571);
#5989=AXIS2_PLACEMENT_3D('',#7851,#6572,#6573);
#5990=AXIS2_PLACEMENT_3D('',#7853,#6574,#6575);
#5991=AXIS2_PLACEMENT_3D('',#7854,#6576,#6577);
#5992=AXIS2_PLACEMENT_3D('',#7856,#6578,#6579);
#5993=AXIS2_PLACEMENT_3D('',#7858,#6581,#6582);
#5994=AXIS2_PLACEMENT_3D('',#7860,#6583,#6584);
#5995=AXIS2_PLACEMENT_3D('',#7862,#6585,#6586);
#5996=AXIS2_PLACEMENT_3D('',#7863,#6587,#6588);
#5997=AXIS2_PLACEMENT_3D('',#7866,#6590,#6591);
#5998=AXIS2_PLACEMENT_3D('',#7867,#6592,#6593);
#5999=AXIS2_PLACEMENT_3D('',#7868,#6594,#6595);
#6000=AXIS2_PLACEMENT_3D('',#7870,#6597,#6598);
#6001=AXIS2_PLACEMENT_3D('',#7871,#6599,#6600);
#6002=AXIS2_PLACEMENT_3D('',#7872,#6601,#6602);
#6003=AXIS2_PLACEMENT_3D('',#7881,#6607,#6608);
#6004=AXIS2_PLACEMENT_3D('',#7887,#6612,#6613);
#6005=AXIS2_PLACEMENT_3D('',#7893,#6617,#6618);
#6006=AXIS2_PLACEMENT_3D('',#7896,#6621,#6622);
#6007=AXIS2_PLACEMENT_3D('',#7897,#6623,#6624);
#6008=AXIS2_PLACEMENT_3D('',#7898,#6625,#6626);
#6009=AXIS2_PLACEMENT_3D('',#7899,#6627,#6628);
#6010=AXIS2_PLACEMENT_3D('',#7901,#6629,#6630);
#6011=AXIS2_PLACEMENT_3D('',#7904,#6632,#6633);
#6012=AXIS2_PLACEMENT_3D('',#7905,#6634,#6635);
#6013=AXIS2_PLACEMENT_3D('',#7906,#6636,#6637);
#6014=AXIS2_PLACEMENT_3D('',#7908,#6638,#6639);
#6015=AXIS2_PLACEMENT_3D('',#7911,#6641,#6642);
#6016=AXIS2_PLACEMENT_3D('',#7912,#6643,#6644);
#6017=AXIS2_PLACEMENT_3D('',#7913,#6645,#6646);
#6018=AXIS2_PLACEMENT_3D('',#7915,#6647,#6648);
#6019=AXIS2_PLACEMENT_3D('',#7918,#6650,#6651);
#6020=AXIS2_PLACEMENT_3D('',#7919,#6652,#6653);
#6021=AXIS2_PLACEMENT_3D('',#7920,#6654,#6655);
#6022=AXIS2_PLACEMENT_3D('',#7922,#6656,#6657);
#6023=AXIS2_PLACEMENT_3D('',#7925,#6659,#6660);
#6024=AXIS2_PLACEMENT_3D('',#7926,#6661,#6662);
#6025=AXIS2_PLACEMENT_3D('',#7927,#6663,#6664);
#6026=AXIS2_PLACEMENT_3D('',#7929,#6665,#6666);
#6027=AXIS2_PLACEMENT_3D('',#7932,#6668,#6669);
#6028=AXIS2_PLACEMENT_3D('',#7933,#6670,#6671);
#6029=AXIS2_PLACEMENT_3D('',#7935,#6672,#6673);
#6030=AXIS2_PLACEMENT_3D('',#7938,#6675,#6676);
#6031=AXIS2_PLACEMENT_3D('',#7939,#6677,#6678);
#6032=AXIS2_PLACEMENT_3D('',#7948,#6683,#6684);
#6033=AXIS2_PLACEMENT_3D('',#7957,#6689,#6690);
#6034=AXIS2_PLACEMENT_3D('',#7966,#6695,#6696);
#6035=AXIS2_PLACEMENT_3D('',#7975,#6701,#6702);
#6036=AXIS2_PLACEMENT_3D('',#7984,#6707,#6708);
#6037=AXIS2_PLACEMENT_3D('',#7993,#6713,#6714);
#6038=AXIS2_PLACEMENT_3D('',#8002,#6719,#6720);
#6039=AXIS2_PLACEMENT_3D('',#8011,#6725,#6726);
#6040=AXIS2_PLACEMENT_3D('',#8060,#6755,#6756);
#6041=AXIS2_PLACEMENT_3D('',#8064,#6759,#6760);
#6042=AXIS2_PLACEMENT_3D('',#8068,#6763,#6764);
#6043=AXIS2_PLACEMENT_3D('',#8072,#6767,#6768);
#6044=AXIS2_PLACEMENT_3D('',#8076,#6771,#6772);
#6045=AXIS2_PLACEMENT_3D('',#8078,#6774,#6775);
#6046=AXIS2_PLACEMENT_3D('',#8080,#6777,#6778);
#6047=AXIS2_PLACEMENT_3D('',#8084,#6781,#6782);
#6048=AXIS2_PLACEMENT_3D('',#8088,#6785,#6786);
#6049=AXIS2_PLACEMENT_3D('',#8092,#6789,#6790);
#6050=AXIS2_PLACEMENT_3D('',#8096,#6793,#6794);
#6051=AXIS2_PLACEMENT_3D('',#8098,#6796,#6797);
#6052=AXIS2_PLACEMENT_3D('',#8100,#6799,#6800);
#6053=AXIS2_PLACEMENT_3D('',#8104,#6803,#6804);
#6054=AXIS2_PLACEMENT_3D('',#8108,#6807,#6808);
#6055=AXIS2_PLACEMENT_3D('',#8112,#6811,#6812);
#6056=AXIS2_PLACEMENT_3D('',#8116,#6815,#6816);
#6057=AXIS2_PLACEMENT_3D('',#8118,#6818,#6819);
#6058=AXIS2_PLACEMENT_3D('',#8120,#6821,#6822);
#6059=AXIS2_PLACEMENT_3D('',#8124,#6825,#6826);
#6060=AXIS2_PLACEMENT_3D('',#8128,#6829,#6830);
#6061=AXIS2_PLACEMENT_3D('',#8132,#6833,#6834);
#6062=AXIS2_PLACEMENT_3D('',#8136,#6837,#6838);
#6063=AXIS2_PLACEMENT_3D('',#8138,#6840,#6841);
#6064=AXIS2_PLACEMENT_3D('',#8140,#6843,#6844);
#6065=AXIS2_PLACEMENT_3D('',#8146,#6848,#6849);
#6066=AXIS2_PLACEMENT_3D('',#8150,#6852,#6853);
#6067=AXIS2_PLACEMENT_3D('',#8154,#6856,#6857);
#6068=AXIS2_PLACEMENT_3D('',#8156,#6859,#6860);
#6069=AXIS2_PLACEMENT_3D('',#8157,#6861,#6862);
#6070=AXIS2_PLACEMENT_3D('',#8158,#6863,#6864);
#6071=AXIS2_PLACEMENT_3D('',#8167,#6869,#6870);
#6072=AXIS2_PLACEMENT_3D('',#8176,#6875,#6876);
#6073=AXIS2_PLACEMENT_3D('',#8179,#6879,#6880);
#6074=AXIS2_PLACEMENT_3D('',#8189,#6886,#6887);
#6075=AXIS2_PLACEMENT_3D('',#8193,#6890,#6891);
#6076=AXIS2_PLACEMENT_3D('',#8199,#6895,#6896);
#6077=AXIS2_PLACEMENT_3D('',#8203,#6899,#6900);
#6078=AXIS2_PLACEMENT_3D('',#8206,#6903,#6904);
#6079=AXIS2_PLACEMENT_3D('',#8207,#6905,#6906);
#6080=AXIS2_PLACEMENT_3D('',#8208,#6907,#6908);
#6081=AXIS2_PLACEMENT_3D('',#8209,#6909,#6910);
#6082=AXIS2_PLACEMENT_3D('',#8218,#6915,#6916);
#6083=AXIS2_PLACEMENT_3D('',#8224,#6920,#6921);
#6084=AXIS2_PLACEMENT_3D('',#8230,#6925,#6926);
#6085=AXIS2_PLACEMENT_3D('',#8236,#6930,#6931);
#6086=AXIS2_PLACEMENT_3D('',#8242,#6935,#6936);
#6087=AXIS2_PLACEMENT_3D('',#8245,#6939,#6940);
#6088=AXIS2_PLACEMENT_3D('',#8246,#6941,#6942);
#6089=AXIS2_PLACEMENT_3D('',#8247,#6943,#6944);
#6090=AXIS2_PLACEMENT_3D('',#8248,#6945,#6946);
#6091=AXIS2_PLACEMENT_3D('',#8434,#6948,#6949);
#6092=AXIS2_PLACEMENT_3D('',#8481,#6950,#6951);
#6093=AXIS2_PLACEMENT_3D('',#8926,#6953,#6954);
#6094=AXIS2_PLACEMENT_3D('',#9413,#6956,#6957);
#6095=AXIS2_PLACEMENT_3D('',#9900,#6959,#6960);
#6096=AXIS2_PLACEMENT_3D('',#10401,#6962,#6963);
#6097=AXIS2_PLACEMENT_3D('',#10754,#6965,#6966);
#6098=AXIS2_PLACEMENT_3D('',#10878,#6968,#6969);
#6099=AXIS2_PLACEMENT_3D('',#11179,#6971,#6972);
#6100=AXIS2_PLACEMENT_3D('',#11608,#6974,#6975);
#6101=AXIS2_PLACEMENT_3D('',#12111,#6977,#6978);
#6102=AXIS2_PLACEMENT_3D('',#12610,#6980,#6981);
#6103=AXIS2_PLACEMENT_3D('',#13149,#6983,#6984);
#6104=AXIS2_PLACEMENT_3D('',#13800,#6986,#6987);
#6105=AXIS2_PLACEMENT_3D('',#14301,#6989,#6990);
#6106=AXIS2_PLACEMENT_3D('',#14802,#6992,#6993);
#6107=AXIS2_PLACEMENT_3D('',#15285,#6995,#6996);
#6108=AXIS2_PLACEMENT_3D('',#15780,#6998,#6999);
#6109=AXIS2_PLACEMENT_3D('',#16137,#7001,#7002);
#6110=AXIS2_PLACEMENT_3D('',#16264,#7004,#7005);
#6111=AXIS2_PLACEMENT_3D('',#16559,#7007,#7008);
#6112=AXIS2_PLACEMENT_3D('',#17004,#7010,#7011);
#6113=AXIS2_PLACEMENT_3D('',#17531,#7013,#7014);
#6114=AXIS2_PLACEMENT_3D('',#18096,#7016,#7017);
#6115=AXIS2_PLACEMENT_3D('',#18601,#7019,#7020);
#6116=AXIS2_PLACEMENT_3D('',#19070,#7022,#7023);
#6117=AXIS2_PLACEMENT_3D('',#19535,#7025,#7026);
#6118=AXIS2_PLACEMENT_3D('',#20026,#7028,#7029);
#6119=AXIS2_PLACEMENT_3D('',#20348,#7031,#7032);
#6120=AXIS2_PLACEMENT_3D('',#20824,#7034,#7035);
#6121=AXIS2_PLACEMENT_3D('',#21282,#7037,#7038);
#6122=AXIS2_PLACEMENT_3D('',#21583,#7040,#7041);
#6123=AXIS2_PLACEMENT_3D('',#21931,#7043,#7044);
#6124=AXIS2_PLACEMENT_3D('',#22283,#7046,#7047);
#6125=AXIS2_PLACEMENT_3D('',#22778,#7049,#7050);
#6126=AXIS2_PLACEMENT_3D('',#22819,#7051,#7052);
#6127=AXIS2_PLACEMENT_3D('',#24487,#7053,#7054);
#6128=AXIS2_PLACEMENT_3D('',#26222,#7055,#7056);
#6129=AXIS2_PLACEMENT_3D('',#26463,#7057,#7058);
#6130=AXIS2_PLACEMENT_3D('',#28547,#7059,#7060);
#6131=AXIS2_PLACEMENT_3D('',#28556,#7065,#7066);
#6132=AXIS2_PLACEMENT_3D('',#28562,#7070,#7071);
#6133=AXIS2_PLACEMENT_3D('',#28568,#7075,#7076);
#6134=AXIS2_PLACEMENT_3D('',#28574,#7080,#7081);
#6135=AXIS2_PLACEMENT_3D('',#28580,#7085,#7086);
#6136=AXIS2_PLACEMENT_3D('',#28583,#7089,#7090);
#6137=AXIS2_PLACEMENT_3D('',#28584,#7091,#7092);
#6138=AXIS2_PLACEMENT_3D('',#28586,#7093,#7094);
#6139=AXIS2_PLACEMENT_3D('',#28587,#7095,#7096);
#6140=AXIS2_PLACEMENT_3D('',#28590,#7098,#7099);
#6141=AXIS2_PLACEMENT_3D('',#28591,#7100,#7101);
#6142=AXIS2_PLACEMENT_3D('',#28592,#7102,#7103);
#6143=AXIS2_PLACEMENT_3D('',#28593,#7104,#7105);
#6144=AXIS2_PLACEMENT_3D('',#28594,#7106,#7107);
#6145=AXIS2_PLACEMENT_3D('',#28604,#7109,#7110);
#6146=AXIS2_PLACEMENT_3D('',#28624,#7111,#7112);
#6147=AXIS2_PLACEMENT_3D('',#28760,#7114,#7115);
#6148=AXIS2_PLACEMENT_3D('',#28902,#7117,#7118);
#6149=AXIS2_PLACEMENT_3D('',#29038,#7120,#7121);
#6150=AXIS2_PLACEMENT_3D('',#29109,#7123,#7124);
#6151=AXIS2_PLACEMENT_3D('',#29127,#7126,#7127);
#6152=AXIS2_PLACEMENT_3D('',#29170,#7128,#7129);
#6153=AXIS2_PLACEMENT_3D('',#29175,#7131,#7132);
#6154=AXIS2_PLACEMENT_3D('',#29183,#7133,#7134);
#6155=AXIS2_PLACEMENT_3D('',#29267,#7136,#7137);
#6156=AXIS2_PLACEMENT_3D('',#29418,#7138,#7139);
#6157=AXIS2_PLACEMENT_3D('',#29714,#7141,#7142);
#6158=AXIS2_PLACEMENT_3D('',#30017,#7144,#7145);
#6159=AXIS2_PLACEMENT_3D('',#30190,#7147,#7148);
#6160=AXIS2_PLACEMENT_3D('',#30271,#7150,#7151);
#6161=AXIS2_PLACEMENT_3D('',#30365,#7152,#7153);
#6162=AXIS2_PLACEMENT_3D('',#30568,#7154,#7155);
#6163=AXIS2_PLACEMENT_3D('',#31129,#7156,#7157);
#6164=AXIS2_PLACEMENT_3D('',#31142,#7164,#7165);
#6165=AXIS2_PLACEMENT_3D('',#31148,#7169,#7170);
#6166=AXIS2_PLACEMENT_3D('',#31152,#7173,#7174);
#6167=AXIS2_PLACEMENT_3D('',#31156,#7177,#7178);
#6168=AXIS2_PLACEMENT_3D('',#31160,#7181,#7182);
#6169=AXIS2_PLACEMENT_3D('',#31164,#7185,#7186);
#6170=AXIS2_PLACEMENT_3D('',#31166,#7188,#7189);
#6171=AXIS2_PLACEMENT_3D('',#31167,#7190,#7191);
#6172=AXIS2_PLACEMENT_3D('',#31168,#7192,#7193);
#6173=AXIS2_PLACEMENT_3D('',#31170,#7194,#7195);
#6174=AXIS2_PLACEMENT_3D('',#31173,#7197,#7198);
#6175=AXIS2_PLACEMENT_3D('',#31174,#7199,#7200);
#6176=AXIS2_PLACEMENT_3D('',#31175,#7201,#7202);
#6177=AXIS2_PLACEMENT_3D('',#31177,#7203,#7204);
#6178=AXIS2_PLACEMENT_3D('',#31180,#7206,#7207);
#6179=AXIS2_PLACEMENT_3D('',#31181,#7208,#7209);
#6180=AXIS2_PLACEMENT_3D('',#31182,#7210,#7211);
#6181=AXIS2_PLACEMENT_3D('',#31184,#7212,#7213);
#6182=AXIS2_PLACEMENT_3D('',#31187,#7215,#7216);
#6183=AXIS2_PLACEMENT_3D('',#31188,#7217,#7218);
#6184=AXIS2_PLACEMENT_3D('',#31189,#7219,#7220);
#6185=AXIS2_PLACEMENT_3D('',#31191,#7221,#7222);
#6186=AXIS2_PLACEMENT_3D('',#31194,#7224,#7225);
#6187=AXIS2_PLACEMENT_3D('',#31195,#7226,#7227);
#6188=AXIS2_PLACEMENT_3D('',#31196,#7228,#7229);
#6189=AXIS2_PLACEMENT_3D('',#31205,#7234,#7235);
#6190=AXIS2_PLACEMENT_3D('',#31214,#7240,#7241);
#6191=AXIS2_PLACEMENT_3D('',#31223,#7246,#7247);
#6192=AXIS2_PLACEMENT_3D('',#31232,#7252,#7253);
#6193=AXIS2_PLACEMENT_3D('',#31241,#7258,#7259);
#6194=AXIS2_PLACEMENT_3D('',#31250,#7264,#7265);
#6195=AXIS2_PLACEMENT_3D('',#31259,#7270,#7271);
#6196=AXIS2_PLACEMENT_3D('',#31268,#7276,#7277);
#6197=AXIS2_PLACEMENT_3D('',#31317,#7306,#7307);
#6198=AXIS2_PLACEMENT_3D('',#31321,#7310,#7311);
#6199=AXIS2_PLACEMENT_3D('',#31325,#7314,#7315);
#6200=AXIS2_PLACEMENT_3D('',#31329,#7318,#7319);
#6201=AXIS2_PLACEMENT_3D('',#31333,#7322,#7323);
#6202=AXIS2_PLACEMENT_3D('',#31335,#7325,#7326);
#6203=AXIS2_PLACEMENT_3D('',#31337,#7328,#7329);
#6204=AXIS2_PLACEMENT_3D('',#31341,#7332,#7333);
#6205=AXIS2_PLACEMENT_3D('',#31345,#7336,#7337);
#6206=AXIS2_PLACEMENT_3D('',#31349,#7340,#7341);
#6207=AXIS2_PLACEMENT_3D('',#31353,#7344,#7345);
#6208=AXIS2_PLACEMENT_3D('',#31355,#7347,#7348);
#6209=AXIS2_PLACEMENT_3D('',#31357,#7350,#7351);
#6210=AXIS2_PLACEMENT_3D('',#31361,#7354,#7355);
#6211=AXIS2_PLACEMENT_3D('',#31365,#7358,#7359);
#6212=AXIS2_PLACEMENT_3D('',#31369,#7362,#7363);
#6213=AXIS2_PLACEMENT_3D('',#31373,#7366,#7367);
#6214=AXIS2_PLACEMENT_3D('',#31375,#7369,#7370);
#6215=AXIS2_PLACEMENT_3D('',#31377,#7372,#7373);
#6216=AXIS2_PLACEMENT_3D('',#31381,#7376,#7377);
#6217=AXIS2_PLACEMENT_3D('',#31385,#7380,#7381);
#6218=AXIS2_PLACEMENT_3D('',#31389,#7384,#7385);
#6219=AXIS2_PLACEMENT_3D('',#31393,#7388,#7389);
#6220=AXIS2_PLACEMENT_3D('',#31395,#7391,#7392);
#6221=AXIS2_PLACEMENT_3D('',#31397,#7394,#7395);
#6222=AXIS2_PLACEMENT_3D('',#31403,#7399,#7400);
#6223=AXIS2_PLACEMENT_3D('',#31407,#7403,#7404);
#6224=AXIS2_PLACEMENT_3D('',#31411,#7407,#7408);
#6225=AXIS2_PLACEMENT_3D('',#31413,#7410,#7411);
#6226=AXIS2_PLACEMENT_3D('',#31414,#7412,#7413);
#6227=AXIS2_PLACEMENT_3D('',#31415,#7414,#7415);
#6228=AXIS2_PLACEMENT_3D('',#31424,#7420,#7421);
#6229=AXIS2_PLACEMENT_3D('',#31433,#7426,#7427);
#6230=AXIS2_PLACEMENT_3D('',#31436,#7430,#7431);
#6231=AXIS2_PLACEMENT_3D('',#31446,#7437,#7438);
#6232=AXIS2_PLACEMENT_3D('',#31450,#7441,#7442);
#6233=AXIS2_PLACEMENT_3D('',#31456,#7446,#7447);
#6234=AXIS2_PLACEMENT_3D('',#31460,#7450,#7451);
#6235=AXIS2_PLACEMENT_3D('',#31463,#7454,#7455);
#6236=AXIS2_PLACEMENT_3D('',#31464,#7456,#7457);
#6237=AXIS2_PLACEMENT_3D('',#31465,#7458,#7459);
#6238=AXIS2_PLACEMENT_3D('',#31466,#7460,#7461);
#6239=AXIS2_PLACEMENT_3D('',#31475,#7466,#7467);
#6240=AXIS2_PLACEMENT_3D('',#31481,#7471,#7472);
#6241=AXIS2_PLACEMENT_3D('',#31487,#7476,#7477);
#6242=AXIS2_PLACEMENT_3D('',#31490,#7480,#7481);
#6243=AXIS2_PLACEMENT_3D('',#31491,#7482,#7483);
#6244=AXIS2_PLACEMENT_3D('',#31492,#7484,#7485);
#6245=AXIS2_PLACEMENT_3D('',#31493,#7486,#7487);
#6246=AXIS2_PLACEMENT_3D('',#31495,#7488,#7489);
#6247=AXIS2_PLACEMENT_3D('',#31498,#7491,#7492);
#6248=AXIS2_PLACEMENT_3D('',#31499,#7493,#7494);
#6249=AXIS2_PLACEMENT_3D('',#31500,#7495,#7496);
#6250=AXIS2_PLACEMENT_3D('',#31501,#7497,#7498);
#6251=AXIS2_PLACEMENT_3D('',#31502,#7499,#7500);
#6252=AXIS2_PLACEMENT_3D('',#31503,#7501,#7502);
#6253=AXIS2_PLACEMENT_3D('',#31504,#7503,#7504);
#6254=AXIS2_PLACEMENT_3D('',#31505,#7505,#7506);
#6255=AXIS2_PLACEMENT_3D('',#31506,#7507,#7508);
#6256=AXIS2_PLACEMENT_3D('',#31507,#7509,#7510);
#6257=AXIS2_PLACEMENT_3D('',#31508,#7511,#7512);
#6258=AXIS2_PLACEMENT_3D('',#31509,#7513,#7514);
#6259=AXIS2_PLACEMENT_3D('',#31510,#7515,#7516);
#6260=AXIS2_PLACEMENT_3D('',#31511,#7517,#7518);
#6261=AXIS2_PLACEMENT_3D('',#31512,#7519,#7520);
#6262=AXIS2_PLACEMENT_3D('',#31513,#7521,#7522);
#6263=AXIS2_PLACEMENT_3D('',#31514,#7523,#7524);
#6264=AXIS2_PLACEMENT_3D('',#31515,#7525,#7526);
#6265=AXIS2_PLACEMENT_3D('',#31516,#7527,#7528);
#6266=AXIS2_PLACEMENT_3D('',#31517,#7529,#7530);
#6267=AXIS2_PLACEMENT_3D('',#31518,#7531,#7532);
#6268=AXIS2_PLACEMENT_3D('',#31519,#7533,#7534);
#6269=AXIS2_PLACEMENT_3D('',#31520,#7535,#7536);
#6270=AXIS2_PLACEMENT_3D('',#31521,#7537,#7538);
#6271=AXIS2_PLACEMENT_3D('',#31522,#7539,#7540);
#6272=AXIS2_PLACEMENT_3D('',#31523,#7541,#7542);
#6273=AXIS2_PLACEMENT_3D('',#31524,#7543,#7544);
#6274=AXIS2_PLACEMENT_3D('',#31525,#7545,#7546);
#6275=AXIS2_PLACEMENT_3D('',#31526,#7547,#7548);
#6276=AXIS2_PLACEMENT_3D('',#31527,#7549,#7550);
#6277=AXIS2_PLACEMENT_3D('',#31528,#7551,#7552);
#6278=AXIS2_PLACEMENT_3D('',#31529,#7553,#7554);
#6279=AXIS2_PLACEMENT_3D('',#31530,#7555,#7556);
#6280=AXIS2_PLACEMENT_3D('',#31531,#7557,#7558);
#6281=AXIS2_PLACEMENT_3D('',#31532,#7559,#7560);
#6282=DIRECTION('axis',(0.,0.,1.));
#6283=DIRECTION('refdir',(1.,0.,0.));
#6284=DIRECTION('axis',(0.,0.,1.));
#6285=DIRECTION('refdir',(1.,0.,0.));
#6286=DIRECTION('center_axis',(0.,1.,0.));
#6287=DIRECTION('ref_axis',(-1.,0.,0.));
#6288=DIRECTION('',(-1.,0.,0.));
#6289=DIRECTION('',(0.,0.,1.));
#6290=DIRECTION('',(-1.,0.,0.));
#6291=DIRECTION('',(0.,0.,1.));
#6292=DIRECTION('center_axis',(1.,0.,0.));
#6293=DIRECTION('ref_axis',(0.,1.,0.));
#6294=DIRECTION('',(0.,1.,0.));
#6295=DIRECTION('',(0.,1.,0.));
#6296=DIRECTION('',(0.,0.,1.));
#6297=DIRECTION('center_axis',(0.,-1.,0.));
#6298=DIRECTION('ref_axis',(1.,0.,0.));
#6299=DIRECTION('',(1.,0.,0.));
#6300=DIRECTION('',(1.,0.,0.));
#6301=DIRECTION('',(0.,0.,1.));
#6302=DIRECTION('center_axis',(-1.,0.,0.));
#6303=DIRECTION('ref_axis',(0.,-1.,0.));
#6304=DIRECTION('',(0.,-1.,0.));
#6305=DIRECTION('',(0.,-1.,0.));
#6306=DIRECTION('center_axis',(0.,0.,1.));
#6307=DIRECTION('ref_axis',(1.,0.,0.));
#6308=DIRECTION('center_axis',(0.,0.,1.));
#6309=DIRECTION('ref_axis',(1.,0.,0.));
#6310=DIRECTION('axis',(0.,0.,1.));
#6311=DIRECTION('refdir',(1.,0.,0.));
#6312=DIRECTION('center_axis',(0.,0.,-1.));
#6313=DIRECTION('ref_axis',(1.,0.,0.));
#6314=DIRECTION('',(1.,0.,0.));
#6315=DIRECTION('',(0.,-1.,0.));
#6316=DIRECTION('',(-1.,0.,0.));
#6317=DIRECTION('',(0.,-1.,0.));
#6318=DIRECTION('center_axis',(0.,-1.,0.));
#6319=DIRECTION('ref_axis',(0.,0.,-1.));
#6320=DIRECTION('center_axis',(0.,-1.,0.));
#6321=DIRECTION('ref_axis',(0.,0.,-1.));
#6322=DIRECTION('',(0.,-1.,0.));
#6323=DIRECTION('center_axis',(0.,1.,0.));
#6324=DIRECTION('ref_axis',(0.,0.,-1.));
#6325=DIRECTION('center_axis',(0.,0.,1.));
#6326=DIRECTION('ref_axis',(-1.,0.,0.));
#6327=DIRECTION('',(-1.,0.,0.));
#6328=DIRECTION('',(0.,-1.,0.));
#6329=DIRECTION('',(1.,0.,0.));
#6330=DIRECTION('center_axis',(0.,-1.,0.));
#6331=DIRECTION('ref_axis',(0.,0.,1.));
#6332=DIRECTION('center_axis',(0.,-1.,0.));
#6333=DIRECTION('ref_axis',(0.,0.,1.));
#6334=DIRECTION('center_axis',(0.,1.,0.));
#6335=DIRECTION('ref_axis',(0.,0.,1.));
#6336=DIRECTION('center_axis',(0.,-1.,0.));
#6337=DIRECTION('ref_axis',(1.,0.,0.));
#6338=DIRECTION('center_axis',(0.,-1.,0.));
#6339=DIRECTION('ref_axis',(1.,0.,0.));
#6340=DIRECTION('',(0.,-1.,0.));
#6341=DIRECTION('center_axis',(0.,1.,0.));
#6342=DIRECTION('ref_axis',(1.,0.,0.));
#6343=DIRECTION('center_axis',(0.,-1.,0.));
#6344=DIRECTION('ref_axis',(1.,0.,0.));
#6345=DIRECTION('center_axis',(0.,-1.,0.));
#6346=DIRECTION('ref_axis',(1.,0.,0.));
#6347=DIRECTION('',(0.,-1.,0.));
#6348=DIRECTION('center_axis',(0.,1.,0.));
#6349=DIRECTION('ref_axis',(1.,0.,0.));
#6350=DIRECTION('center_axis',(0.,1.,0.));
#6351=DIRECTION('ref_axis',(-1.,0.,0.));
#6352=DIRECTION('',(-1.,0.,0.));
#6353=DIRECTION('',(0.,0.,1.));
#6354=DIRECTION('',(-1.,0.,0.));
#6355=DIRECTION('',(0.,0.,1.));
#6356=DIRECTION('center_axis',(1.,0.,0.));
#6357=DIRECTION('ref_axis',(0.,1.,0.));
#6358=DIRECTION('',(0.,1.,0.));
#6359=DIRECTION('',(0.,1.,0.));
#6360=DIRECTION('',(0.,0.,1.));
#6361=DIRECTION('center_axis',(0.,-1.,0.));
#6362=DIRECTION('ref_axis',(1.,0.,0.));
#6363=DIRECTION('',(1.,0.,0.));
#6364=DIRECTION('',(1.,0.,0.));
#6365=DIRECTION('',(0.,0.,1.));
#6366=DIRECTION('center_axis',(-1.,0.,0.));
#6367=DIRECTION('ref_axis',(0.,-1.,0.));
#6368=DIRECTION('',(0.,-1.,0.));
#6369=DIRECTION('',(0.,-1.,0.));
#6370=DIRECTION('center_axis',(0.,0.,1.));
#6371=DIRECTION('ref_axis',(1.,0.,0.));
#6372=DIRECTION('center_axis',(0.,0.,1.));
#6373=DIRECTION('ref_axis',(1.,0.,0.));
#6374=DIRECTION('axis',(0.,0.,1.));
#6375=DIRECTION('refdir',(1.,0.,0.));
#6376=DIRECTION('center_axis',(1.,0.,0.));
#6377=DIRECTION('ref_axis',(0.,0.,-1.));
#6378=DIRECTION('center_axis',(1.,0.,0.));
#6379=DIRECTION('ref_axis',(0.,0.,-1.));
#6380=DIRECTION('',(1.,0.,0.));
#6381=DIRECTION('center_axis',(-1.,0.,0.));
#6382=DIRECTION('ref_axis',(0.,0.,-1.));
#6383=DIRECTION('center_axis',(1.,0.,0.));
#6384=DIRECTION('ref_axis',(0.,0.,-1.));
#6385=DIRECTION('center_axis',(1.,0.,0.));
#6386=DIRECTION('ref_axis',(0.,0.,-1.));
#6387=DIRECTION('',(1.,0.,0.));
#6388=DIRECTION('center_axis',(-1.,0.,0.));
#6389=DIRECTION('ref_axis',(0.,0.,-1.));
#6390=DIRECTION('center_axis',(0.,0.,1.));
#6391=DIRECTION('ref_axis',(1.,0.,0.));
#6392=DIRECTION('',(0.,-1.,0.));
#6393=DIRECTION('center_axis',(0.,0.,1.));
#6394=DIRECTION('ref_axis',(1.,0.,0.));
#6395=DIRECTION('',(0.,1.,0.));
#6396=DIRECTION('',(1.,0.,0.));
#6397=DIRECTION('center_axis',(0.,0.,1.));
#6398=DIRECTION('ref_axis',(1.,0.,0.));
#6399=DIRECTION('',(0.,0.,1.));
#6400=DIRECTION('center_axis',(0.,0.,1.));
#6401=DIRECTION('ref_axis',(1.,0.,0.));
#6402=DIRECTION('',(0.,0.,-1.));
#6403=DIRECTION('center_axis',(0.,0.,1.));
#6404=DIRECTION('ref_axis',(1.,0.,0.));
#6405=DIRECTION('',(0.,1.,0.));
#6406=DIRECTION('',(-1.,0.,0.));
#6407=DIRECTION('',(0.,-1.,0.));
#6408=DIRECTION('center_axis',(1.,0.,0.));
#6409=DIRECTION('ref_axis',(0.,1.,0.));
#6410=DIRECTION('',(0.,0.,1.));
#6411=DIRECTION('',(0.,1.,0.));
#6412=DIRECTION('',(0.,0.,-1.));
#6413=DIRECTION('',(0.,1.,0.));
#6414=DIRECTION('',(0.,0.,1.));
#6415=DIRECTION('',(0.,1.,0.));
#6416=DIRECTION('',(0.,0.,-1.));
#6417=DIRECTION('',(0.,-1.,0.));
#6418=DIRECTION('',(0.,0.,1.));
#6419=DIRECTION('center_axis',(0.,-1.,0.));
#6420=DIRECTION('ref_axis',(1.,0.,0.));
#6421=DIRECTION('',(0.,0.,1.));
#6422=DIRECTION('',(1.,0.,0.));
#6423=DIRECTION('',(0.,0.,1.));
#6424=DIRECTION('',(1.,0.,0.));
#6425=DIRECTION('center_axis',(0.,-1.,0.));
#6426=DIRECTION('ref_axis',(1.,0.,0.));
#6427=DIRECTION('',(-1.,0.,0.));
#6428=DIRECTION('',(0.,0.,1.));
#6429=DIRECTION('',(1.,0.,0.));
#6430=DIRECTION('',(0.,0.,1.));
#6431=DIRECTION('center_axis',(0.,0.,1.));
#6432=DIRECTION('ref_axis',(1.,0.,0.));
#6433=DIRECTION('center_axis',(0.,0.,1.));
#6434=DIRECTION('ref_axis',(1.,0.,0.));
#6435=DIRECTION('',(0.,1.,0.));
#6436=DIRECTION('center_axis',(0.,0.,-1.));
#6437=DIRECTION('ref_axis',(1.,0.,0.));
#6438=DIRECTION('center_axis',(0.,0.,1.));
#6439=DIRECTION('ref_axis',(-0.25881904510252,-0.965925826289069,0.));
#6440=DIRECTION('center_axis',(0.,0.,1.));
#6441=DIRECTION('ref_axis',(1.,0.,0.));
#6442=DIRECTION('',(0.,0.,1.));
#6443=DIRECTION('center_axis',(0.,0.,1.));
#6444=DIRECTION('ref_axis',(-0.213200716355611,-0.977008420918394,0.));
#6445=DIRECTION('',(0.,0.,-1.));
#6446=DIRECTION('center_axis',(0.,0.,-1.));
#6447=DIRECTION('ref_axis',(1.,0.,0.));
#6448=DIRECTION('center_axis',(0.,0.,1.));
#6449=DIRECTION('ref_axis',(1.,0.,0.));
#6450=DIRECTION('',(-1.,0.,0.));
#6451=DIRECTION('',(0.,-1.,0.));
#6452=DIRECTION('',(0.,-1.,0.));
#6453=DIRECTION('center_axis',(-1.,0.,0.));
#6454=DIRECTION('ref_axis',(0.,-1.,0.));
#6455=DIRECTION('',(0.,0.,1.));
#6456=DIRECTION('',(0.,-1.,0.));
#6457=DIRECTION('',(0.,0.,1.));
#6458=DIRECTION('',(0.,-1.,0.));
#6459=DIRECTION('',(0.,0.,-1.));
#6460=DIRECTION('',(0.,-1.,0.));
#6461=DIRECTION('center_axis',(0.,0.,1.));
#6462=DIRECTION('ref_axis',(-0.213200716355611,-0.977008420918394,0.));
#6463=DIRECTION('center_axis',(0.,0.,-1.));
#6464=DIRECTION('ref_axis',(1.,0.,0.));
#6465=DIRECTION('center_axis',(0.,0.,-1.));
#6466=DIRECTION('ref_axis',(1.,0.,0.));
#6467=DIRECTION('center_axis',(0.,0.,1.));
#6468=DIRECTION('ref_axis',(-0.25881904510252,-0.965925826289069,0.));
#6469=DIRECTION('center_axis',(0.,0.,1.));
#6470=DIRECTION('ref_axis',(1.,0.,0.));
#6471=DIRECTION('center_axis',(0.,0.,1.));
#6472=DIRECTION('ref_axis',(1.,0.,0.));
#6473=DIRECTION('center_axis',(0.,0.,1.));
#6474=DIRECTION('ref_axis',(1.,0.,0.));
#6475=DIRECTION('center_axis',(0.,1.,0.));
#6476=DIRECTION('ref_axis',(-1.,0.,0.));
#6477=DIRECTION('',(-1.,0.,0.));
#6478=DIRECTION('center_axis',(0.,0.,1.));
#6479=DIRECTION('ref_axis',(1.,0.,0.));
#6480=DIRECTION('axis',(0.,0.,1.));
#6481=DIRECTION('refdir',(1.,0.,0.));
#6482=DIRECTION('center_axis',(0.,-1.,0.));
#6483=DIRECTION('ref_axis',(1.,0.,0.));
#6484=DIRECTION('center_axis',(0.,-1.,0.));
#6485=DIRECTION('ref_axis',(1.,0.,0.));
#6486=DIRECTION('',(0.,-1.,0.));
#6487=DIRECTION('center_axis',(0.,1.,0.));
#6488=DIRECTION('ref_axis',(1.,0.,0.));
#6489=DIRECTION('center_axis',(0.,-1.,0.));
#6490=DIRECTION('ref_axis',(1.,0.,0.));
#6491=DIRECTION('center_axis',(0.,-1.,0.));
#6492=DIRECTION('ref_axis',(1.,0.,0.));
#6493=DIRECTION('',(0.,-1.,0.));
#6494=DIRECTION('center_axis',(0.,1.,0.));
#6495=DIRECTION('ref_axis',(1.,0.,0.));
#6496=DIRECTION('center_axis',(0.,0.,1.));
#6497=DIRECTION('ref_axis',(1.,0.,0.));
#6498=DIRECTION('',(-1.,0.,0.));
#6499=DIRECTION('center_axis',(0.,0.,1.));
#6500=DIRECTION('ref_axis',(1.,0.,0.));
#6501=DIRECTION('',(0.,1.,0.));
#6502=DIRECTION('center_axis',(0.,0.,1.));
#6503=DIRECTION('ref_axis',(1.,0.,0.));
#6504=DIRECTION('',(0.,0.,-1.));
#6505=DIRECTION('center_axis',(0.,0.,-1.));
#6506=DIRECTION('ref_axis',(1.,0.,0.));
#6507=DIRECTION('',(0.,0.,1.));
#6508=DIRECTION('center_axis',(0.,-1.,0.));
#6509=DIRECTION('ref_axis',(1.,0.,0.));
#6510=DIRECTION('',(0.,0.,1.));
#6511=DIRECTION('',(1.,0.,0.));
#6512=DIRECTION('',(0.,0.,-1.));
#6513=DIRECTION('',(-1.,0.,0.));
#6514=DIRECTION('',(0.,0.,1.));
#6515=DIRECTION('',(1.,0.,0.));
#6516=DIRECTION('',(0.,0.,-1.));
#6517=DIRECTION('',(1.,0.,0.));
#6518=DIRECTION('',(0.,0.,1.));
#6519=DIRECTION('',(1.,0.,0.));
#6520=DIRECTION('center_axis',(-1.,0.,0.));
#6521=DIRECTION('ref_axis',(0.,-1.,0.));
#6522=DIRECTION('',(0.,-1.,0.));
#6523=DIRECTION('',(0.,0.,1.));
#6524=DIRECTION('',(0.,-1.,0.));
#6525=DIRECTION('',(0.,0.,1.));
#6526=DIRECTION('',(0.,-1.,0.));
#6527=DIRECTION('',(0.,1.,0.));
#6528=DIRECTION('',(0.,0.,1.));
#6529=DIRECTION('',(0.,-1.,0.));
#6530=DIRECTION('center_axis',(0.,0.,1.));
#6531=DIRECTION('ref_axis',(1.,0.,0.));
#6532=DIRECTION('center_axis',(0.,0.,1.));
#6533=DIRECTION('ref_axis',(1.,0.,0.));
#6534=DIRECTION('center_axis',(0.,0.,1.));
#6535=DIRECTION('ref_axis',(1.,0.,0.));
#6536=DIRECTION('center_axis',(0.,0.,1.));
#6537=DIRECTION('ref_axis',(1.,0.,0.));
#6538=DIRECTION('center_axis',(0.,0.,1.));
#6539=DIRECTION('ref_axis',(1.,0.,0.));
#6540=DIRECTION('',(-1.,0.,0.));
#6541=DIRECTION('',(0.,1.,0.));
#6542=DIRECTION('center_axis',(0.,0.,1.));
#6543=DIRECTION('ref_axis',(1.,0.,0.));
#6544=DIRECTION('center_axis',(0.,0.,1.));
#6545=DIRECTION('ref_axis',(1.,0.,0.));
#6546=DIRECTION('center_axis',(0.,0.,-1.));
#6547=DIRECTION('ref_axis',(1.,0.,0.));
#6548=DIRECTION('center_axis',(0.,0.,1.));
#6549=DIRECTION('ref_axis',(1.,0.,0.));
#6550=DIRECTION('center_axis',(0.,0.,-1.));
#6551=DIRECTION('ref_axis',(1.,0.,0.));
#6552=DIRECTION('',(0.,0.,1.));
#6553=DIRECTION('center_axis',(0.,0.,1.));
#6554=DIRECTION('ref_axis',(-0.758601839724033,-0.651554486414845,0.));
#6555=DIRECTION('center_axis',(0.,0.,1.));
#6556=DIRECTION('ref_axis',(1.,0.,0.));
#6557=DIRECTION('center_axis',(0.,0.,1.));
#6558=DIRECTION('ref_axis',(1.,0.,0.));
#6559=DIRECTION('center_axis',(0.,1.,0.));
#6560=DIRECTION('ref_axis',(-1.,0.,0.));
#6561=DIRECTION('',(-1.,0.,0.));
#6562=DIRECTION('',(0.,0.,1.));
#6563=DIRECTION('center_axis',(1.,0.,0.));
#6564=DIRECTION('ref_axis',(0.,1.,0.));
#6565=DIRECTION('',(0.,1.,0.));
#6566=DIRECTION('center_axis',(0.,0.,1.));
#6567=DIRECTION('ref_axis',(1.,0.,0.));
#6568=DIRECTION('axis',(0.,0.,1.));
#6569=DIRECTION('refdir',(1.,0.,0.));
#6570=DIRECTION('center_axis',(0.,0.,1.));
#6571=DIRECTION('ref_axis',(1.,0.,0.));
#6572=DIRECTION('center_axis',(0.,0.,1.));
#6573=DIRECTION('ref_axis',(1.,0.,0.));
#6574=DIRECTION('center_axis',(0.,0.,-1.));
#6575=DIRECTION('ref_axis',(1.,0.,0.));
#6576=DIRECTION('center_axis',(0.,0.,1.));
#6577=DIRECTION('ref_axis',(1.,0.,0.));
#6578=DIRECTION('center_axis',(0.,0.,1.));
#6579=DIRECTION('ref_axis',(1.,0.,0.));
#6580=DIRECTION('',(0.,0.,-1.));
#6581=DIRECTION('center_axis',(0.,0.,1.));
#6582=DIRECTION('ref_axis',(1.,0.,0.));
#6583=DIRECTION('center_axis',(0.,0.,1.));
#6584=DIRECTION('ref_axis',(1.,0.,0.));
#6585=DIRECTION('center_axis',(0.,0.,1.));
#6586=DIRECTION('ref_axis',(1.,0.,0.));
#6587=DIRECTION('center_axis',(0.,0.,1.));
#6588=DIRECTION('ref_axis',(1.,0.,0.));
#6589=DIRECTION('',(0.,0.,-1.));
#6590=DIRECTION('center_axis',(0.,0.,1.));
#6591=DIRECTION('ref_axis',(1.,0.,0.));
#6592=DIRECTION('center_axis',(0.,0.,1.));
#6593=DIRECTION('ref_axis',(1.,0.,0.));
#6594=DIRECTION('center_axis',(0.,0.,1.));
#6595=DIRECTION('ref_axis',(1.,0.,0.));
#6596=DIRECTION('',(0.,0.,-1.));
#6597=DIRECTION('center_axis',(0.,0.,1.));
#6598=DIRECTION('ref_axis',(1.,0.,0.));
#6599=DIRECTION('axis',(0.,0.,1.));
#6600=DIRECTION('refdir',(1.,0.,0.));
#6601=DIRECTION('center_axis',(0.,1.,0.));
#6602=DIRECTION('ref_axis',(-1.,0.,0.));
#6603=DIRECTION('',(-1.,0.,0.));
#6604=DIRECTION('',(0.,0.,1.));
#6605=DIRECTION('',(-1.,0.,0.));
#6606=DIRECTION('',(0.,0.,1.));
#6607=DIRECTION('center_axis',(1.,0.,0.));
#6608=DIRECTION('ref_axis',(0.,1.,0.));
#6609=DIRECTION('',(0.,1.,0.));
#6610=DIRECTION('',(0.,1.,0.));
#6611=DIRECTION('',(0.,0.,1.));
#6612=DIRECTION('center_axis',(0.,-1.,0.));
#6613=DIRECTION('ref_axis',(1.,0.,0.));
#6614=DIRECTION('',(1.,0.,0.));
#6615=DIRECTION('',(1.,0.,0.));
#6616=DIRECTION('',(0.,0.,1.));
#6617=DIRECTION('center_axis',(-1.,0.,0.));
#6618=DIRECTION('ref_axis',(0.,-1.,0.));
#6619=DIRECTION('',(0.,-1.,0.));
#6620=DIRECTION('',(0.,-1.,0.));
#6621=DIRECTION('center_axis',(0.,0.,1.));
#6622=DIRECTION('ref_axis',(1.,0.,0.));
#6623=DIRECTION('center_axis',(0.,0.,1.));
#6624=DIRECTION('ref_axis',(1.,0.,0.));
#6625=DIRECTION('axis',(0.,0.,1.));
#6626=DIRECTION('refdir',(1.,0.,0.));
#6627=DIRECTION('center_axis',(1.,0.,0.));
#6628=DIRECTION('ref_axis',(0.,0.,-1.));
#6629=DIRECTION('center_axis',(1.,0.,0.));
#6630=DIRECTION('ref_axis',(0.,0.,-1.));
#6631=DIRECTION('',(1.,0.,0.));
#6632=DIRECTION('center_axis',(1.,0.,0.));
#6633=DIRECTION('ref_axis',(0.,0.,-1.));
#6634=DIRECTION('center_axis',(1.,0.,0.));
#6635=DIRECTION('ref_axis',(0.,0.,-1.));
#6636=DIRECTION('center_axis',(1.,0.,0.));
#6637=DIRECTION('ref_axis',(0.,0.,-1.));
#6638=DIRECTION('center_axis',(1.,0.,0.));
#6639=DIRECTION('ref_axis',(0.,0.,-1.));
#6640=DIRECTION('',(1.,0.,0.));
#6641=DIRECTION('center_axis',(1.,0.,0.));
#6642=DIRECTION('ref_axis',(0.,0.,-1.));
#6643=DIRECTION('center_axis',(1.,0.,0.));
#6644=DIRECTION('ref_axis',(0.,0.,-1.));
#6645=DIRECTION('center_axis',(1.,0.,0.));
#6646=DIRECTION('ref_axis',(0.,0.,-1.));
#6647=DIRECTION('center_axis',(1.,0.,0.));
#6648=DIRECTION('ref_axis',(0.,0.,-1.));
#6649=DIRECTION('',(1.,0.,0.));
#6650=DIRECTION('center_axis',(1.,0.,0.));
#6651=DIRECTION('ref_axis',(0.,0.,-1.));
#6652=DIRECTION('center_axis',(1.,0.,0.));
#6653=DIRECTION('ref_axis',(0.,0.,-1.));
#6654=DIRECTION('center_axis',(1.,0.,0.));
#6655=DIRECTION('ref_axis',(0.,0.,-1.));
#6656=DIRECTION('center_axis',(1.,0.,0.));
#6657=DIRECTION('ref_axis',(0.,0.,-1.));
#6658=DIRECTION('',(1.,0.,0.));
#6659=DIRECTION('center_axis',(1.,0.,0.));
#6660=DIRECTION('ref_axis',(0.,0.,-1.));
#6661=DIRECTION('center_axis',(1.,0.,0.));
#6662=DIRECTION('ref_axis',(0.,0.,-1.));
#6663=DIRECTION('center_axis',(-1.,0.,0.));
#6664=DIRECTION('ref_axis',(0.,0.,-1.));
#6665=DIRECTION('center_axis',(-1.,0.,0.));
#6666=DIRECTION('ref_axis',(0.,0.,-1.));
#6667=DIRECTION('',(-1.,0.,0.));
#6668=DIRECTION('center_axis',(1.,0.,0.));
#6669=DIRECTION('ref_axis',(0.,0.,-1.));
#6670=DIRECTION('center_axis',(-1.,0.,0.));
#6671=DIRECTION('ref_axis',(0.,0.,-1.));
#6672=DIRECTION('center_axis',(-1.,0.,0.));
#6673=DIRECTION('ref_axis',(0.,0.,-1.));
#6674=DIRECTION('',(-1.,0.,0.));
#6675=DIRECTION('center_axis',(1.,0.,0.));
#6676=DIRECTION('ref_axis',(0.,0.,-1.));
#6677=DIRECTION('center_axis',(0.,1.,0.));
#6678=DIRECTION('ref_axis',(-1.,0.,0.));
#6679=DIRECTION('',(1.,0.,0.));
#6680=DIRECTION('',(0.,0.,1.));
#6681=DIRECTION('',(-1.,0.,0.));
#6682=DIRECTION('',(0.,0.,-1.));
#6683=DIRECTION('center_axis',(0.,1.,0.));
#6684=DIRECTION('ref_axis',(-1.,0.,0.));
#6685=DIRECTION('',(1.,0.,0.));
#6686=DIRECTION('',(0.,0.,1.));
#6687=DIRECTION('',(-1.,0.,0.));
#6688=DIRECTION('',(0.,0.,-1.));
#6689=DIRECTION('center_axis',(0.,1.,0.));
#6690=DIRECTION('ref_axis',(-1.,0.,0.));
#6691=DIRECTION('',(1.,0.,0.));
#6692=DIRECTION('',(0.,0.,1.));
#6693=DIRECTION('',(-1.,0.,0.));
#6694=DIRECTION('',(0.,0.,-1.));
#6695=DIRECTION('center_axis',(0.,1.,0.));
#6696=DIRECTION('ref_axis',(-1.,0.,0.));
#6697=DIRECTION('',(1.,0.,0.));
#6698=DIRECTION('',(0.,0.,1.));
#6699=DIRECTION('',(-1.,0.,0.));
#6700=DIRECTION('',(0.,0.,-1.));
#6701=DIRECTION('center_axis',(0.,-1.,0.));
#6702=DIRECTION('ref_axis',(1.,0.,0.));
#6703=DIRECTION('',(-1.,0.,0.));
#6704=DIRECTION('',(0.,0.,1.));
#6705=DIRECTION('',(1.,0.,0.));
#6706=DIRECTION('',(0.,0.,1.));
#6707=DIRECTION('center_axis',(0.,-1.,0.));
#6708=DIRECTION('ref_axis',(1.,0.,0.));
#6709=DIRECTION('',(-1.,0.,0.));
#6710=DIRECTION('',(0.,0.,1.));
#6711=DIRECTION('',(1.,0.,0.));
#6712=DIRECTION('',(0.,0.,1.));
#6713=DIRECTION('center_axis',(0.,-1.,0.));
#6714=DIRECTION('ref_axis',(1.,0.,0.));
#6715=DIRECTION('',(-1.,0.,0.));
#6716=DIRECTION('',(0.,0.,1.));
#6717=DIRECTION('',(1.,0.,0.));
#6718=DIRECTION('',(0.,0.,1.));
#6719=DIRECTION('center_axis',(0.,-1.,0.));
#6720=DIRECTION('ref_axis',(1.,0.,0.));
#6721=DIRECTION('',(-1.,0.,0.));
#6722=DIRECTION('',(0.,0.,1.));
#6723=DIRECTION('',(1.,0.,0.));
#6724=DIRECTION('',(0.,0.,1.));
#6725=DIRECTION('center_axis',(-1.,0.,0.));
#6726=DIRECTION('ref_axis',(0.,-1.,0.));
#6727=DIRECTION('',(0.,-1.,0.));
#6728=DIRECTION('',(0.,0.,-1.));
#6729=DIRECTION('',(0.,1.,0.));
#6730=DIRECTION('',(0.,0.,1.));
#6731=DIRECTION('',(0.,-1.,0.));
#6732=DIRECTION('',(0.,-1.,0.));
#6733=DIRECTION('',(0.,0.,1.));
#6734=DIRECTION('',(0.,-1.,0.));
#6735=DIRECTION('',(0.,-1.,0.));
#6736=DIRECTION('',(0.,0.,1.));
#6737=DIRECTION('',(0.,-1.,0.));
#6738=DIRECTION('',(0.,-1.,0.));
#6739=DIRECTION('',(0.,0.,1.));
#6740=DIRECTION('',(0.,-1.,0.));
#6741=DIRECTION('',(0.,-1.,0.));
#6742=DIRECTION('',(0.,0.,1.));
#6743=DIRECTION('',(0.,-1.,0.));
#6744=DIRECTION('',(0.,0.,-1.));
#6745=DIRECTION('',(0.,-1.,0.));
#6746=DIRECTION('',(0.,-1.,0.));
#6747=DIRECTION('',(0.,0.,-1.));
#6748=DIRECTION('',(0.,-1.,0.));
#6749=DIRECTION('',(0.,-1.,0.));
#6750=DIRECTION('',(0.,0.,-1.));
#6751=DIRECTION('',(0.,-1.,0.));
#6752=DIRECTION('',(0.,-1.,0.));
#6753=DIRECTION('',(0.,0.,-1.));
#6754=DIRECTION('',(0.,-1.,0.));
#6755=DIRECTION('center_axis',(0.,0.,1.));
#6756=DIRECTION('ref_axis',(1.,0.,0.));
#6757=DIRECTION('',(-1.,0.,0.));
#6758=DIRECTION('',(0.,-1.,0.));
#6759=DIRECTION('center_axis',(0.,0.,1.));
#6760=DIRECTION('ref_axis',(1.,0.,0.));
#6761=DIRECTION('',(0.,-1.,0.));
#6762=DIRECTION('',(1.,0.,0.));
#6763=DIRECTION('center_axis',(1.,0.,0.));
#6764=DIRECTION('ref_axis',(0.,1.,0.));
#6765=DIRECTION('',(0.,0.,1.));
#6766=DIRECTION('',(0.,1.,0.));
#6767=DIRECTION('center_axis',(1.,0.,0.));
#6768=DIRECTION('ref_axis',(0.,1.,0.));
#6769=DIRECTION('',(0.,1.,0.));
#6770=DIRECTION('',(0.,0.,1.));
#6771=DIRECTION('center_axis',(0.,0.,1.));
#6772=DIRECTION('ref_axis',(1.,0.,0.));
#6773=DIRECTION('',(1.,0.,0.));
#6774=DIRECTION('center_axis',(0.,0.,1.));
#6775=DIRECTION('ref_axis',(1.,0.,0.));
#6776=DIRECTION('',(-1.,0.,0.));
#6777=DIRECTION('center_axis',(0.,0.,1.));
#6778=DIRECTION('ref_axis',(1.,0.,0.));
#6779=DIRECTION('',(-1.,0.,0.));
#6780=DIRECTION('',(0.,-1.,0.));
#6781=DIRECTION('center_axis',(0.,0.,1.));
#6782=DIRECTION('ref_axis',(1.,0.,0.));
#6783=DIRECTION('',(0.,-1.,0.));
#6784=DIRECTION('',(1.,0.,0.));
#6785=DIRECTION('center_axis',(1.,0.,0.));
#6786=DIRECTION('ref_axis',(0.,1.,0.));
#6787=DIRECTION('',(0.,0.,1.));
#6788=DIRECTION('',(0.,1.,0.));
#6789=DIRECTION('center_axis',(1.,0.,0.));
#6790=DIRECTION('ref_axis',(0.,1.,0.));
#6791=DIRECTION('',(0.,1.,0.));
#6792=DIRECTION('',(0.,0.,1.));
#6793=DIRECTION('center_axis',(0.,0.,1.));
#6794=DIRECTION('ref_axis',(1.,0.,0.));
#6795=DIRECTION('',(1.,0.,0.));
#6796=DIRECTION('center_axis',(0.,0.,1.));
#6797=DIRECTION('ref_axis',(1.,0.,0.));
#6798=DIRECTION('',(-1.,0.,0.));
#6799=DIRECTION('center_axis',(0.,0.,1.));
#6800=DIRECTION('ref_axis',(1.,0.,0.));
#6801=DIRECTION('',(-1.,0.,0.));
#6802=DIRECTION('',(0.,-1.,0.));
#6803=DIRECTION('center_axis',(0.,0.,1.));
#6804=DIRECTION('ref_axis',(1.,0.,0.));
#6805=DIRECTION('',(0.,-1.,0.));
#6806=DIRECTION('',(1.,0.,0.));
#6807=DIRECTION('center_axis',(1.,0.,0.));
#6808=DIRECTION('ref_axis',(0.,1.,0.));
#6809=DIRECTION('',(0.,0.,1.));
#6810=DIRECTION('',(0.,1.,0.));
#6811=DIRECTION('center_axis',(1.,0.,0.));
#6812=DIRECTION('ref_axis',(0.,1.,0.));
#6813=DIRECTION('',(0.,1.,0.));
#6814=DIRECTION('',(0.,0.,1.));
#6815=DIRECTION('center_axis',(0.,0.,1.));
#6816=DIRECTION('ref_axis',(1.,0.,0.));
#6817=DIRECTION('',(1.,0.,0.));
#6818=DIRECTION('center_axis',(0.,0.,1.));
#6819=DIRECTION('ref_axis',(1.,0.,0.));
#6820=DIRECTION('',(-1.,0.,0.));
#6821=DIRECTION('center_axis',(0.,0.,1.));
#6822=DIRECTION('ref_axis',(1.,0.,0.));
#6823=DIRECTION('',(-1.,0.,0.));
#6824=DIRECTION('',(0.,-1.,0.));
#6825=DIRECTION('center_axis',(0.,0.,1.));
#6826=DIRECTION('ref_axis',(1.,0.,0.));
#6827=DIRECTION('',(0.,-1.,0.));
#6828=DIRECTION('',(1.,0.,0.));
#6829=DIRECTION('center_axis',(1.,0.,0.));
#6830=DIRECTION('ref_axis',(0.,1.,0.));
#6831=DIRECTION('',(0.,0.,1.));
#6832=DIRECTION('',(0.,1.,0.));
#6833=DIRECTION('center_axis',(1.,0.,0.));
#6834=DIRECTION('ref_axis',(0.,1.,0.));
#6835=DIRECTION('',(0.,1.,0.));
#6836=DIRECTION('',(0.,0.,1.));
#6837=DIRECTION('center_axis',(0.,0.,1.));
#6838=DIRECTION('ref_axis',(1.,0.,0.));
#6839=DIRECTION('',(1.,0.,0.));
#6840=DIRECTION('center_axis',(0.,0.,1.));
#6841=DIRECTION('ref_axis',(1.,0.,0.));
#6842=DIRECTION('',(-1.,0.,0.));
#6843=DIRECTION('center_axis',(0.,1.,0.));
#6844=DIRECTION('ref_axis',(-1.,0.,0.));
#6845=DIRECTION('',(-1.,0.,0.));
#6846=DIRECTION('',(0.,0.,1.));
#6847=DIRECTION('',(-1.,0.,0.));
#6848=DIRECTION('center_axis',(0.,0.,1.));
#6849=DIRECTION('ref_axis',(1.,0.,0.));
#6850=DIRECTION('',(1.,0.,0.));
#6851=DIRECTION('',(0.,-1.,0.));
#6852=DIRECTION('center_axis',(0.,-1.,0.));
#6853=DIRECTION('ref_axis',(1.,0.,0.));
#6854=DIRECTION('',(1.,0.,0.));
#6855=DIRECTION('',(0.,0.,1.));
#6856=DIRECTION('center_axis',(-1.,0.,0.));
#6857=DIRECTION('ref_axis',(0.,-1.,0.));
#6858=DIRECTION('',(0.,-1.,0.));
#6859=DIRECTION('center_axis',(0.,0.,1.));
#6860=DIRECTION('ref_axis',(1.,0.,0.));
#6861=DIRECTION('axis',(0.,0.,1.));
#6862=DIRECTION('refdir',(1.,0.,0.));
#6863=DIRECTION('center_axis',(0.,-1.,0.));
#6864=DIRECTION('ref_axis',(1.,0.,0.));
#6865=DIRECTION('',(-1.,0.,0.));
#6866=DIRECTION('',(0.,0.,1.));
#6867=DIRECTION('',(1.,0.,0.));
#6868=DIRECTION('',(0.,0.,-1.));
#6869=DIRECTION('center_axis',(0.,1.,0.));
#6870=DIRECTION('ref_axis',(-1.,0.,0.));
#6871=DIRECTION('',(1.,0.,0.));
#6872=DIRECTION('',(0.,0.,1.));
#6873=DIRECTION('',(-1.,0.,0.));
#6874=DIRECTION('',(0.,0.,-1.));
#6875=DIRECTION('center_axis',(0.,0.,1.));
#6876=DIRECTION('ref_axis',(1.,0.,0.));
#6877=DIRECTION('',(0.,1.,0.));
#6878=DIRECTION('',(0.,-1.,0.));
#6879=DIRECTION('center_axis',(1.,0.,0.));
#6880=DIRECTION('ref_axis',(0.,1.,0.));
#6881=DIRECTION('',(0.,1.,0.));
#6882=DIRECTION('',(0.,0.,1.));
#6883=DIRECTION('',(0.,1.,0.));
#6884=DIRECTION('',(0.,0.,1.));
#6885=DIRECTION('',(0.,1.,0.));
#6886=DIRECTION('center_axis',(0.,0.,1.));
#6887=DIRECTION('ref_axis',(1.,0.,0.));
#6888=DIRECTION('',(0.,-1.,0.));
#6889=DIRECTION('',(1.,0.,0.));
#6890=DIRECTION('center_axis',(0.,1.,0.));
#6891=DIRECTION('ref_axis',(-1.,0.,0.));
#6892=DIRECTION('',(-1.,0.,0.));
#6893=DIRECTION('',(0.,0.,1.));
#6894=DIRECTION('',(-1.,0.,0.));
#6895=DIRECTION('center_axis',(0.,-1.,0.));
#6896=DIRECTION('ref_axis',(1.,0.,0.));
#6897=DIRECTION('',(1.,0.,0.));
#6898=DIRECTION('',(0.,0.,1.));
#6899=DIRECTION('center_axis',(-1.,0.,0.));
#6900=DIRECTION('ref_axis',(0.,-1.,0.));
#6901=DIRECTION('',(0.,-1.,0.));
#6902=DIRECTION('',(0.,-1.,0.));
#6903=DIRECTION('center_axis',(0.,0.,1.));
#6904=DIRECTION('ref_axis',(1.,0.,0.));
#6905=DIRECTION('center_axis',(0.,0.,1.));
#6906=DIRECTION('ref_axis',(1.,0.,0.));
#6907=DIRECTION('axis',(0.,0.,1.));
#6908=DIRECTION('refdir',(1.,0.,0.));
#6909=DIRECTION('center_axis',(0.,1.,0.));
#6910=DIRECTION('ref_axis',(-1.,0.,0.));
#6911=DIRECTION('',(-1.,0.,0.));
#6912=DIRECTION('',(0.,0.,1.));
#6913=DIRECTION('',(1.,0.,0.));
#6914=DIRECTION('',(0.,0.,1.));
#6915=DIRECTION('center_axis',(1.,0.,0.));
#6916=DIRECTION('ref_axis',(0.,1.,0.));
#6917=DIRECTION('',(0.,1.,0.));
#6918=DIRECTION('',(0.,0.,-1.));
#6919=DIRECTION('',(0.,-1.,0.));
#6920=DIRECTION('center_axis',(-1.,0.,0.));
#6921=DIRECTION('ref_axis',(0.,-1.,0.));
#6922=DIRECTION('',(0.,-1.,0.));
#6923=DIRECTION('',(0.,0.,1.));
#6924=DIRECTION('',(0.,-1.,0.));
#6925=DIRECTION('center_axis',(0.,-1.,0.));
#6926=DIRECTION('ref_axis',(1.,0.,0.));
#6927=DIRECTION('',(1.,0.,0.));
#6928=DIRECTION('',(0.,0.,1.));
#6929=DIRECTION('',(1.,0.,0.));
#6930=DIRECTION('center_axis',(0.,1.,0.));
#6931=DIRECTION('ref_axis',(-1.,0.,0.));
#6932=DIRECTION('',(-1.,0.,0.));
#6933=DIRECTION('',(-1.,0.,0.));
#6934=DIRECTION('',(0.,0.,1.));
#6935=DIRECTION('center_axis',(1.,0.,0.));
#6936=DIRECTION('ref_axis',(0.,1.,0.));
#6937=DIRECTION('',(0.,1.,0.));
#6938=DIRECTION('',(0.,1.,0.));
#6939=DIRECTION('center_axis',(0.,0.,1.));
#6940=DIRECTION('ref_axis',(1.,0.,0.));
#6941=DIRECTION('center_axis',(0.,0.,1.));
#6942=DIRECTION('ref_axis',(1.,0.,0.));
#6943=DIRECTION('axis',(0.,0.,1.));
#6944=DIRECTION('refdir',(1.,0.,0.));
#6945=DIRECTION('center_axis',(0.,0.,1.));
#6946=DIRECTION('ref_axis',(0.409441503265782,-0.912336371851663,0.));
#6947=DIRECTION('',(0.,0.,-1.));
#6948=DIRECTION('center_axis',(0.,0.,-1.));
#6949=DIRECTION('ref_axis',(1.,-2.80853466614331E-13,0.));
#6950=DIRECTION('center_axis',(0.,0.,1.));
#6951=DIRECTION('ref_axis',(0.409441503265782,-0.912336371851663,0.));
#6952=DIRECTION('',(0.,0.,-1.));
#6953=DIRECTION('center_axis',(0.,0.,1.));
#6954=DIRECTION('ref_axis',(0.409441503265782,-0.912336371851663,0.));
#6955=DIRECTION('',(0.,0.,-1.));
#6956=DIRECTION('center_axis',(0.,0.,1.));
#6957=DIRECTION('ref_axis',(0.409441503265782,-0.912336371851663,0.));
#6958=DIRECTION('',(0.,0.,-1.));
#6959=DIRECTION('center_axis',(0.,0.,1.));
#6960=DIRECTION('ref_axis',(0.409441503265782,-0.912336371851663,0.));
#6961=DIRECTION('',(0.,0.,-1.));
#6962=DIRECTION('center_axis',(0.,0.,1.));
#6963=DIRECTION('ref_axis',(0.409441503265782,-0.912336371851663,0.));
#6964=DIRECTION('',(0.,0.,-1.));
#6965=DIRECTION('center_axis',(0.,0.,1.));
#6966=DIRECTION('ref_axis',(0.409441503265782,-0.912336371851663,0.));
#6967=DIRECTION('',(0.,0.,-1.));
#6968=DIRECTION('center_axis',(0.,0.,1.));
#6969=DIRECTION('ref_axis',(0.409441503265782,-0.912336371851663,0.));
#6970=DIRECTION('',(0.,0.,-1.));
#6971=DIRECTION('center_axis',(0.,0.,1.));
#6972=DIRECTION('ref_axis',(0.409441503265782,-0.912336371851663,0.));
#6973=DIRECTION('',(0.,0.,-1.));
#6974=DIRECTION('center_axis',(0.,0.,1.));
#6975=DIRECTION('ref_axis',(0.409441503265782,-0.912336371851663,0.));
#6976=DIRECTION('',(0.,0.,-1.));
#6977=DIRECTION('center_axis',(0.,0.,1.));
#6978=DIRECTION('ref_axis',(0.409441503265782,-0.912336371851663,0.));
#6979=DIRECTION('',(0.,0.,-1.));
#6980=DIRECTION('center_axis',(0.,0.,1.));
#6981=DIRECTION('ref_axis',(0.409441503265782,-0.912336371851663,0.));
#6982=DIRECTION('',(0.,0.,-1.));
#6983=DIRECTION('center_axis',(0.,0.,1.));
#6984=DIRECTION('ref_axis',(0.409441503265782,-0.912336371851663,0.));
#6985=DIRECTION('',(0.,0.,-1.));
#6986=DIRECTION('center_axis',(0.,0.,1.));
#6987=DIRECTION('ref_axis',(0.409441503265782,-0.912336371851663,0.));
#6988=DIRECTION('',(0.,0.,-1.));
#6989=DIRECTION('center_axis',(0.,0.,1.));
#6990=DIRECTION('ref_axis',(0.409441503265782,-0.912336371851663,0.));
#6991=DIRECTION('',(0.,0.,-1.));
#6992=DIRECTION('center_axis',(0.,0.,1.));
#6993=DIRECTION('ref_axis',(0.409441503265782,-0.912336371851663,0.));
#6994=DIRECTION('',(0.,0.,-1.));
#6995=DIRECTION('center_axis',(0.,0.,1.));
#6996=DIRECTION('ref_axis',(0.409441503265782,-0.912336371851663,0.));
#6997=DIRECTION('',(0.,0.,-1.));
#6998=DIRECTION('center_axis',(0.,0.,1.));
#6999=DIRECTION('ref_axis',(0.409441503265782,-0.912336371851663,0.));
#7000=DIRECTION('',(0.,0.,-1.));
#7001=DIRECTION('center_axis',(0.,0.,1.));
#7002=DIRECTION('ref_axis',(0.409441503265782,-0.912336371851663,0.));
#7003=DIRECTION('',(0.,0.,-1.));
#7004=DIRECTION('center_axis',(0.,0.,1.));
#7005=DIRECTION('ref_axis',(0.409441503265782,-0.912336371851663,0.));
#7006=DIRECTION('',(0.,0.,-1.));
#7007=DIRECTION('center_axis',(0.,0.,1.));
#7008=DIRECTION('ref_axis',(0.409441503265782,-0.912336371851663,0.));
#7009=DIRECTION('',(0.,0.,-1.));
#7010=DIRECTION('center_axis',(0.,0.,1.));
#7011=DIRECTION('ref_axis',(0.409441503265782,-0.912336371851663,0.));
#7012=DIRECTION('',(0.,0.,-1.));
#7013=DIRECTION('center_axis',(0.,0.,1.));
#7014=DIRECTION('ref_axis',(0.409441503265782,-0.912336371851663,0.));
#7015=DIRECTION('',(0.,0.,-1.));
#7016=DIRECTION('center_axis',(0.,0.,1.));
#7017=DIRECTION('ref_axis',(0.409441503265782,-0.912336371851663,0.));
#7018=DIRECTION('',(0.,0.,-1.));
#7019=DIRECTION('center_axis',(0.,0.,1.));
#7020=DIRECTION('ref_axis',(0.409441503265782,-0.912336371851663,0.));
#7021=DIRECTION('',(0.,0.,-1.));
#7022=DIRECTION('center_axis',(0.,0.,1.));
#7023=DIRECTION('ref_axis',(0.409441503265782,-0.912336371851663,0.));
#7024=DIRECTION('',(0.,0.,-1.));
#7025=DIRECTION('center_axis',(0.,0.,1.));
#7026=DIRECTION('ref_axis',(0.409441503265782,-0.912336371851663,0.));
#7027=DIRECTION('',(0.,0.,-1.));
#7028=DIRECTION('center_axis',(0.,0.,1.));
#7029=DIRECTION('ref_axis',(0.409441503265782,-0.912336371851663,0.));
#7030=DIRECTION('',(0.,0.,-1.));
#7031=DIRECTION('center_axis',(0.,0.,1.));
#7032=DIRECTION('ref_axis',(0.409441503265782,-0.912336371851663,0.));
#7033=DIRECTION('',(0.,0.,-1.));
#7034=DIRECTION('center_axis',(0.,0.,1.));
#7035=DIRECTION('ref_axis',(0.409441503265782,-0.912336371851663,0.));
#7036=DIRECTION('',(0.,0.,-1.));
#7037=DIRECTION('center_axis',(0.,0.,1.));
#7038=DIRECTION('ref_axis',(0.409441503265782,-0.912336371851663,0.));
#7039=DIRECTION('',(0.,0.,-1.));
#7040=DIRECTION('center_axis',(0.,0.,1.));
#7041=DIRECTION('ref_axis',(0.409441503265782,-0.912336371851663,0.));
#7042=DIRECTION('',(0.,0.,-1.));
#7043=DIRECTION('center_axis',(0.,0.,1.));
#7044=DIRECTION('ref_axis',(0.409441503265782,-0.912336371851663,0.));
#7045=DIRECTION('',(0.,0.,-1.));
#7046=DIRECTION('center_axis',(0.,0.,1.));
#7047=DIRECTION('ref_axis',(0.409441503265782,-0.912336371851663,0.));
#7048=DIRECTION('',(0.,0.,-1.));
#7049=DIRECTION('center_axis',(0.,0.,1.));
#7050=DIRECTION('ref_axis',(1.,0.,0.));
#7051=DIRECTION('center_axis',(0.,0.,-1.));
#7052=DIRECTION('ref_axis',(1.,0.,0.));
#7053=DIRECTION('center_axis',(0.,0.,-1.));
#7054=DIRECTION('ref_axis',(1.,0.,0.));
#7055=DIRECTION('center_axis',(0.,0.,1.));
#7056=DIRECTION('ref_axis',(0.409441503265782,-0.912336371851663,0.));
#7057=DIRECTION('center_axis',(0.,0.,1.));
#7058=DIRECTION('ref_axis',(1.,-2.80853466614331E-13,0.));
#7059=DIRECTION('center_axis',(-1.60246890531964E-16,-1.,0.));
#7060=DIRECTION('ref_axis',(1.,-1.60246890531964E-16,0.));
#7061=DIRECTION('',(1.,-1.60246890531964E-16,0.));
#7062=DIRECTION('',(0.,0.,1.));
#7063=DIRECTION('',(1.,-1.60246890531964E-16,0.));
#7064=DIRECTION('',(0.,0.,1.));
#7065=DIRECTION('center_axis',(-0.866025403784439,-0.5,0.));
#7066=DIRECTION('ref_axis',(0.5,-0.866025403784439,0.));
#7067=DIRECTION('',(0.5,-0.866025403784439,0.));
#7068=DIRECTION('',(0.,0.,1.));
#7069=DIRECTION('',(0.5,-0.866025403784439,0.));
#7070=DIRECTION('center_axis',(-0.866025403784439,0.5,0.));
#7071=DIRECTION('ref_axis',(-0.5,-0.866025403784439,0.));
#7072=DIRECTION('',(-0.5,-0.866025403784439,0.));
#7073=DIRECTION('',(0.,0.,1.));
#7074=DIRECTION('',(-0.5,-0.866025403784439,0.));
#7075=DIRECTION('center_axis',(1.60246890531964E-16,1.,0.));
#7076=DIRECTION('ref_axis',(-1.,1.60246890531964E-16,0.));
#7077=DIRECTION('',(-1.,1.60246890531964E-16,0.));
#7078=DIRECTION('',(0.,0.,1.));
#7079=DIRECTION('',(-1.,1.60246890531964E-16,0.));
#7080=DIRECTION('center_axis',(0.866025403784439,0.5,0.));
#7081=DIRECTION('ref_axis',(-0.5,0.866025403784439,0.));
#7082=DIRECTION('',(-0.5,0.866025403784439,0.));
#7083=DIRECTION('',(0.,0.,1.));
#7084=DIRECTION('',(-0.5,0.866025403784439,0.));
#7085=DIRECTION('center_axis',(0.866025403784439,-0.5,0.));
#7086=DIRECTION('ref_axis',(0.5,0.866025403784439,0.));
#7087=DIRECTION('',(0.5,0.866025403784439,0.));
#7088=DIRECTION('',(0.5,0.866025403784439,0.));
#7089=DIRECTION('center_axis',(0.,0.,1.));
#7090=DIRECTION('ref_axis',(1.,0.,0.));
#7091=DIRECTION('center_axis',(0.,0.,1.));
#7092=DIRECTION('ref_axis',(1.,0.,0.));
#7093=DIRECTION('center_axis',(0.,0.,1.));
#7094=DIRECTION('ref_axis',(1.,0.,0.));
#7095=DIRECTION('center_axis',(0.,0.,1.));
#7096=DIRECTION('ref_axis',(1.,0.,0.));
#7097=DIRECTION('',(0.,0.,-1.));
#7098=DIRECTION('center_axis',(0.,0.,1.));
#7099=DIRECTION('ref_axis',(1.,0.,0.));
#7100=DIRECTION('center_axis',(0.,0.,1.));
#7101=DIRECTION('ref_axis',(1.,0.,0.));
#7102=DIRECTION('center_axis',(0.,0.,1.));
#7103=DIRECTION('ref_axis',(1.,0.,0.));
#7104=DIRECTION('axis',(0.,0.,1.));
#7105=DIRECTION('refdir',(1.,0.,0.));
#7106=DIRECTION('center_axis',(0.,0.,-1.));
#7107=DIRECTION('ref_axis',(-0.609355746674506,-0.79289695042594,0.));
#7108=DIRECTION('',(0.,0.,-1.));
#7109=DIRECTION('center_axis',(0.,0.,1.));
#7110=DIRECTION('ref_axis',(1.,-3.8427904741888E-16,0.));
#7111=DIRECTION('center_axis',(0.,0.,-1.));
#7112=DIRECTION('ref_axis',(-0.609355746674506,-0.79289695042594,0.));
#7113=DIRECTION('',(0.,0.,-1.));
#7114=DIRECTION('center_axis',(0.,0.,-1.));
#7115=DIRECTION('ref_axis',(-0.609355746674506,-0.79289695042594,0.));
#7116=DIRECTION('',(0.,0.,-1.));
#7117=DIRECTION('center_axis',(0.,0.,-1.));
#7118=DIRECTION('ref_axis',(-0.609355746674506,-0.79289695042594,0.));
#7119=DIRECTION('',(0.,0.,-1.));
#7120=DIRECTION('center_axis',(0.,0.,-1.));
#7121=DIRECTION('ref_axis',(-0.609355746674506,-0.79289695042594,0.));
#7122=DIRECTION('',(0.,0.,-1.));
#7123=DIRECTION('center_axis',(0.,0.,-1.));
#7124=DIRECTION('ref_axis',(-0.609355746674506,-0.79289695042594,0.));
#7125=DIRECTION('',(0.,0.,-1.));
#7126=DIRECTION('center_axis',(0.,0.,-1.));
#7127=DIRECTION('ref_axis',(1.,-3.8427904741888E-16,0.));
#7128=DIRECTION('center_axis',(0.,0.,-1.));
#7129=DIRECTION('ref_axis',(0.938432355146259,-0.345463044064985,0.));
#7130=DIRECTION('',(0.,0.,-1.));
#7131=DIRECTION('center_axis',(0.,0.,-1.));
#7132=DIRECTION('ref_axis',(1.,0.,0.));
#7133=DIRECTION('center_axis',(0.,0.,-1.));
#7134=DIRECTION('ref_axis',(0.938432355146259,-0.345463044064985,0.));
#7135=DIRECTION('',(0.,0.,-1.));
#7136=DIRECTION('center_axis',(0.,0.,-1.));
#7137=DIRECTION('ref_axis',(1.,0.,0.));
#7138=DIRECTION('center_axis',(0.,0.,-1.));
#7139=DIRECTION('ref_axis',(0.938432355146259,-0.345463044064985,0.));
#7140=DIRECTION('',(0.,0.,-1.));
#7141=DIRECTION('center_axis',(0.,0.,-1.));
#7142=DIRECTION('ref_axis',(0.938432355146259,-0.345463044064985,0.));
#7143=DIRECTION('',(0.,0.,-1.));
#7144=DIRECTION('center_axis',(0.,0.,-1.));
#7145=DIRECTION('ref_axis',(0.938432355146259,-0.345463044064985,0.));
#7146=DIRECTION('',(0.,0.,-1.));
#7147=DIRECTION('center_axis',(0.,0.,-1.));
#7148=DIRECTION('ref_axis',(0.938432355146259,-0.345463044064985,0.));
#7149=DIRECTION('',(0.,0.,-1.));
#7150=DIRECTION('center_axis',(0.,0.,-1.));
#7151=DIRECTION('ref_axis',(1.,0.,0.));
#7152=DIRECTION('center_axis',(0.,0.,-1.));
#7153=DIRECTION('ref_axis',(0.938432355146259,-0.345463044064985,0.));
#7154=DIRECTION('center_axis',(0.,0.,-1.));
#7155=DIRECTION('ref_axis',(-0.609355746674506,-0.79289695042594,0.));
#7156=DIRECTION('center_axis',(0.,0.,1.));
#7157=DIRECTION('ref_axis',(1.,0.,0.));
#7158=DIRECTION('',(0.5,0.866025403784439,0.));
#7159=DIRECTION('',(-0.5,0.866025403784439,0.));
#7160=DIRECTION('',(-1.,1.37354477598826E-16,0.));
#7161=DIRECTION('',(-0.5,-0.866025403784439,0.));
#7162=DIRECTION('',(0.5,-0.866025403784439,0.));
#7163=DIRECTION('',(1.,-1.37354477598826E-16,0.));
#7164=DIRECTION('center_axis',(-1.37354477598826E-16,-1.,0.));
#7165=DIRECTION('ref_axis',(1.,-1.37354477598826E-16,0.));
#7166=DIRECTION('',(1.,-1.37354477598826E-16,0.));
#7167=DIRECTION('',(0.,0.,1.));
#7168=DIRECTION('',(0.,0.,1.));
#7169=DIRECTION('center_axis',(-0.866025403784439,-0.5,0.));
#7170=DIRECTION('ref_axis',(0.5,-0.866025403784439,0.));
#7171=DIRECTION('',(0.5,-0.866025403784439,0.));
#7172=DIRECTION('',(0.,0.,1.));
#7173=DIRECTION('center_axis',(-0.866025403784439,0.5,0.));
#7174=DIRECTION('ref_axis',(-0.5,-0.866025403784439,0.));
#7175=DIRECTION('',(-0.5,-0.866025403784439,0.));
#7176=DIRECTION('',(0.,0.,1.));
#7177=DIRECTION('center_axis',(1.37354477598826E-16,1.,0.));
#7178=DIRECTION('ref_axis',(-1.,1.37354477598826E-16,0.));
#7179=DIRECTION('',(-1.,1.37354477598826E-16,0.));
#7180=DIRECTION('',(0.,0.,1.));
#7181=DIRECTION('center_axis',(0.866025403784439,0.5,0.));
#7182=DIRECTION('ref_axis',(-0.5,0.866025403784439,0.));
#7183=DIRECTION('',(-0.5,0.866025403784439,0.));
#7184=DIRECTION('',(0.,0.,1.));
#7185=DIRECTION('center_axis',(0.866025403784439,-0.5,0.));
#7186=DIRECTION('ref_axis',(0.5,0.866025403784439,0.));
#7187=DIRECTION('',(0.5,0.866025403784439,0.));
#7188=DIRECTION('center_axis',(0.,0.,1.));
#7189=DIRECTION('ref_axis',(1.,0.,0.));
#7190=DIRECTION('axis',(0.,0.,1.));
#7191=DIRECTION('refdir',(1.,0.,0.));
#7192=DIRECTION('center_axis',(1.,0.,0.));
#7193=DIRECTION('ref_axis',(0.,0.,-1.));
#7194=DIRECTION('center_axis',(1.,0.,0.));
#7195=DIRECTION('ref_axis',(0.,0.,-1.));
#7196=DIRECTION('',(1.,0.,0.));
#7197=DIRECTION('center_axis',(1.,0.,0.));
#7198=DIRECTION('ref_axis',(0.,0.,-1.));
#7199=DIRECTION('center_axis',(1.,0.,0.));
#7200=DIRECTION('ref_axis',(0.,0.,-1.));
#7201=DIRECTION('center_axis',(1.,0.,0.));
#7202=DIRECTION('ref_axis',(0.,0.,-1.));
#7203=DIRECTION('center_axis',(1.,0.,0.));
#7204=DIRECTION('ref_axis',(0.,0.,-1.));
#7205=DIRECTION('',(1.,0.,0.));
#7206=DIRECTION('center_axis',(1.,0.,0.));
#7207=DIRECTION('ref_axis',(0.,0.,-1.));
#7208=DIRECTION('center_axis',(1.,0.,0.));
#7209=DIRECTION('ref_axis',(0.,0.,-1.));
#7210=DIRECTION('center_axis',(1.,0.,0.));
#7211=DIRECTION('ref_axis',(0.,0.,-1.));
#7212=DIRECTION('center_axis',(1.,0.,0.));
#7213=DIRECTION('ref_axis',(0.,0.,-1.));
#7214=DIRECTION('',(1.,0.,0.));
#7215=DIRECTION('center_axis',(1.,0.,0.));
#7216=DIRECTION('ref_axis',(0.,0.,-1.));
#7217=DIRECTION('center_axis',(1.,0.,0.));
#7218=DIRECTION('ref_axis',(0.,0.,-1.));
#7219=DIRECTION('center_axis',(1.,0.,0.));
#7220=DIRECTION('ref_axis',(0.,0.,-1.));
#7221=DIRECTION('center_axis',(1.,0.,0.));
#7222=DIRECTION('ref_axis',(0.,0.,-1.));
#7223=DIRECTION('',(1.,0.,0.));
#7224=DIRECTION('center_axis',(1.,0.,0.));
#7225=DIRECTION('ref_axis',(0.,0.,-1.));
#7226=DIRECTION('center_axis',(1.,0.,0.));
#7227=DIRECTION('ref_axis',(0.,0.,-1.));
#7228=DIRECTION('center_axis',(0.,1.,0.));
#7229=DIRECTION('ref_axis',(-1.,0.,0.));
#7230=DIRECTION('',(1.,0.,0.));
#7231=DIRECTION('',(0.,0.,1.));
#7232=DIRECTION('',(-1.,0.,0.));
#7233=DIRECTION('',(0.,0.,-1.));
#7234=DIRECTION('center_axis',(0.,1.,0.));
#7235=DIRECTION('ref_axis',(-1.,0.,0.));
#7236=DIRECTION('',(1.,0.,0.));
#7237=DIRECTION('',(0.,0.,1.));
#7238=DIRECTION('',(-1.,0.,0.));
#7239=DIRECTION('',(0.,0.,-1.));
#7240=DIRECTION('center_axis',(0.,1.,0.));
#7241=DIRECTION('ref_axis',(-1.,0.,0.));
#7242=DIRECTION('',(1.,0.,0.));
#7243=DIRECTION('',(0.,0.,1.));
#7244=DIRECTION('',(-1.,0.,0.));
#7245=DIRECTION('',(0.,0.,-1.));
#7246=DIRECTION('center_axis',(0.,1.,0.));
#7247=DIRECTION('ref_axis',(-1.,0.,0.));
#7248=DIRECTION('',(1.,0.,0.));
#7249=DIRECTION('',(0.,0.,1.));
#7250=DIRECTION('',(-1.,0.,0.));
#7251=DIRECTION('',(0.,0.,-1.));
#7252=DIRECTION('center_axis',(0.,-1.,0.));
#7253=DIRECTION('ref_axis',(1.,0.,0.));
#7254=DIRECTION('',(-1.,0.,0.));
#7255=DIRECTION('',(0.,0.,1.));
#7256=DIRECTION('',(1.,0.,0.));
#7257=DIRECTION('',(0.,0.,1.));
#7258=DIRECTION('center_axis',(0.,-1.,0.));
#7259=DIRECTION('ref_axis',(1.,0.,0.));
#7260=DIRECTION('',(-1.,0.,0.));
#7261=DIRECTION('',(0.,0.,1.));
#7262=DIRECTION('',(1.,0.,0.));
#7263=DIRECTION('',(0.,0.,1.));
#7264=DIRECTION('center_axis',(0.,-1.,0.));
#7265=DIRECTION('ref_axis',(1.,0.,0.));
#7266=DIRECTION('',(-1.,0.,0.));
#7267=DIRECTION('',(0.,0.,1.));
#7268=DIRECTION('',(1.,0.,0.));
#7269=DIRECTION('',(0.,0.,1.));
#7270=DIRECTION('center_axis',(0.,-1.,0.));
#7271=DIRECTION('ref_axis',(1.,0.,0.));
#7272=DIRECTION('',(-1.,0.,0.));
#7273=DIRECTION('',(0.,0.,1.));
#7274=DIRECTION('',(1.,0.,0.));
#7275=DIRECTION('',(0.,0.,1.));
#7276=DIRECTION('center_axis',(-1.,0.,0.));
#7277=DIRECTION('ref_axis',(0.,-1.,0.));
#7278=DIRECTION('',(0.,-1.,0.));
#7279=DIRECTION('',(0.,0.,-1.));
#7280=DIRECTION('',(0.,1.,0.));
#7281=DIRECTION('',(0.,0.,1.));
#7282=DIRECTION('',(0.,-1.,0.));
#7283=DIRECTION('',(0.,-1.,0.));
#7284=DIRECTION('',(0.,0.,1.));
#7285=DIRECTION('',(0.,-1.,0.));
#7286=DIRECTION('',(0.,-1.,0.));
#7287=DIRECTION('',(0.,0.,1.));
#7288=DIRECTION('',(0.,-1.,0.));
#7289=DIRECTION('',(0.,-1.,0.));
#7290=DIRECTION('',(0.,0.,1.));
#7291=DIRECTION('',(0.,-1.,0.));
#7292=DIRECTION('',(0.,-1.,0.));
#7293=DIRECTION('',(0.,0.,1.));
#7294=DIRECTION('',(0.,-1.,0.));
#7295=DIRECTION('',(0.,0.,-1.));
#7296=DIRECTION('',(0.,-1.,0.));
#7297=DIRECTION('',(0.,-1.,0.));
#7298=DIRECTION('',(0.,0.,-1.));
#7299=DIRECTION('',(0.,-1.,0.));
#7300=DIRECTION('',(0.,-1.,0.));
#7301=DIRECTION('',(0.,0.,-1.));
#7302=DIRECTION('',(0.,-1.,0.));
#7303=DIRECTION('',(0.,-1.,0.));
#7304=DIRECTION('',(0.,0.,-1.));
#7305=DIRECTION('',(0.,-1.,0.));
#7306=DIRECTION('center_axis',(0.,0.,1.));
#7307=DIRECTION('ref_axis',(1.,0.,0.));
#7308=DIRECTION('',(-1.,0.,0.));
#7309=DIRECTION('',(0.,-1.,0.));
#7310=DIRECTION('center_axis',(0.,0.,1.));
#7311=DIRECTION('ref_axis',(1.,0.,0.));
#7312=DIRECTION('',(0.,-1.,0.));
#7313=DIRECTION('',(1.,0.,0.));
#7314=DIRECTION('center_axis',(1.,0.,0.));
#7315=DIRECTION('ref_axis',(0.,1.,0.));
#7316=DIRECTION('',(0.,0.,1.));
#7317=DIRECTION('',(0.,1.,0.));
#7318=DIRECTION('center_axis',(1.,0.,0.));
#7319=DIRECTION('ref_axis',(0.,1.,0.));
#7320=DIRECTION('',(0.,1.,0.));
#7321=DIRECTION('',(0.,0.,1.));
#7322=DIRECTION('center_axis',(0.,0.,1.));
#7323=DIRECTION('ref_axis',(1.,0.,0.));
#7324=DIRECTION('',(1.,0.,0.));
#7325=DIRECTION('center_axis',(0.,0.,1.));
#7326=DIRECTION('ref_axis',(1.,0.,0.));
#7327=DIRECTION('',(-1.,0.,0.));
#7328=DIRECTION('center_axis',(0.,0.,1.));
#7329=DIRECTION('ref_axis',(1.,0.,0.));
#7330=DIRECTION('',(-1.,0.,0.));
#7331=DIRECTION('',(0.,-1.,0.));
#7332=DIRECTION('center_axis',(0.,0.,1.));
#7333=DIRECTION('ref_axis',(1.,0.,0.));
#7334=DIRECTION('',(0.,-1.,0.));
#7335=DIRECTION('',(1.,0.,0.));
#7336=DIRECTION('center_axis',(1.,0.,0.));
#7337=DIRECTION('ref_axis',(0.,1.,0.));
#7338=DIRECTION('',(0.,0.,1.));
#7339=DIRECTION('',(0.,1.,0.));
#7340=DIRECTION('center_axis',(1.,0.,0.));
#7341=DIRECTION('ref_axis',(0.,1.,0.));
#7342=DIRECTION('',(0.,1.,0.));
#7343=DIRECTION('',(0.,0.,1.));
#7344=DIRECTION('center_axis',(0.,0.,1.));
#7345=DIRECTION('ref_axis',(1.,0.,0.));
#7346=DIRECTION('',(1.,0.,0.));
#7347=DIRECTION('center_axis',(0.,0.,1.));
#7348=DIRECTION('ref_axis',(1.,0.,0.));
#7349=DIRECTION('',(-1.,0.,0.));
#7350=DIRECTION('center_axis',(0.,0.,1.));
#7351=DIRECTION('ref_axis',(1.,0.,0.));
#7352=DIRECTION('',(-1.,0.,0.));
#7353=DIRECTION('',(0.,-1.,0.));
#7354=DIRECTION('center_axis',(0.,0.,1.));
#7355=DIRECTION('ref_axis',(1.,0.,0.));
#7356=DIRECTION('',(0.,-1.,0.));
#7357=DIRECTION('',(1.,0.,0.));
#7358=DIRECTION('center_axis',(1.,0.,0.));
#7359=DIRECTION('ref_axis',(0.,1.,0.));
#7360=DIRECTION('',(0.,0.,1.));
#7361=DIRECTION('',(0.,1.,0.));
#7362=DIRECTION('center_axis',(1.,0.,0.));
#7363=DIRECTION('ref_axis',(0.,1.,0.));
#7364=DIRECTION('',(0.,1.,0.));
#7365=DIRECTION('',(0.,0.,1.));
#7366=DIRECTION('center_axis',(0.,0.,1.));
#7367=DIRECTION('ref_axis',(1.,0.,0.));
#7368=DIRECTION('',(1.,0.,0.));
#7369=DIRECTION('center_axis',(0.,0.,1.));
#7370=DIRECTION('ref_axis',(1.,0.,0.));
#7371=DIRECTION('',(-1.,0.,0.));
#7372=DIRECTION('center_axis',(0.,0.,1.));
#7373=DIRECTION('ref_axis',(1.,0.,0.));
#7374=DIRECTION('',(-1.,0.,0.));
#7375=DIRECTION('',(0.,-1.,0.));
#7376=DIRECTION('center_axis',(0.,0.,1.));
#7377=DIRECTION('ref_axis',(1.,0.,0.));
#7378=DIRECTION('',(0.,-1.,0.));
#7379=DIRECTION('',(1.,0.,0.));
#7380=DIRECTION('center_axis',(1.,0.,0.));
#7381=DIRECTION('ref_axis',(0.,1.,0.));
#7382=DIRECTION('',(0.,0.,1.));
#7383=DIRECTION('',(0.,1.,0.));
#7384=DIRECTION('center_axis',(1.,0.,0.));
#7385=DIRECTION('ref_axis',(0.,1.,0.));
#7386=DIRECTION('',(0.,1.,0.));
#7387=DIRECTION('',(0.,0.,1.));
#7388=DIRECTION('center_axis',(0.,0.,1.));
#7389=DIRECTION('ref_axis',(1.,0.,0.));
#7390=DIRECTION('',(1.,0.,0.));
#7391=DIRECTION('center_axis',(0.,0.,1.));
#7392=DIRECTION('ref_axis',(1.,0.,0.));
#7393=DIRECTION('',(-1.,0.,0.));
#7394=DIRECTION('center_axis',(0.,1.,0.));
#7395=DIRECTION('ref_axis',(-1.,0.,0.));
#7396=DIRECTION('',(-1.,0.,0.));
#7397=DIRECTION('',(0.,0.,1.));
#7398=DIRECTION('',(-1.,0.,0.));
#7399=DIRECTION('center_axis',(0.,0.,1.));
#7400=DIRECTION('ref_axis',(1.,0.,0.));
#7401=DIRECTION('',(1.,0.,0.));
#7402=DIRECTION('',(0.,-1.,0.));
#7403=DIRECTION('center_axis',(0.,-1.,0.));
#7404=DIRECTION('ref_axis',(1.,0.,0.));
#7405=DIRECTION('',(1.,0.,0.));
#7406=DIRECTION('',(0.,0.,1.));
#7407=DIRECTION('center_axis',(-1.,0.,0.));
#7408=DIRECTION('ref_axis',(0.,-1.,0.));
#7409=DIRECTION('',(0.,-1.,0.));
#7410=DIRECTION('center_axis',(0.,0.,1.));
#7411=DIRECTION('ref_axis',(1.,0.,0.));
#7412=DIRECTION('axis',(0.,0.,1.));
#7413=DIRECTION('refdir',(1.,0.,0.));
#7414=DIRECTION('center_axis',(0.,-1.,0.));
#7415=DIRECTION('ref_axis',(1.,0.,0.));
#7416=DIRECTION('',(-1.,0.,0.));
#7417=DIRECTION('',(0.,0.,1.));
#7418=DIRECTION('',(1.,0.,0.));
#7419=DIRECTION('',(0.,0.,-1.));
#7420=DIRECTION('center_axis',(0.,1.,0.));
#7421=DIRECTION('ref_axis',(-1.,0.,0.));
#7422=DIRECTION('',(1.,0.,0.));
#7423=DIRECTION('',(0.,0.,1.));
#7424=DIRECTION('',(-1.,0.,0.));
#7425=DIRECTION('',(0.,0.,-1.));
#7426=DIRECTION('center_axis',(0.,0.,1.));
#7427=DIRECTION('ref_axis',(1.,0.,0.));
#7428=DIRECTION('',(0.,1.,0.));
#7429=DIRECTION('',(0.,-1.,0.));
#7430=DIRECTION('center_axis',(1.,0.,0.));
#7431=DIRECTION('ref_axis',(0.,1.,0.));
#7432=DIRECTION('',(0.,1.,0.));
#7433=DIRECTION('',(0.,0.,1.));
#7434=DIRECTION('',(0.,1.,0.));
#7435=DIRECTION('',(0.,0.,1.));
#7436=DIRECTION('',(0.,1.,0.));
#7437=DIRECTION('center_axis',(0.,0.,1.));
#7438=DIRECTION('ref_axis',(1.,0.,0.));
#7439=DIRECTION('',(0.,-1.,0.));
#7440=DIRECTION('',(1.,0.,0.));
#7441=DIRECTION('center_axis',(0.,1.,0.));
#7442=DIRECTION('ref_axis',(-1.,0.,0.));
#7443=DIRECTION('',(-1.,0.,0.));
#7444=DIRECTION('',(0.,0.,1.));
#7445=DIRECTION('',(-1.,0.,0.));
#7446=DIRECTION('center_axis',(0.,-1.,0.));
#7447=DIRECTION('ref_axis',(1.,0.,0.));
#7448=DIRECTION('',(1.,0.,0.));
#7449=DIRECTION('',(0.,0.,1.));
#7450=DIRECTION('center_axis',(-1.,0.,0.));
#7451=DIRECTION('ref_axis',(0.,-1.,0.));
#7452=DIRECTION('',(0.,-1.,0.));
#7453=DIRECTION('',(0.,-1.,0.));
#7454=DIRECTION('center_axis',(0.,0.,1.));
#7455=DIRECTION('ref_axis',(1.,0.,0.));
#7456=DIRECTION('center_axis',(0.,0.,1.));
#7457=DIRECTION('ref_axis',(1.,0.,0.));
#7458=DIRECTION('axis',(0.,0.,1.));
#7459=DIRECTION('refdir',(1.,0.,0.));
#7460=DIRECTION('center_axis',(0.,1.,0.));
#7461=DIRECTION('ref_axis',(-1.,0.,0.));
#7462=DIRECTION('',(-1.,0.,0.));
#7463=DIRECTION('',(0.,0.,1.));
#7464=DIRECTION('',(-1.,0.,0.));
#7465=DIRECTION('',(0.,0.,1.));
#7466=DIRECTION('center_axis',(1.,0.,0.));
#7467=DIRECTION('ref_axis',(0.,1.,0.));
#7468=DIRECTION('',(0.,1.,0.));
#7469=DIRECTION('',(0.,1.,0.));
#7470=DIRECTION('',(0.,0.,1.));
#7471=DIRECTION('center_axis',(0.,-1.,0.));
#7472=DIRECTION('ref_axis',(1.,0.,0.));
#7473=DIRECTION('',(1.,0.,0.));
#7474=DIRECTION('',(1.,0.,0.));
#7475=DIRECTION('',(0.,0.,1.));
#7476=DIRECTION('center_axis',(-1.,0.,0.));
#7477=DIRECTION('ref_axis',(0.,-1.,0.));
#7478=DIRECTION('',(0.,-1.,0.));
#7479=DIRECTION('',(0.,-1.,0.));
#7480=DIRECTION('center_axis',(0.,0.,1.));
#7481=DIRECTION('ref_axis',(1.,0.,0.));
#7482=DIRECTION('center_axis',(0.,0.,1.));
#7483=DIRECTION('ref_axis',(1.,0.,0.));
#7484=DIRECTION('axis',(0.,0.,1.));
#7485=DIRECTION('refdir',(1.,0.,0.));
#7486=DIRECTION('center_axis',(0.,0.,1.));
#7487=DIRECTION('ref_axis',(1.,0.,0.));
#7488=DIRECTION('center_axis',(0.,0.,1.));
#7489=DIRECTION('ref_axis',(1.,0.,0.));
#7490=DIRECTION('',(0.,0.,-1.));
#7491=DIRECTION('center_axis',(0.,0.,1.));
#7492=DIRECTION('ref_axis',(1.,0.,0.));
#7493=DIRECTION('center_axis',(0.,0.,1.));
#7494=DIRECTION('ref_axis',(1.,0.,0.));
#7495=DIRECTION('center_axis',(0.,0.,1.));
#7496=DIRECTION('ref_axis',(1.,0.,0.));
#7497=DIRECTION('',(0.,0.,1.));
#7498=DIRECTION('',(1.,0.,0.));
#7499=DIRECTION('',(0.,0.,1.));
#7500=DIRECTION('',(1.,0.,0.));
#7501=DIRECTION('',(0.,0.,1.));
#7502=DIRECTION('',(1.,0.,0.));
#7503=DIRECTION('',(0.,0.,1.));
#7504=DIRECTION('',(1.,0.,0.));
#7505=DIRECTION('',(0.,0.,1.));
#7506=DIRECTION('',(1.,0.,0.));
#7507=DIRECTION('',(0.,0.,1.));
#7508=DIRECTION('',(1.,0.,0.));
#7509=DIRECTION('',(0.,0.,1.));
#7510=DIRECTION('',(1.,0.,0.));
#7511=DIRECTION('',(0.,0.,1.));
#7512=DIRECTION('',(1.,0.,0.));
#7513=DIRECTION('',(-1.,0.,0.));
#7514=DIRECTION('',(0.,-0.5,0.866025403784439));
#7515=DIRECTION('',(-1.,0.,0.));
#7516=DIRECTION('',(0.,-1.,0.));
#7517=DIRECTION('',(0.,0.,1.));
#7518=DIRECTION('',(1.,0.,0.));
#7519=DIRECTION('',(0.,0.,1.));
#7520=DIRECTION('',(1.,0.,0.));
#7521=DIRECTION('',(0.,0.,1.));
#7522=DIRECTION('',(1.,0.,0.));
#7523=DIRECTION('',(0.,0.,1.));
#7524=DIRECTION('',(1.,0.,0.));
#7525=DIRECTION('',(1.,0.,2.22044604925031E-16));
#7526=DIRECTION('',(2.22044604925031E-16,0.,-1.));
#7527=DIRECTION('',(1.22464679914735E-16,0.,-1.));
#7528=DIRECTION('',(-1.,0.,-1.22464679914735E-16));
#7529=DIRECTION('',(1.22464679914735E-16,0.,-1.));
#7530=DIRECTION('',(-1.,0.,-1.22464679914735E-16));
#7531=DIRECTION('',(0.,0.,1.));
#7532=DIRECTION('',(1.,0.,0.));
#7533=DIRECTION('',(0.,0.,1.));
#7534=DIRECTION('',(1.,0.,0.));
#7535=DIRECTION('',(0.,-1.,0.));
#7536=DIRECTION('',(0.5,0.,0.866025403784439));
#7537=DIRECTION('',(0.,-1.,0.));
#7538=DIRECTION('',(1.,0.,0.));
#7539=DIRECTION('',(-1.,0.,0.));
#7540=DIRECTION('',(0.,-0.5,0.866025403784439));
#7541=DIRECTION('',(-1.,0.,0.));
#7542=DIRECTION('',(0.,-1.,0.));
#7543=DIRECTION('',(0.,-1.,0.));
#7544=DIRECTION('',(0.5,0.,0.866025403784439));
#7545=DIRECTION('',(0.,-1.,0.));
#7546=DIRECTION('',(1.,0.,0.));
#7547=DIRECTION('',(1.22464679914735E-16,0.,-1.));
#7548=DIRECTION('',(-1.,0.,-1.22464679914735E-16));
#7549=DIRECTION('',(1.22464679914735E-16,0.,-1.));
#7550=DIRECTION('',(-1.,0.,-1.22464679914735E-16));
#7551=DIRECTION('',(0.,0.,1.));
#7552=DIRECTION('',(1.,0.,0.));
#7553=DIRECTION('',(0.,0.,1.));
#7554=DIRECTION('',(1.,0.,0.));
#7555=DIRECTION('',(1.,0.,2.22044604925031E-16));
#7556=DIRECTION('',(2.22044604925031E-16,0.,-1.));
#7557=DIRECTION('',(1.,0.,2.22044604925031E-16));
#7558=DIRECTION('',(2.22044604925031E-16,0.,-1.));
#7559=DIRECTION('',(1.,0.,2.22044604925031E-16));
#7560=DIRECTION('',(2.22044604925031E-16,0.,-1.));
#7561=CARTESIAN_POINT('',(0.,0.,0.));
#7562=CARTESIAN_POINT('',(0.,0.,0.));
#7563=CARTESIAN_POINT('Origin',(77.36,0.6,0.));
#7564=CARTESIAN_POINT('',(77.36,0.6,0.));
#7565=CARTESIAN_POINT('',(0.,0.6,0.));
#7566=CARTESIAN_POINT('',(77.36,0.6,0.));
#7567=CARTESIAN_POINT('',(0.,0.6,177.36));
#7568=CARTESIAN_POINT('',(0.,0.6,0.));
#7569=CARTESIAN_POINT('',(77.36,0.6,177.36));
#7570=CARTESIAN_POINT('',(77.36,0.6,177.36));
#7571=CARTESIAN_POINT('',(77.36,0.6,0.));
#7572=CARTESIAN_POINT('Origin',(77.36,0.,0.));
#7573=CARTESIAN_POINT('',(77.36,0.,0.));
#7574=CARTESIAN_POINT('',(77.36,0.,0.));
#7575=CARTESIAN_POINT('',(77.36,0.,177.36));
#7576=CARTESIAN_POINT('',(77.36,0.,177.36));
#7577=CARTESIAN_POINT('',(77.36,0.,0.));
#7578=CARTESIAN_POINT('Origin',(0.,0.,0.));
#7579=CARTESIAN_POINT('',(0.,0.,0.));
#7580=CARTESIAN_POINT('',(0.,0.,0.));
#7581=CARTESIAN_POINT('',(0.,0.,177.36));
#7582=CARTESIAN_POINT('',(0.,0.,177.36));
#7583=CARTESIAN_POINT('',(0.,0.,0.));
#7584=CARTESIAN_POINT('Origin',(0.,0.6,0.));
#7585=CARTESIAN_POINT('',(0.,0.6,0.));
#7586=CARTESIAN_POINT('',(0.,0.6,177.36));
#7587=CARTESIAN_POINT('Origin',(38.68,0.3,177.36));
#7588=CARTESIAN_POINT('Origin',(38.68,0.3,0.));
#7589=CARTESIAN_POINT('',(0.,0.,0.));
#7590=CARTESIAN_POINT('Origin',(69.,-0.2,89.));
#7591=CARTESIAN_POINT('',(69.,-0.2,89.));
#7592=CARTESIAN_POINT('',(75.,-0.2,89.));
#7593=CARTESIAN_POINT('',(73.5,-0.2,89.));
#7594=CARTESIAN_POINT('',(69.,-2.,89.));
#7595=CARTESIAN_POINT('',(69.,-0.2,89.));
#7596=CARTESIAN_POINT('',(75.,-2.,89.));
#7597=CARTESIAN_POINT('',(35.7,-2.,89.));
#7598=CARTESIAN_POINT('',(75.,-0.2,89.));
#7599=CARTESIAN_POINT('Origin',(69.,-0.2,90.));
#7600=CARTESIAN_POINT('',(69.,-0.2,91.));
#7601=CARTESIAN_POINT('Origin',(69.,-0.2,90.));
#7602=CARTESIAN_POINT('',(69.,-2.,91.));
#7603=CARTESIAN_POINT('',(69.,-0.2,91.));
#7604=CARTESIAN_POINT('Origin',(69.,-2.,90.));
#7605=CARTESIAN_POINT('Origin',(75.,-0.2,91.));
#7606=CARTESIAN_POINT('',(75.,-0.2,91.));
#7607=CARTESIAN_POINT('',(76.5,-0.2,91.));
#7608=CARTESIAN_POINT('',(75.,-2.,91.));
#7609=CARTESIAN_POINT('',(75.,-0.2,91.));
#7610=CARTESIAN_POINT('',(38.7,-2.,91.));
#7611=CARTESIAN_POINT('Origin',(75.,-0.2,90.));
#7612=CARTESIAN_POINT('Origin',(75.,-0.2,90.));
#7613=CARTESIAN_POINT('Origin',(75.,-2.,90.));
#7614=CARTESIAN_POINT('Origin',(3.4,-0.2,60.));
#7615=CARTESIAN_POINT('',(3.175,-0.2,60.));
#7616=CARTESIAN_POINT('Origin',(3.4,-0.2,60.));
#7617=CARTESIAN_POINT('',(3.175,-2.,60.));
#7618=CARTESIAN_POINT('',(3.175,-0.2,60.));
#7619=CARTESIAN_POINT('Origin',(3.4,-2.,60.));
#7620=CARTESIAN_POINT('Origin',(3.4,-0.2,120.));
#7621=CARTESIAN_POINT('',(3.175,-0.2,120.));
#7622=CARTESIAN_POINT('Origin',(3.4,-0.2,120.));
#7623=CARTESIAN_POINT('',(3.175,-2.,120.));
#7624=CARTESIAN_POINT('',(3.175,-0.2,120.));
#7625=CARTESIAN_POINT('Origin',(3.4,-2.,120.));
#7626=CARTESIAN_POINT('Origin',(78.,-0.2,0.2));
#7627=CARTESIAN_POINT('',(78.,-0.2,0.2));
#7628=CARTESIAN_POINT('',(2.4,-0.2,0.2));
#7629=CARTESIAN_POINT('',(78.,-0.2,0.2));
#7630=CARTESIAN_POINT('',(2.4,-0.2,179.8));
#7631=CARTESIAN_POINT('',(2.4,-0.2,0.2));
#7632=CARTESIAN_POINT('',(78.,-0.2,179.8));
#7633=CARTESIAN_POINT('',(78.,-0.2,179.8));
#7634=CARTESIAN_POINT('',(78.,-0.2,0.2));
#7635=CARTESIAN_POINT('Origin',(78.,-2.,0.2));
#7636=CARTESIAN_POINT('',(78.,-2.,0.2));
#7637=CARTESIAN_POINT('',(78.,-2.,0.2));
#7638=CARTESIAN_POINT('',(78.,-2.,179.8));
#7639=CARTESIAN_POINT('',(78.,-2.,179.8));
#7640=CARTESIAN_POINT('',(78.,-2.,0.2));
#7641=CARTESIAN_POINT('Origin',(2.4,-2.,0.2));
#7642=CARTESIAN_POINT('',(2.4,-2.,0.2));
#7643=CARTESIAN_POINT('',(2.4,-2.,0.2));
#7644=CARTESIAN_POINT('',(2.4,-2.,179.8));
#7645=CARTESIAN_POINT('',(2.4,-2.,179.8));
#7646=CARTESIAN_POINT('',(2.4,-2.,0.2));
#7647=CARTESIAN_POINT('Origin',(2.4,-0.2,0.2));
#7648=CARTESIAN_POINT('',(2.4,-0.2,0.2));
#7649=CARTESIAN_POINT('',(2.4,-0.2,179.8));
#7650=CARTESIAN_POINT('Origin',(40.2,-1.1,179.8));
#7651=CARTESIAN_POINT('Origin',(40.2,-1.1,0.2));
#7652=CARTESIAN_POINT('',(0.,0.,0.));
#7653=CARTESIAN_POINT('Origin',(0.,2.,55.));
#7654=CARTESIAN_POINT('',(0.,2.,55.225));
#7655=CARTESIAN_POINT('Origin',(0.,2.,55.));
#7656=CARTESIAN_POINT('',(0.2,2.,55.225));
#7657=CARTESIAN_POINT('',(0.,2.,55.225));
#7658=CARTESIAN_POINT('Origin',(0.2,2.,55.));
#7659=CARTESIAN_POINT('Origin',(0.,2.,115.));
#7660=CARTESIAN_POINT('',(0.,2.,115.225));
#7661=CARTESIAN_POINT('Origin',(0.,2.,115.));
#7662=CARTESIAN_POINT('',(0.2,2.,115.225));
#7663=CARTESIAN_POINT('',(0.,2.,115.225));
#7664=CARTESIAN_POINT('Origin',(0.2,2.,115.));
#7665=CARTESIAN_POINT('Origin',(0.,0.,113.343333333333));
#7666=CARTESIAN_POINT('',(0.,0.42,113.343333333333));
#7667=CARTESIAN_POINT('',(0.,0.2,113.343333333333));
#7668=CARTESIAN_POINT('',(0.,1.5,113.343333333333));
#7669=CARTESIAN_POINT('',(0.2,0.369323706252388,113.343333333333));
#7670=CARTESIAN_POINT('Origin',(0.,0.,113.343333333333));
#7671=CARTESIAN_POINT('',(0.2,0.2,113.343333333333));
#7672=CARTESIAN_POINT('',(0.2,0.1,113.343333333333));
#7673=CARTESIAN_POINT('',(0.,0.2,113.343333333333));
#7674=CARTESIAN_POINT('Origin',(0.,0.,56.6566666666667));
#7675=CARTESIAN_POINT('',(0.,0.42,56.6566666666667));
#7676=CARTESIAN_POINT('',(0.,0.42,56.6566666666667));
#7677=CARTESIAN_POINT('',(0.2,0.369323706252388,56.6566666666667));
#7678=CARTESIAN_POINT('Origin',(0.,0.,56.6566666666667));
#7679=CARTESIAN_POINT('',(0.2,0.369323706252388,56.6566666666667));
#7680=CARTESIAN_POINT('Origin',(0.,0.,56.6566666666667));
#7681=CARTESIAN_POINT('',(0.,0.2,56.6566666666667));
#7682=CARTESIAN_POINT('',(0.,1.5,56.6566666666667));
#7683=CARTESIAN_POINT('',(0.2,0.2,56.6566666666667));
#7684=CARTESIAN_POINT('',(0.,0.2,56.6566666666667));
#7685=CARTESIAN_POINT('',(0.2,0.1,56.6566666666667));
#7686=CARTESIAN_POINT('Origin',(0.2,0.2,0.));
#7687=CARTESIAN_POINT('',(0.2,0.2,56.6466666666667));
#7688=CARTESIAN_POINT('',(0.2,0.2,0.));
#7689=CARTESIAN_POINT('',(0.2,0.346410161513776,56.6466666666667));
#7690=CARTESIAN_POINT('',(0.2,0.1,56.6466666666667));
#7691=CARTESIAN_POINT('',(0.2,0.346410161513776,0.));
#7692=CARTESIAN_POINT('',(0.2,0.346410161513776,0.));
#7693=CARTESIAN_POINT('',(0.2,3.,0.));
#7694=CARTESIAN_POINT('',(0.2,0.2,0.));
#7695=CARTESIAN_POINT('',(0.2,3.,170.));
#7696=CARTESIAN_POINT('',(0.2,3.,0.));
#7697=CARTESIAN_POINT('',(0.2,0.346410161513776,170.));
#7698=CARTESIAN_POINT('',(0.2,0.2,170.));
#7699=CARTESIAN_POINT('',(0.2,0.346410161513776,113.353333333333));
#7700=CARTESIAN_POINT('',(0.2,0.346410161513776,113.353333333333));
#7701=CARTESIAN_POINT('',(0.2,0.2,113.353333333333));
#7702=CARTESIAN_POINT('',(0.2,0.1,113.353333333333));
#7703=CARTESIAN_POINT('',(0.2,0.2,0.));
#7704=CARTESIAN_POINT('Origin',(0.,0.2,0.));
#7705=CARTESIAN_POINT('',(0.,0.2,0.));
#7706=CARTESIAN_POINT('',(0.,0.2,0.));
#7707=CARTESIAN_POINT('',(0.0916515138991168,0.2,0.));
#7708=CARTESIAN_POINT('',(0.,0.2,0.));
#7709=CARTESIAN_POINT('',(0.0916515138991168,0.2,56.6466666666667));
#7710=CARTESIAN_POINT('',(0.0916515138991168,0.2,0.));
#7711=CARTESIAN_POINT('',(0.,0.2,56.6466666666667));
#7712=CARTESIAN_POINT('Origin',(0.,0.2,0.));
#7713=CARTESIAN_POINT('',(0.0916515138991168,0.2,113.353333333333));
#7714=CARTESIAN_POINT('',(0.,0.2,113.353333333333));
#7715=CARTESIAN_POINT('',(0.0916515138991168,0.2,170.));
#7716=CARTESIAN_POINT('',(0.0916515138991168,0.2,113.353333333333));
#7717=CARTESIAN_POINT('',(0.,0.2,170.));
#7718=CARTESIAN_POINT('',(0.,0.2,170.));
#7719=CARTESIAN_POINT('',(0.,0.2,0.));
#7720=CARTESIAN_POINT('Origin',(0.,0.,113.353333333333));
#7721=CARTESIAN_POINT('',(0.,0.4,113.353333333333));
#7722=CARTESIAN_POINT('Origin',(0.,0.,113.353333333333));
#7723=CARTESIAN_POINT('',(0.,0.22,113.353333333333));
#7724=CARTESIAN_POINT('',(0.,1.5,113.353333333333));
#7725=CARTESIAN_POINT('Origin',(0.,0.,113.353333333333));
#7726=CARTESIAN_POINT('Origin',(0.,0.,113.353333333333));
#7727=CARTESIAN_POINT('',(0.,0.4,170.));
#7728=CARTESIAN_POINT('Origin',(0.,0.,170.));
#7729=CARTESIAN_POINT('',(0.,0.4,113.353333333333));
#7730=CARTESIAN_POINT('Origin',(0.,0.,113.353333333333));
#7731=CARTESIAN_POINT('',(0.,0.22,170.));
#7732=CARTESIAN_POINT('',(0.,0.22,113.353333333333));
#7733=CARTESIAN_POINT('Origin',(0.,0.,170.));
#7734=CARTESIAN_POINT('Origin',(0.1,1.6,170.));
#7735=CARTESIAN_POINT('',(0.,3.,170.));
#7736=CARTESIAN_POINT('',(0.2,3.,170.));
#7737=CARTESIAN_POINT('',(0.,3.,170.));
#7738=CARTESIAN_POINT('',(0.,3.,170.));
#7739=CARTESIAN_POINT('Origin',(0.,3.,0.));
#7740=CARTESIAN_POINT('',(0.,3.,0.));
#7741=CARTESIAN_POINT('',(0.,3.,0.));
#7742=CARTESIAN_POINT('',(0.,0.4,0.));
#7743=CARTESIAN_POINT('',(0.,3.,0.));
#7744=CARTESIAN_POINT('',(0.,0.4,56.6466666666667));
#7745=CARTESIAN_POINT('',(0.,0.4,0.));
#7746=CARTESIAN_POINT('',(0.,0.22,56.6466666666667));
#7747=CARTESIAN_POINT('',(0.,1.5,56.6466666666667));
#7748=CARTESIAN_POINT('',(0.,0.22,0.));
#7749=CARTESIAN_POINT('',(0.,0.22,0.));
#7750=CARTESIAN_POINT('',(0.,3.,0.));
#7751=CARTESIAN_POINT('Origin',(0.,0.,0.));
#7752=CARTESIAN_POINT('Origin',(0.,0.,0.));
#7753=CARTESIAN_POINT('Origin',(0.,0.,56.6466666666667));
#7754=CARTESIAN_POINT('Origin',(0.,0.,0.));
#7755=CARTESIAN_POINT('Origin',(0.,0.,56.6466666666667));
#7756=CARTESIAN_POINT('Origin',(0.,0.,0.));
#7757=CARTESIAN_POINT('Origin',(0.,0.,56.6466666666667));
#7758=CARTESIAN_POINT('Origin',(0.2,3.,0.));
#7759=CARTESIAN_POINT('',(0.2,3.,0.));
#7760=CARTESIAN_POINT('Origin',(0.1,1.6,0.));
#7761=CARTESIAN_POINT('',(0.,0.,0.));
#7762=CARTESIAN_POINT('Origin',(1.6,0.4,55.));
#7763=CARTESIAN_POINT('',(1.375,0.4,55.));
#7764=CARTESIAN_POINT('Origin',(1.6,0.4,55.));
#7765=CARTESIAN_POINT('',(1.375,0.2,55.));
#7766=CARTESIAN_POINT('',(1.375,0.4,55.));
#7767=CARTESIAN_POINT('Origin',(1.6,0.2,55.));
#7768=CARTESIAN_POINT('Origin',(1.6,0.4,115.));
#7769=CARTESIAN_POINT('',(1.375,0.4,115.));
#7770=CARTESIAN_POINT('Origin',(1.6,0.4,115.));
#7771=CARTESIAN_POINT('',(1.375,0.2,115.));
#7772=CARTESIAN_POINT('',(1.375,0.4,115.));
#7773=CARTESIAN_POINT('Origin',(1.6,0.2,115.));
#7774=CARTESIAN_POINT('Origin',(0.,0.,113.323333333333));
#7775=CARTESIAN_POINT('',(0.369323706252388,0.2,113.323333333333));
#7776=CARTESIAN_POINT('',(0.25,0.2,113.323333333333));
#7777=CARTESIAN_POINT('',(0.125,0.2,113.323333333333));
#7778=CARTESIAN_POINT('',(0.25,0.337490740613724,113.323333333333));
#7779=CARTESIAN_POINT('Origin',(0.,0.,113.323333333333));
#7780=CARTESIAN_POINT('',(0.25,0.2,113.323333333333));
#7781=CARTESIAN_POINT('Origin',(0.,0.,113.323333333333));
#7782=CARTESIAN_POINT('',(0.369323706252388,0.2,170.));
#7783=CARTESIAN_POINT('',(0.369323706252388,0.2,113.323333333333));
#7784=CARTESIAN_POINT('',(0.25,0.337490740613724,170.));
#7785=CARTESIAN_POINT('Origin',(0.,0.,170.));
#7786=CARTESIAN_POINT('',(0.25,0.337490740613724,113.323333333333));
#7787=CARTESIAN_POINT('Origin',(0.25,0.2,0.));
#7788=CARTESIAN_POINT('',(0.25,0.2,113.313333333333));
#7789=CARTESIAN_POINT('',(0.25,0.2,0.));
#7790=CARTESIAN_POINT('',(0.346410161513776,0.2,113.313333333333));
#7791=CARTESIAN_POINT('',(0.125,0.2,113.313333333333));
#7792=CARTESIAN_POINT('',(0.346410161513776,0.2,56.6866666666667));
#7793=CARTESIAN_POINT('',(0.346410161513776,0.2,56.6866666666667));
#7794=CARTESIAN_POINT('',(0.25,0.2,56.6866666666667));
#7795=CARTESIAN_POINT('',(0.125,0.2,56.6866666666667));
#7796=CARTESIAN_POINT('',(0.25,0.2,56.6766666666667));
#7797=CARTESIAN_POINT('',(0.25,0.2,0.));
#7798=CARTESIAN_POINT('',(0.369323706252388,0.2,56.6766666666667));
#7799=CARTESIAN_POINT('',(0.125,0.2,56.6766666666667));
#7800=CARTESIAN_POINT('',(0.369323706252388,0.2,0.));
#7801=CARTESIAN_POINT('',(0.369323706252388,0.2,0.));
#7802=CARTESIAN_POINT('',(2.7,0.2,0.));
#7803=CARTESIAN_POINT('',(0.25,0.2,0.));
#7804=CARTESIAN_POINT('',(2.7,0.2,170.));
#7805=CARTESIAN_POINT('',(2.7,0.2,0.));
#7806=CARTESIAN_POINT('',(0.25,0.2,170.));
#7807=CARTESIAN_POINT('Origin',(0.25,0.4,0.));
#7808=CARTESIAN_POINT('',(0.25,0.4,170.));
#7809=CARTESIAN_POINT('',(0.25,0.4,170.));
#7810=CARTESIAN_POINT('',(0.25,0.4,0.));
#7811=CARTESIAN_POINT('',(0.25,0.4,0.));
#7812=CARTESIAN_POINT('',(0.25,0.337490740613724,0.));
#7813=CARTESIAN_POINT('',(0.25,0.4,0.));
#7814=CARTESIAN_POINT('',(0.25,0.337490740613724,56.6766666666667));
#7815=CARTESIAN_POINT('',(0.25,0.337490740613724,0.));
#7816=CARTESIAN_POINT('',(0.25,0.2,56.6766666666667));
#7817=CARTESIAN_POINT('',(0.25,0.31224989991992,56.6866666666667));
#7818=CARTESIAN_POINT('',(0.25,0.2,56.6866666666667));
#7819=CARTESIAN_POINT('',(0.25,0.31224989991992,113.313333333333));
#7820=CARTESIAN_POINT('',(0.25,0.31224989991992,56.6866666666667));
#7821=CARTESIAN_POINT('',(0.25,0.2,113.313333333333));
#7822=CARTESIAN_POINT('Origin',(0.,0.,0.));
#7823=CARTESIAN_POINT('Origin',(0.,0.,56.6766666666667));
#7824=CARTESIAN_POINT('Origin',(0.,0.,0.));
#7825=CARTESIAN_POINT('Origin',(0.,0.,56.6766666666667));
#7826=CARTESIAN_POINT('Origin',(1.475,0.3,0.));
#7827=CARTESIAN_POINT('',(2.7,0.4,0.));
#7828=CARTESIAN_POINT('',(2.7,0.4,0.));
#7829=CARTESIAN_POINT('',(2.7,0.2,0.));
#7830=CARTESIAN_POINT('Origin',(0.,0.,113.313333333333));
#7831=CARTESIAN_POINT('Origin',(0.,0.,113.313333333333));
#7832=CARTESIAN_POINT('',(-0.22,-2.69422295812418E-17,113.313333333333));
#7833=CARTESIAN_POINT('Origin',(0.,0.,113.313333333333));
#7834=CARTESIAN_POINT('Origin',(0.,0.,56.6866666666667));
#7835=CARTESIAN_POINT('',(-0.22,-2.69422295812418E-17,56.6866666666667));
#7836=CARTESIAN_POINT('Origin',(0.,0.,56.6866666666667));
#7837=CARTESIAN_POINT('',(-0.22,-2.69422295812418E-17,56.6866666666667));
#7838=CARTESIAN_POINT('Origin',(0.,0.,56.6866666666667));
#7839=CARTESIAN_POINT('Origin',(0.,0.,56.6866666666667));
#7840=CARTESIAN_POINT('Origin',(0.,0.,56.6866666666667));
#7841=CARTESIAN_POINT('Origin',(2.7,0.4,0.));
#7842=CARTESIAN_POINT('',(2.7,0.4,170.));
#7843=CARTESIAN_POINT('',(2.7,0.4,170.));
#7844=CARTESIAN_POINT('',(2.7,0.4,0.));
#7845=CARTESIAN_POINT('Origin',(2.7,0.2,0.));
#7846=CARTESIAN_POINT('',(2.7,0.2,170.));
#7847=CARTESIAN_POINT('Origin',(1.475,0.3,170.));
#7848=CARTESIAN_POINT('',(0.,0.,0.));
#7849=CARTESIAN_POINT('Origin',(0.,0.,170.));
#7850=CARTESIAN_POINT('',(-0.3,-3.67394039744206E-17,170.));
#7851=CARTESIAN_POINT('Origin',(0.,0.,170.));
#7852=CARTESIAN_POINT('',(-0.2,2.44929359829471E-17,170.));
#7853=CARTESIAN_POINT('Origin',(0.,0.,170.));
#7854=CARTESIAN_POINT('Origin',(0.,0.,170.));
#7855=CARTESIAN_POINT('',(-0.3,-3.67394039744206E-17,170.2));
#7856=CARTESIAN_POINT('Origin',(0.,0.,170.2));
#7857=CARTESIAN_POINT('',(-0.3,-3.67394039744206E-17,170.));
#7858=CARTESIAN_POINT('Origin',(0.,0.,0.));
#7859=CARTESIAN_POINT('',(-0.35,-4.28626379701574E-17,0.));
#7860=CARTESIAN_POINT('Origin',(0.,0.,0.));
#7861=CARTESIAN_POINT('',(-0.2,-2.44929359829471E-17,0.));
#7862=CARTESIAN_POINT('Origin',(0.,0.,0.));
#7863=CARTESIAN_POINT('Origin',(0.,0.,-0.2));
#7864=CARTESIAN_POINT('',(-0.35,-4.28626379701574E-17,-0.2));
#7865=CARTESIAN_POINT('',(-0.35,-4.28626379701574E-17,-0.2));
#7866=CARTESIAN_POINT('Origin',(0.,0.,-0.2));
#7867=CARTESIAN_POINT('Origin',(0.,0.,-0.2));
#7868=CARTESIAN_POINT('Origin',(0.,0.,0.));
#7869=CARTESIAN_POINT('',(-0.2,-2.44929359829471E-17,0.));
#7870=CARTESIAN_POINT('Origin',(0.,0.,170.2));
#7871=CARTESIAN_POINT('',(0.,0.,0.));
#7872=CARTESIAN_POINT('Origin',(57.36,0.6,0.));
#7873=CARTESIAN_POINT('',(57.36,0.6,0.));
#7874=CARTESIAN_POINT('',(0.,0.6,0.));
#7875=CARTESIAN_POINT('',(57.36,0.6,0.));
#7876=CARTESIAN_POINT('',(0.,0.6,177.36));
#7877=CARTESIAN_POINT('',(0.,0.6,0.));
#7878=CARTESIAN_POINT('',(57.36,0.6,177.36));
#7879=CARTESIAN_POINT('',(57.36,0.6,177.36));
#7880=CARTESIAN_POINT('',(57.36,0.6,0.));
#7881=CARTESIAN_POINT('Origin',(57.36,0.,0.));
#7882=CARTESIAN_POINT('',(57.36,0.,0.));
#7883=CARTESIAN_POINT('',(57.36,0.,0.));
#7884=CARTESIAN_POINT('',(57.36,0.,177.36));
#7885=CARTESIAN_POINT('',(57.36,0.,177.36));
#7886=CARTESIAN_POINT('',(57.36,0.,0.));
#7887=CARTESIAN_POINT('Origin',(0.,0.,0.));
#7888=CARTESIAN_POINT('',(0.,0.,0.));
#7889=CARTESIAN_POINT('',(0.,0.,0.));
#7890=CARTESIAN_POINT('',(0.,0.,177.36));
#7891=CARTESIAN_POINT('',(0.,0.,177.36));
#7892=CARTESIAN_POINT('',(0.,0.,0.));
#7893=CARTESIAN_POINT('Origin',(0.,0.6,0.));
#7894=CARTESIAN_POINT('',(0.,0.6,0.));
#7895=CARTESIAN_POINT('',(0.,0.6,177.36));
#7896=CARTESIAN_POINT('Origin',(28.68,0.3,177.36));
#7897=CARTESIAN_POINT('Origin',(28.68,0.3,0.));
#7898=CARTESIAN_POINT('',(0.,0.,0.));
#7899=CARTESIAN_POINT('Origin',(0.,51.,60.));
#7900=CARTESIAN_POINT('',(0.,51.,60.41));
#7901=CARTESIAN_POINT('Origin',(0.,51.,60.));
#7902=CARTESIAN_POINT('',(1.5,51.,60.41));
#7903=CARTESIAN_POINT('',(0.,51.,60.41));
#7904=CARTESIAN_POINT('Origin',(1.5,51.,60.));
#7905=CARTESIAN_POINT('Origin',(1.5,51.,60.));
#7906=CARTESIAN_POINT('Origin',(0.,9.,120.));
#7907=CARTESIAN_POINT('',(0.,9.,120.41));
#7908=CARTESIAN_POINT('Origin',(0.,9.,120.));
#7909=CARTESIAN_POINT('',(1.5,9.,120.41));
#7910=CARTESIAN_POINT('',(0.,9.,120.41));
#7911=CARTESIAN_POINT('Origin',(1.5,9.,120.));
#7912=CARTESIAN_POINT('Origin',(1.5,9.,120.));
#7913=CARTESIAN_POINT('Origin',(0.,9.,60.));
#7914=CARTESIAN_POINT('',(0.,9.,60.41));
#7915=CARTESIAN_POINT('Origin',(0.,9.,60.));
#7916=CARTESIAN_POINT('',(1.5,9.,60.41));
#7917=CARTESIAN_POINT('',(0.,9.,60.41));
#7918=CARTESIAN_POINT('Origin',(1.5,9.,60.));
#7919=CARTESIAN_POINT('Origin',(1.5,9.,60.));
#7920=CARTESIAN_POINT('Origin',(0.,51.,120.));
#7921=CARTESIAN_POINT('',(0.,51.,120.41));
#7922=CARTESIAN_POINT('Origin',(0.,51.,120.));
#7923=CARTESIAN_POINT('',(1.5,51.,120.41));
#7924=CARTESIAN_POINT('',(0.,51.,120.41));
#7925=CARTESIAN_POINT('Origin',(1.5,51.,120.));
#7926=CARTESIAN_POINT('Origin',(1.5,51.,120.));
#7927=CARTESIAN_POINT('Origin',(1.8,1.6,60.));
#7928=CARTESIAN_POINT('',(1.8,1.6,60.225));
#7929=CARTESIAN_POINT('Origin',(1.8,1.6,60.));
#7930=CARTESIAN_POINT('',(0.,1.6,60.225));
#7931=CARTESIAN_POINT('',(1.8,1.6,60.225));
#7932=CARTESIAN_POINT('Origin',(0.,1.6,60.));
#7933=CARTESIAN_POINT('Origin',(1.8,1.6,120.));
#7934=CARTESIAN_POINT('',(1.8,1.6,120.225));
#7935=CARTESIAN_POINT('Origin',(1.8,1.6,120.));
#7936=CARTESIAN_POINT('',(0.,1.6,120.225));
#7937=CARTESIAN_POINT('',(1.8,1.6,120.225));
#7938=CARTESIAN_POINT('Origin',(0.,1.6,120.));
#7939=CARTESIAN_POINT('Origin',(1.81,58.82,0.));
#7940=CARTESIAN_POINT('',(1.3,58.82,134.08));
#7941=CARTESIAN_POINT('',(1.8,58.82,134.08));
#7942=CARTESIAN_POINT('',(1.6825,58.82,134.08));
#7943=CARTESIAN_POINT('',(1.3,58.82,90.92));
#7944=CARTESIAN_POINT('',(1.3,58.82,0.));
#7945=CARTESIAN_POINT('',(1.8,58.82,90.92));
#7946=CARTESIAN_POINT('',(1.6825,58.82,90.92));
#7947=CARTESIAN_POINT('',(1.8,58.82,0.));
#7948=CARTESIAN_POINT('Origin',(1.81,58.82,0.));
#7949=CARTESIAN_POINT('',(1.3,58.82,89.08));
#7950=CARTESIAN_POINT('',(1.8,58.82,89.08));
#7951=CARTESIAN_POINT('',(1.6825,58.82,89.08));
#7952=CARTESIAN_POINT('',(1.3,58.82,45.92));
#7953=CARTESIAN_POINT('',(1.3,58.82,0.));
#7954=CARTESIAN_POINT('',(1.8,58.82,45.92));
#7955=CARTESIAN_POINT('',(1.6825,58.82,45.92));
#7956=CARTESIAN_POINT('',(1.8,58.82,0.));
#7957=CARTESIAN_POINT('Origin',(1.81,58.82,0.));
#7958=CARTESIAN_POINT('',(1.3,58.82,44.08));
#7959=CARTESIAN_POINT('',(1.8,58.82,44.08));
#7960=CARTESIAN_POINT('',(1.6825,58.82,44.08));
#7961=CARTESIAN_POINT('',(1.3,58.82,1.82));
#7962=CARTESIAN_POINT('',(1.3,58.82,0.));
#7963=CARTESIAN_POINT('',(1.8,58.82,1.82));
#7964=CARTESIAN_POINT('',(1.6825,58.82,1.82));
#7965=CARTESIAN_POINT('',(1.8,58.82,0.));
#7966=CARTESIAN_POINT('Origin',(1.81,58.82,0.));
#7967=CARTESIAN_POINT('',(1.3,58.82,178.18));
#7968=CARTESIAN_POINT('',(1.8,58.82,178.18));
#7969=CARTESIAN_POINT('',(1.6825,58.82,178.18));
#7970=CARTESIAN_POINT('',(1.3,58.82,135.92));
#7971=CARTESIAN_POINT('',(1.3,58.82,0.));
#7972=CARTESIAN_POINT('',(1.8,58.82,135.92));
#7973=CARTESIAN_POINT('',(1.6825,58.82,135.92));
#7974=CARTESIAN_POINT('',(1.8,58.82,0.));
#7975=CARTESIAN_POINT('Origin',(1.3,58.18,0.));
#7976=CARTESIAN_POINT('',(1.8,58.18,44.08));
#7977=CARTESIAN_POINT('',(1.3,58.18,44.08));
#7978=CARTESIAN_POINT('',(1.4275,58.18,44.08));
#7979=CARTESIAN_POINT('',(1.8,58.18,1.82));
#7980=CARTESIAN_POINT('',(1.8,58.18,0.));
#7981=CARTESIAN_POINT('',(1.3,58.18,1.82));
#7982=CARTESIAN_POINT('',(1.4275,58.18,1.82));
#7983=CARTESIAN_POINT('',(1.3,58.18,0.));
#7984=CARTESIAN_POINT('Origin',(1.3,58.18,0.));
#7985=CARTESIAN_POINT('',(1.8,58.18,89.08));
#7986=CARTESIAN_POINT('',(1.3,58.18,89.08));
#7987=CARTESIAN_POINT('',(1.4275,58.18,89.08));
#7988=CARTESIAN_POINT('',(1.8,58.18,45.92));
#7989=CARTESIAN_POINT('',(1.8,58.18,0.));
#7990=CARTESIAN_POINT('',(1.3,58.18,45.92));
#7991=CARTESIAN_POINT('',(1.4275,58.18,45.92));
#7992=CARTESIAN_POINT('',(1.3,58.18,0.));
#7993=CARTESIAN_POINT('Origin',(1.3,58.18,0.));
#7994=CARTESIAN_POINT('',(1.8,58.18,134.08));
#7995=CARTESIAN_POINT('',(1.3,58.18,134.08));
#7996=CARTESIAN_POINT('',(1.4275,58.18,134.08));
#7997=CARTESIAN_POINT('',(1.8,58.18,90.92));
#7998=CARTESIAN_POINT('',(1.8,58.18,0.));
#7999=CARTESIAN_POINT('',(1.3,58.18,90.92));
#8000=CARTESIAN_POINT('',(1.4275,58.18,90.92));
#8001=CARTESIAN_POINT('',(1.3,58.18,0.));
#8002=CARTESIAN_POINT('Origin',(1.3,58.18,0.));
#8003=CARTESIAN_POINT('',(1.8,58.18,178.18));
#8004=CARTESIAN_POINT('',(1.3,58.18,178.18));
#8005=CARTESIAN_POINT('',(1.4275,58.18,178.18));
#8006=CARTESIAN_POINT('',(1.8,58.18,135.92));
#8007=CARTESIAN_POINT('',(1.8,58.18,0.));
#8008=CARTESIAN_POINT('',(1.3,58.18,135.92));
#8009=CARTESIAN_POINT('',(1.4275,58.18,135.92));
#8010=CARTESIAN_POINT('',(1.3,58.18,0.));
#8011=CARTESIAN_POINT('Origin',(1.3,60.,178.18));
#8012=CARTESIAN_POINT('',(1.3,60.,178.18));
#8013=CARTESIAN_POINT('',(1.3,60.,178.18));
#8014=CARTESIAN_POINT('',(1.3,60.,180.));
#8015=CARTESIAN_POINT('',(1.3,60.,89.09));
#8016=CARTESIAN_POINT('',(1.3,0.,180.));
#8017=CARTESIAN_POINT('',(1.3,45.,180.));
#8018=CARTESIAN_POINT('',(1.3,0.,178.18));
#8019=CARTESIAN_POINT('',(1.3,0.,89.09));
#8020=CARTESIAN_POINT('',(1.3,60.,178.18));
#8021=CARTESIAN_POINT('',(1.3,0.,135.92));
#8022=CARTESIAN_POINT('',(1.3,60.,135.92));
#8023=CARTESIAN_POINT('',(1.3,0.,134.08));
#8024=CARTESIAN_POINT('',(1.3,0.,67.04));
#8025=CARTESIAN_POINT('',(1.3,60.,134.08));
#8026=CARTESIAN_POINT('',(1.3,0.,90.92));
#8027=CARTESIAN_POINT('',(1.3,60.,90.92));
#8028=CARTESIAN_POINT('',(1.3,0.,89.08));
#8029=CARTESIAN_POINT('',(1.3,0.,44.54));
#8030=CARTESIAN_POINT('',(1.3,60.,89.08));
#8031=CARTESIAN_POINT('',(1.3,0.,45.92));
#8032=CARTESIAN_POINT('',(1.3,60.,45.92));
#8033=CARTESIAN_POINT('',(1.3,0.,44.08));
#8034=CARTESIAN_POINT('',(1.3,0.,22.04));
#8035=CARTESIAN_POINT('',(1.3,60.,44.08));
#8036=CARTESIAN_POINT('',(1.3,0.,1.82));
#8037=CARTESIAN_POINT('',(1.3,60.,1.82));
#8038=CARTESIAN_POINT('',(1.3,0.,0.));
#8039=CARTESIAN_POINT('',(1.3,0.,0.));
#8040=CARTESIAN_POINT('',(1.3,60.,0.));
#8041=CARTESIAN_POINT('',(1.3,45.,0.));
#8042=CARTESIAN_POINT('',(1.3,60.,1.82));
#8043=CARTESIAN_POINT('',(1.3,60.,0.));
#8044=CARTESIAN_POINT('',(1.3,60.,1.82));
#8045=CARTESIAN_POINT('',(1.3,60.,44.08));
#8046=CARTESIAN_POINT('',(1.3,60.,44.08));
#8047=CARTESIAN_POINT('',(1.3,60.,45.92));
#8048=CARTESIAN_POINT('',(1.3,60.,22.04));
#8049=CARTESIAN_POINT('',(1.3,60.,45.92));
#8050=CARTESIAN_POINT('',(1.3,60.,89.08));
#8051=CARTESIAN_POINT('',(1.3,60.,89.08));
#8052=CARTESIAN_POINT('',(1.3,60.,90.92));
#8053=CARTESIAN_POINT('',(1.3,60.,44.54));
#8054=CARTESIAN_POINT('',(1.3,60.,90.92));
#8055=CARTESIAN_POINT('',(1.3,60.,134.08));
#8056=CARTESIAN_POINT('',(1.3,60.,134.08));
#8057=CARTESIAN_POINT('',(1.3,60.,135.92));
#8058=CARTESIAN_POINT('',(1.3,60.,67.04));
#8059=CARTESIAN_POINT('',(1.3,60.,135.92));
#8060=CARTESIAN_POINT('Origin',(1.555,30.,178.18));
#8061=CARTESIAN_POINT('',(1.8,0.,178.18));
#8062=CARTESIAN_POINT('',(0.7775,0.,178.18));
#8063=CARTESIAN_POINT('',(1.8,15.,178.18));
#8064=CARTESIAN_POINT('Origin',(1.555,30.,178.18));
#8065=CARTESIAN_POINT('',(1.8,60.,178.18));
#8066=CARTESIAN_POINT('',(1.8,15.,178.18));
#8067=CARTESIAN_POINT('',(1.6775,60.,178.18));
#8068=CARTESIAN_POINT('Origin',(1.8,0.,0.));
#8069=CARTESIAN_POINT('',(1.8,0.,135.92));
#8070=CARTESIAN_POINT('',(1.8,0.,0.));
#8071=CARTESIAN_POINT('',(1.8,15.,135.92));
#8072=CARTESIAN_POINT('Origin',(1.8,0.,0.));
#8073=CARTESIAN_POINT('',(1.8,60.,135.92));
#8074=CARTESIAN_POINT('',(1.8,15.,135.92));
#8075=CARTESIAN_POINT('',(1.8,60.,0.));
#8076=CARTESIAN_POINT('Origin',(1.555,30.,135.92));
#8077=CARTESIAN_POINT('',(0.7775,0.,135.92));
#8078=CARTESIAN_POINT('Origin',(1.555,30.,135.92));
#8079=CARTESIAN_POINT('',(1.6775,60.,135.92));
#8080=CARTESIAN_POINT('Origin',(1.555,30.,134.08));
#8081=CARTESIAN_POINT('',(1.8,0.,134.08));
#8082=CARTESIAN_POINT('',(0.7775,0.,134.08));
#8083=CARTESIAN_POINT('',(1.8,15.,134.08));
#8084=CARTESIAN_POINT('Origin',(1.555,30.,134.08));
#8085=CARTESIAN_POINT('',(1.8,60.,134.08));
#8086=CARTESIAN_POINT('',(1.8,15.,134.08));
#8087=CARTESIAN_POINT('',(1.6775,60.,134.08));
#8088=CARTESIAN_POINT('Origin',(1.8,0.,0.));
#8089=CARTESIAN_POINT('',(1.8,0.,90.92));
#8090=CARTESIAN_POINT('',(1.8,0.,0.));
#8091=CARTESIAN_POINT('',(1.8,15.,90.92));
#8092=CARTESIAN_POINT('Origin',(1.8,0.,0.));
#8093=CARTESIAN_POINT('',(1.8,60.,90.92));
#8094=CARTESIAN_POINT('',(1.8,15.,90.92));
#8095=CARTESIAN_POINT('',(1.8,60.,0.));
#8096=CARTESIAN_POINT('Origin',(1.555,30.,90.92));
#8097=CARTESIAN_POINT('',(0.7775,0.,90.92));
#8098=CARTESIAN_POINT('Origin',(1.555,30.,90.92));
#8099=CARTESIAN_POINT('',(1.6775,60.,90.92));
#8100=CARTESIAN_POINT('Origin',(1.555,30.,89.08));
#8101=CARTESIAN_POINT('',(1.8,0.,89.08));
#8102=CARTESIAN_POINT('',(0.7775,0.,89.08));
#8103=CARTESIAN_POINT('',(1.8,15.,89.08));
#8104=CARTESIAN_POINT('Origin',(1.555,30.,89.08));
#8105=CARTESIAN_POINT('',(1.8,60.,89.08));
#8106=CARTESIAN_POINT('',(1.8,15.,89.08));
#8107=CARTESIAN_POINT('',(1.6775,60.,89.08));
#8108=CARTESIAN_POINT('Origin',(1.8,0.,0.));
#8109=CARTESIAN_POINT('',(1.8,0.,45.92));
#8110=CARTESIAN_POINT('',(1.8,0.,0.));
#8111=CARTESIAN_POINT('',(1.8,15.,45.92));
#8112=CARTESIAN_POINT('Origin',(1.8,0.,0.));
#8113=CARTESIAN_POINT('',(1.8,60.,45.92));
#8114=CARTESIAN_POINT('',(1.8,15.,45.92));
#8115=CARTESIAN_POINT('',(1.8,60.,0.));
#8116=CARTESIAN_POINT('Origin',(1.555,30.,45.92));
#8117=CARTESIAN_POINT('',(0.7775,0.,45.92));
#8118=CARTESIAN_POINT('Origin',(1.555,30.,45.92));
#8119=CARTESIAN_POINT('',(1.6775,60.,45.92));
#8120=CARTESIAN_POINT('Origin',(1.555,30.,44.08));
#8121=CARTESIAN_POINT('',(1.8,0.,44.08));
#8122=CARTESIAN_POINT('',(0.7775,0.,44.08));
#8123=CARTESIAN_POINT('',(1.8,15.,44.08));
#8124=CARTESIAN_POINT('Origin',(1.555,30.,44.08));
#8125=CARTESIAN_POINT('',(1.8,60.,44.08));
#8126=CARTESIAN_POINT('',(1.8,15.,44.08));
#8127=CARTESIAN_POINT('',(1.6775,60.,44.08));
#8128=CARTESIAN_POINT('Origin',(1.8,0.,0.));
#8129=CARTESIAN_POINT('',(1.8,0.,1.82));
#8130=CARTESIAN_POINT('',(1.8,0.,0.));
#8131=CARTESIAN_POINT('',(1.8,15.,1.82));
#8132=CARTESIAN_POINT('Origin',(1.8,0.,0.));
#8133=CARTESIAN_POINT('',(1.8,60.,1.82));
#8134=CARTESIAN_POINT('',(1.8,15.,1.82));
#8135=CARTESIAN_POINT('',(1.8,60.,0.));
#8136=CARTESIAN_POINT('Origin',(1.555,30.,1.82));
#8137=CARTESIAN_POINT('',(0.7775,0.,1.82));
#8138=CARTESIAN_POINT('Origin',(1.555,30.,1.82));
#8139=CARTESIAN_POINT('',(1.6775,60.,1.82));
#8140=CARTESIAN_POINT('Origin',(1.8,60.,0.));
#8141=CARTESIAN_POINT('',(0.,60.,0.));
#8142=CARTESIAN_POINT('',(1.8,60.,0.));
#8143=CARTESIAN_POINT('',(0.,60.,180.));
#8144=CARTESIAN_POINT('',(0.,60.,0.));
#8145=CARTESIAN_POINT('',(1.8,60.,180.));
#8146=CARTESIAN_POINT('Origin',(0.9,30.,0.));
#8147=CARTESIAN_POINT('',(0.,0.,0.));
#8148=CARTESIAN_POINT('',(0.,0.,0.));
#8149=CARTESIAN_POINT('',(0.,60.,0.));
#8150=CARTESIAN_POINT('Origin',(0.,0.,0.));
#8151=CARTESIAN_POINT('',(0.,0.,180.));
#8152=CARTESIAN_POINT('',(0.,0.,180.));
#8153=CARTESIAN_POINT('',(0.,0.,0.));
#8154=CARTESIAN_POINT('Origin',(0.,60.,0.));
#8155=CARTESIAN_POINT('',(0.,60.,180.));
#8156=CARTESIAN_POINT('Origin',(0.9,30.,180.));
#8157=CARTESIAN_POINT('',(0.,0.,0.));
#8158=CARTESIAN_POINT('Origin',(0.,58.18,1.3));
#8159=CARTESIAN_POINT('',(77.36,58.18,1.8));
#8160=CARTESIAN_POINT('',(0.,58.18,1.8));
#8161=CARTESIAN_POINT('',(19.34,58.18,1.8));
#8162=CARTESIAN_POINT('',(77.36,58.18,1.3));
#8163=CARTESIAN_POINT('',(77.36,58.18,0.65));
#8164=CARTESIAN_POINT('',(0.,58.18,1.3));
#8165=CARTESIAN_POINT('',(0.,58.18,1.3));
#8166=CARTESIAN_POINT('',(0.,58.18,0.65));
#8167=CARTESIAN_POINT('Origin',(77.36,58.82,1.3));
#8168=CARTESIAN_POINT('',(0.,58.82,1.8));
#8169=CARTESIAN_POINT('',(77.36,58.82,1.8));
#8170=CARTESIAN_POINT('',(58.02,58.82,1.8));
#8171=CARTESIAN_POINT('',(0.,58.82,1.3));
#8172=CARTESIAN_POINT('',(0.,58.82,0.65));
#8173=CARTESIAN_POINT('',(77.36,58.82,1.3));
#8174=CARTESIAN_POINT('',(77.36,58.82,1.3));
#8175=CARTESIAN_POINT('',(77.36,58.82,0.65));
#8176=CARTESIAN_POINT('Origin',(38.68,58.5,1.3));
#8177=CARTESIAN_POINT('',(0.,59.25,1.3));
#8178=CARTESIAN_POINT('',(77.36,29.25,1.3));
#8179=CARTESIAN_POINT('Origin',(77.36,0.,0.));
#8180=CARTESIAN_POINT('',(77.36,0.,1.8));
#8181=CARTESIAN_POINT('',(77.36,0.,1.8));
#8182=CARTESIAN_POINT('',(77.36,0.,0.));
#8183=CARTESIAN_POINT('',(77.36,0.,0.));
#8184=CARTESIAN_POINT('',(77.36,60.,0.));
#8185=CARTESIAN_POINT('',(77.36,0.,0.));
#8186=CARTESIAN_POINT('',(77.36,60.,1.8));
#8187=CARTESIAN_POINT('',(77.36,60.,0.));
#8188=CARTESIAN_POINT('',(77.36,0.,1.8));
#8189=CARTESIAN_POINT('Origin',(38.68,30.,1.8));
#8190=CARTESIAN_POINT('',(0.,0.,1.8));
#8191=CARTESIAN_POINT('',(0.,60.,1.8));
#8192=CARTESIAN_POINT('',(0.,0.,1.8));
#8193=CARTESIAN_POINT('Origin',(77.36,60.,0.));
#8194=CARTESIAN_POINT('',(0.,60.,0.));
#8195=CARTESIAN_POINT('',(77.36,60.,0.));
#8196=CARTESIAN_POINT('',(0.,60.,1.8));
#8197=CARTESIAN_POINT('',(0.,60.,0.));
#8198=CARTESIAN_POINT('',(77.36,60.,1.8));
#8199=CARTESIAN_POINT('Origin',(0.,0.,0.));
#8200=CARTESIAN_POINT('',(0.,0.,0.));
#8201=CARTESIAN_POINT('',(0.,0.,0.));
#8202=CARTESIAN_POINT('',(0.,0.,0.));
#8203=CARTESIAN_POINT('Origin',(0.,60.,0.));
#8204=CARTESIAN_POINT('',(0.,60.,1.8));
#8205=CARTESIAN_POINT('',(0.,60.,0.));
#8206=CARTESIAN_POINT('Origin',(38.68,30.,1.8));
#8207=CARTESIAN_POINT('Origin',(38.68,30.,0.));
#8208=CARTESIAN_POINT('',(0.,0.,0.));
#8209=CARTESIAN_POINT('Origin',(0.88,3.,0.));
#8210=CARTESIAN_POINT('',(0.88,3.,0.));
#8211=CARTESIAN_POINT('',(0.,3.,0.));
#8212=CARTESIAN_POINT('',(19.78,3.,0.));
#8213=CARTESIAN_POINT('',(0.88,3.,1.8));
#8214=CARTESIAN_POINT('',(0.88,3.,0.));
#8215=CARTESIAN_POINT('',(0.,3.,1.8));
#8216=CARTESIAN_POINT('',(19.78,3.,1.8));
#8217=CARTESIAN_POINT('',(0.,3.,0.));
#8218=CARTESIAN_POINT('Origin',(0.88,0.6,0.));
#8219=CARTESIAN_POINT('',(0.88,0.6,0.));
#8220=CARTESIAN_POINT('',(0.880000000000003,14.85,0.));
#8221=CARTESIAN_POINT('',(0.88,0.6,1.8));
#8222=CARTESIAN_POINT('',(0.88,0.6,0.));
#8223=CARTESIAN_POINT('',(0.880000000000003,14.85,1.8));
#8224=CARTESIAN_POINT('Origin',(0.,57.6,0.));
#8225=CARTESIAN_POINT('',(0.,57.6,1.8));
#8226=CARTESIAN_POINT('',(0.,57.6,1.8));
#8227=CARTESIAN_POINT('',(0.,57.6,0.));
#8228=CARTESIAN_POINT('',(0.,57.6,0.));
#8229=CARTESIAN_POINT('',(0.,57.6,0.));
#8230=CARTESIAN_POINT('Origin',(0.,0.6,0.));
#8231=CARTESIAN_POINT('',(77.36,0.6,0.));
#8232=CARTESIAN_POINT('',(0.,0.6,0.));
#8233=CARTESIAN_POINT('',(77.36,0.600000000000001,1.8));
#8234=CARTESIAN_POINT('',(77.36,0.6,0.));
#8235=CARTESIAN_POINT('',(0.,0.6,1.8));
#8236=CARTESIAN_POINT('Origin',(77.36,57.6,0.));
#8237=CARTESIAN_POINT('',(77.36,57.6,0.));
#8238=CARTESIAN_POINT('',(77.36,57.6,0.));
#8239=CARTESIAN_POINT('',(77.36,57.6,1.8));
#8240=CARTESIAN_POINT('',(77.36,57.6,1.8));
#8241=CARTESIAN_POINT('',(77.36,57.6,0.));
#8242=CARTESIAN_POINT('Origin',(77.36,0.6,0.));
#8243=CARTESIAN_POINT('',(77.36,0.6,0.));
#8244=CARTESIAN_POINT('',(77.36,0.6,1.8));
#8245=CARTESIAN_POINT('Origin',(38.68,29.1,1.8));
#8246=CARTESIAN_POINT('Origin',(38.68,29.1,0.));
#8247=CARTESIAN_POINT('',(0.,0.,0.));
#8248=CARTESIAN_POINT('Origin',(0.,0.,-0.129405622560373));
#8249=CARTESIAN_POINT('',(-0.0636885943104742,0.141913936788308,0.0466443258702189));
#8250=CARTESIAN_POINT('',(-0.0636886258329924,0.141913922641526,0.0327905057321709));
#8251=CARTESIAN_POINT('',(-0.0636886258329924,0.141913922641526,-0.129405622560373));
#8252=CARTESIAN_POINT('',(-0.0887899522119582,-0.127719015366539,5.89805981832114E-17));
#8253=CARTESIAN_POINT('Ctrl Pts',(-0.0636885943104762,0.141913936788307,
0.046644325870219));
#8254=CARTESIAN_POINT('Ctrl Pts',(-0.0568706875042543,0.144973698996693,
0.0460674767969737));
#8255=CARTESIAN_POINT('Ctrl Pts',(-0.0498372314917207,0.147539905386712,
0.0454841194495339));
#8256=CARTESIAN_POINT('Ctrl Pts',(-0.0413488363880294,0.149959613661576,
0.0448074822562266));
#8257=CARTESIAN_POINT('Ctrl Pts',(-0.0400504322490268,0.150311593213423,
0.0447047356879959));
#8258=CARTESIAN_POINT('Ctrl Pts',(-0.0351567921767657,0.151570278540172,
0.0443206555495273));
#8259=CARTESIAN_POINT('Ctrl Pts',(-0.0315337316229291,0.152365280825276,
0.0440426625291857));
#8260=CARTESIAN_POINT('Ctrl Pts',(-0.0272702941063451,0.153142170667987,
0.0437254306071763));
#8261=CARTESIAN_POINT('Ctrl Pts',(-0.0266545361742012,0.153250543602531,
0.0436798532206328));
#8262=CARTESIAN_POINT('Ctrl Pts',(-0.0257193741345411,0.153409324446148,
0.0436110140072139));
#8263=CARTESIAN_POINT('Ctrl Pts',(-0.025400448699141,0.153462452228372,
0.0435876041457351));
#8264=CARTESIAN_POINT('Ctrl Pts',(-0.0248263790894383,0.153556244255832,
0.0435455891848324));
#8265=CARTESIAN_POINT('Ctrl Pts',(-0.0245712997285078,0.153597267167013,
0.0435269643365862));
#8266=CARTESIAN_POINT('Ctrl Pts',(-0.0240153248161858,0.153685260886435,
0.0434864647056545));
#8267=CARTESIAN_POINT('Ctrl Pts',(-0.0237143940782576,0.153731983521882,
0.0434646040589109));
#8268=CARTESIAN_POINT('Ctrl Pts',(-0.0228663427562202,0.153861102926211,
0.0434031639073866));
#8269=CARTESIAN_POINT('Ctrl Pts',(-0.0223189094731189,0.153941465919114,
0.0433636966382276));
#8270=CARTESIAN_POINT('Ctrl Pts',(-0.0189956769671261,0.154411215091918,
0.0431252161329079));
#8271=CARTESIAN_POINT('Ctrl Pts',(-0.0162099741319758,0.154728466865676,
0.0429299935086839));
#8272=CARTESIAN_POINT('Ctrl Pts',(0.00124647087156192,0.156239808213013,
0.0417272042602695));
#8273=CARTESIAN_POINT('Ctrl Pts',(0.0160171008148657,0.155421956466042,
0.0407933739561897));
#8274=CARTESIAN_POINT('Ctrl Pts',(0.0357815183452902,0.151476070394245,
0.0394361505080405));
#8275=CARTESIAN_POINT('Ctrl Pts',(0.0410491476710349,0.150134185089699,
0.0390643164092514));
#8276=CARTESIAN_POINT('Ctrl Pts',(0.0471445959753226,0.148236622932751,
0.0386166913475808));
#8277=CARTESIAN_POINT('Ctrl Pts',(0.048051184941417,0.147945236025617,0.0385496598891293));
#8278=CARTESIAN_POINT('Ctrl Pts',(0.0495196256884408,0.147458343246464,
0.0384403167580589));
#8279=CARTESIAN_POINT('Ctrl Pts',(0.0500831419342288,0.147267902808322,
0.0383981708569045));
#8280=CARTESIAN_POINT('Ctrl Pts',(0.0510844363447539,0.146923103460167,
0.0383229459682699));
#8281=CARTESIAN_POINT('Ctrl Pts',(0.0515226445693025,0.146770007341707,
0.038289908868643));
#8282=CARTESIAN_POINT('Ctrl Pts',(0.0524442928143612,0.146443376353324,
0.0382201774063333));
#8283=CARTESIAN_POINT('Ctrl Pts',(0.0529275707304974,0.146269404085352,
0.0381834689226026));
#8284=CARTESIAN_POINT('Ctrl Pts',(0.054202914277151,0.145803152834494,0.0380862108751925));
#8285=CARTESIAN_POINT('Ctrl Pts',(0.0549934676451898,0.145506816874414,
0.0380255273703788));
#8286=CARTESIAN_POINT('Ctrl Pts',(0.0586455792660056,0.144103822642237,
0.0377433135274135));
#8287=CARTESIAN_POINT('Ctrl Pts',(0.061476221414232,0.142919163836473,0.0375191986505781));
#8288=CARTESIAN_POINT('Ctrl Pts',(0.0774315956669701,0.135679934608843,
0.036223664566306));
#8289=CARTESIAN_POINT('Ctrl Pts',(0.0896951437222894,0.127903540121908,
0.0350913654422326));
#8290=CARTESIAN_POINT('Ctrl Pts',(0.105061585360943,0.114850011548946,0.0335398665531906));
#8291=CARTESIAN_POINT('Ctrl Pts',(0.109210447074238,0.110912385410338,0.0331057258356621));
#8292=CARTESIAN_POINT('Ctrl Pts',(0.113608594865368,0.106251440848463,0.0326360161345161));
#8293=CARTESIAN_POINT('Ctrl Pts',(0.114080237597373,0.105744886152826,0.032585516938738));
#8294=CARTESIAN_POINT('Ctrl Pts',(0.11477336334011,0.104990418825038,0.0325111330022006));
#8295=CARTESIAN_POINT('Ctrl Pts',(0.11499744915996,0.104744926701814,0.0324870581311852));
#8296=CARTESIAN_POINT('Ctrl Pts',(0.115393969483804,0.104307721624725,0.0324444129315734));
#8297=CARTESIAN_POINT('Ctrl Pts',(0.115566716870844,0.104116295264915,0.0324258190496426));
#8298=CARTESIAN_POINT('Ctrl Pts',(0.115935176202657,0.103705947972701,0.0323861283601505));
#8299=CARTESIAN_POINT('Ctrl Pts',(0.116130744868572,0.103486901713488,0.0323650423753064));
#8300=CARTESIAN_POINT('Ctrl Pts',(0.116667285269238,0.102882514513061,0.0323071358146115));
#8301=CARTESIAN_POINT('Ctrl Pts',(0.117006971450516,0.102496028688104,0.0322704106681944));
#8302=CARTESIAN_POINT('Ctrl Pts',(0.118829898217057,0.100401078566248,0.0320729299171071));
#8303=CARTESIAN_POINT('Ctrl Pts',(0.120277748849068,0.0986619778996509,
0.0319146577500692));
#8304=CARTESIAN_POINT('Ctrl Pts',(0.130437515508156,0.0859022380018732,
0.0307882427301412));
#8305=CARTESIAN_POINT('Ctrl Pts',(0.13765988439999,0.0737767332478561,0.0298957087520044));
#8306=CARTESIAN_POINT('Ctrl Pts',(0.145820741216985,0.0545757551836579,
0.0285039182135418));
#8307=CARTESIAN_POINT('Ctrl Pts',(0.148070190666843,0.0481393836691937,
0.0280415146952546));
#8308=CARTESIAN_POINT('Ctrl Pts',(0.150157317995708,0.0406150079109869,
0.0274945939492325));
#8309=CARTESIAN_POINT('Ctrl Pts',(0.150414869932778,0.0396505464712973,
0.0274243838614422));
#8310=CARTESIAN_POINT('Ctrl Pts',(0.150812075043454,0.0381035338796276,
0.0273115638515942));
#8311=CARTESIAN_POINT('Ctrl Pts',(0.150957680204654,0.0375225271263452,
0.0272691471353898));
#8312=CARTESIAN_POINT('Ctrl Pts',(0.151209698811495,0.0364916860455356,
0.0271938032756404));
#8313=CARTESIAN_POINT('Ctrl Pts',(0.151317470305596,0.0360421882925573,
0.0271609205117994));
#8314=CARTESIAN_POINT('Ctrl Pts',(0.151537300894291,0.035106942954735,0.0270924394105436));
#8315=CARTESIAN_POINT('Ctrl Pts',(0.151649031450763,0.0346211244076252,
0.0270568308784482));
#8316=CARTESIAN_POINT('Ctrl Pts',(0.151931981890424,0.0333631666977353,
0.0269645309005217));
#8317=CARTESIAN_POINT('Ctrl Pts',(0.152099649686521,0.0325902521513084,
0.0269077258040014));
#8318=CARTESIAN_POINT('Ctrl Pts',(0.152791815876093,0.0292777725240725,
0.0266638468777155));
#8319=CARTESIAN_POINT('Ctrl Pts',(0.153258629729472,0.0267267255748599,
0.0264749410446673));
#8320=CARTESIAN_POINT('Ctrl Pts',(0.15432002483048,0.0199775760837909,0.0259719459324084));
#8321=CARTESIAN_POINT('Ctrl Pts',(0.154807078932913,0.0157650218380878,
0.0256546958910069));
#8322=CARTESIAN_POINT('Ctrl Pts',(0.155990495241355,-0.000145061447557968,
0.0244446576807383));
#8323=CARTESIAN_POINT('Ctrl Pts',(0.155536710792408,-0.0118887813816597,
0.023524005431808));
#8324=CARTESIAN_POINT('Ctrl Pts',(0.153047927123364,-0.0281958210189353,
0.022260263756572));
#8325=CARTESIAN_POINT('Ctrl Pts',(0.152108692168808,-0.0328881310512085,
0.0218989631250029));
#8326=CARTESIAN_POINT('Ctrl Pts',(0.150796977338198,-0.038164129955926,
0.0215005883543145));
#8327=CARTESIAN_POINT('Ctrl Pts',(0.150635378084855,-0.0387970630280932,
0.0214529292213288));
#8328=CARTESIAN_POINT('Ctrl Pts',(0.150387512308824,-0.0397429743179642,
0.021381919701207));
#8329=CARTESIAN_POINT('Ctrl Pts',(0.15030424830047,-0.0400567199625435,
0.021358402603714));
#8330=CARTESIAN_POINT('Ctrl Pts',(0.150154697699623,-0.0406132068729712,
0.0213167569614059));
#8331=CARTESIAN_POINT('Ctrl Pts',(0.150088804241103,-0.0408560479998004,
0.0212986062025822));
#8332=CARTESIAN_POINT('Ctrl Pts',(0.15002217775146,-0.0410992540443237,
0.0212804509122708));
#8333=CARTESIAN_POINT('Ctrl Pts',(0.150022035316903,-0.0410997739612348,
0.0212804121006641));
#8334=CARTESIAN_POINT('Ctrl Pts',(0.1500217861134,-0.0411006835893117,0.0212803441974421));
#8335=CARTESIAN_POINT('Ctrl Pts',(0.150021679365621,-0.0411010732278623,
0.0212803151112024));
#8336=CARTESIAN_POINT('Ctrl Pts',(0.149945988073925,-0.041377348713481,
0.0212596913844328));
#8337=CARTESIAN_POINT('Ctrl Pts',(0.149869641824313,-0.0416530285702638,
0.021239141158709));
#8338=CARTESIAN_POINT('Ctrl Pts',(0.149660083720702,-0.0424016897444627,
0.0211834081084647));
#8339=CARTESIAN_POINT('Ctrl Pts',(0.149525388905231,-0.0428742585092002,
0.0211483098705703));
#8340=CARTESIAN_POINT('Ctrl Pts',(0.148852441292606,-0.0451935074389334,
0.0209764210814314));
#8341=CARTESIAN_POINT('Ctrl Pts',(0.148282175366296,-0.0470308385630788,
0.0208413871428836));
#8342=CARTESIAN_POINT('Ctrl Pts',(0.146547663600301,-0.0522736475130693,
0.0204580775309201));
#8343=CARTESIAN_POINT('Ctrl Pts',(0.145299081924695,-0.0556500929327148,
0.020213674159934));
#8344=CARTESIAN_POINT('Ctrl Pts',(0.141222836798195,-0.0655976606615059,
0.0194925501555046));
#8345=CARTESIAN_POINT('Ctrl Pts',(0.138058054156169,-0.0720203169219205,
0.0190252143776118));
#8346=CARTESIAN_POINT('Ctrl Pts',(0.129207914896176,-0.0872373344194798,
0.0178651299980061));
#8347=CARTESIAN_POINT('Ctrl Pts',(0.123057151797318,-0.095717941047913,
0.017169351109896));
#8348=CARTESIAN_POINT('Ctrl Pts',(0.115340690505904,-0.104372606189801,
0.0163572971506247));
#8349=CARTESIAN_POINT('Ctrl Pts',(0.114568628014315,-0.105219509408824,
0.0162766613466596));
#8350=CARTESIAN_POINT('Ctrl Pts',(0.113387102756084,-0.10648714444917,0.0161541320151808));
#8351=CARTESIAN_POINT('Ctrl Pts',(0.112984487424815,-0.106914230056936,
0.0161125285405117));
#8352=CARTESIAN_POINT('Ctrl Pts',(0.112259071133417,-0.107675062232297,
0.0160378289602106));
#8353=CARTESIAN_POINT('Ctrl Pts',(0.111937172987326,-0.10800966333412,0.0160047718486466));
#8354=CARTESIAN_POINT('Ctrl Pts',(0.111251383395406,-0.108716157548238,
0.0159345323623914));
#8355=CARTESIAN_POINT('Ctrl Pts',(0.1108871151897,-0.109087675253784,0.0158973338766515));
#8356=CARTESIAN_POINT('Ctrl Pts',(0.109908362866084,-0.110075938493984,
0.0157976733317111));
#8357=CARTESIAN_POINT('Ctrl Pts',(0.109290561071052,-0.110689356611725,
0.0157350663452626));
#8358=CARTESIAN_POINT('Ctrl Pts',(0.106272703409519,-0.113635904194289,
0.0154306438519125));
#8359=CARTESIAN_POINT('Ctrl Pts',(0.103803085387429,-0.115896171158918,
0.0151857395511717));
#8360=CARTESIAN_POINT('Ctrl Pts',(0.0897245142846927,-0.127970149818489,
0.0138109281765094));
#8361=CARTESIAN_POINT('Ctrl Pts',(0.0767990645433999,-0.136119732114037,
0.0126146394232799));
#8362=CARTESIAN_POINT('Ctrl Pts',(0.0587395372212553,-0.144104772115435,
0.0111057763044583));
#8363=CARTESIAN_POINT('Ctrl Pts',(0.0544975130973068,-0.145761960890926,
0.0107627464206152));
#8364=CARTESIAN_POINT('Ctrl Pts',(0.0495685260728842,-0.147442167242722,
0.0103813898888732));
#8365=CARTESIAN_POINT('Ctrl Pts',(0.0489472619512179,-0.147649575164198,
0.0103336304574409));
#8366=CARTESIAN_POINT('Ctrl Pts',(0.0480124011775435,-0.147955127578881,
0.0102622435689829));
#8367=CARTESIAN_POINT('Ctrl Pts',(0.0476997840424651,-0.148056209094316,
0.0102384521091382));
#8368=CARTESIAN_POINT('Ctrl Pts',(0.0471404052402745,-0.148235122826344,
0.0101960272985566));
#8369=CARTESIAN_POINT('Ctrl Pts',(0.0468937721907758,-0.148313329059141,
0.0101773729345747));
#8370=CARTESIAN_POINT('Ctrl Pts',(0.0466455424533205,-0.148391360501144,
0.0101586483329417));
#8371=CARTESIAN_POINT('Ctrl Pts',(0.0466441453019813,-0.148391799676372,
0.0101585429438606));
#8372=CARTESIAN_POINT('Ctrl Pts',(0.0466413718085115,-0.148392671442702,
0.0101583337385513));
#8373=CARTESIAN_POINT('Ctrl Pts',(0.0466399954679868,-0.14839310403394,
0.0101582299223967));
#8374=CARTESIAN_POINT('Ctrl Pts',(0.0466372631672831,-0.148393962768995,
0.0101580238304495));
#8375=CARTESIAN_POINT('Ctrl Pts',(0.0466359072077521,-0.148394388913227,
0.0101579215546601));
#8376=CARTESIAN_POINT('Ctrl Pts',(0.0466332152539379,-0.148395234886573,
0.0101577185119968));
#8377=CARTESIAN_POINT('Ctrl Pts',(0.0466318792582104,-0.148395654716736,
0.0101576177449698));
#8378=CARTESIAN_POINT('Ctrl Pts',(0.0466292268259325,-0.148396488191331,
0.0101574176890716));
#8379=CARTESIAN_POINT('Ctrl Pts',(0.046627910388248,-0.148396901836695,
0.0101573184000722));
#8380=CARTESIAN_POINT('Ctrl Pts',(0.046625296669606,-0.148397723069865,
0.0101571212697479));
#8381=CARTESIAN_POINT('Ctrl Pts',(0.0466239993912728,-0.148398130657403,
0.0101570234285797));
#8382=CARTESIAN_POINT('Ctrl Pts',(0.0466214236110177,-0.148398939896072,
0.0101568291651111));
#8383=CARTESIAN_POINT('Ctrl Pts',(0.0466201451079589,-0.148399341548097,
0.0101567327426853));
#8384=CARTESIAN_POINT('Ctrl Pts',(0.0466176065015387,-0.14840013903569,
0.0101565412881715));
#8385=CARTESIAN_POINT('Ctrl Pts',(0.0466163463984353,-0.148400534871697,
0.0101564462560646));
#8386=CARTESIAN_POINT('Ctrl Pts',(0.0466138442202533,-0.148401320845554,
0.0101562575540438));
#8387=CARTESIAN_POINT('Ctrl Pts',(0.0466126021480873,-0.148401710982991,
0.0101561638843125));
#8388=CARTESIAN_POINT('Ctrl Pts',(0.0466101356848381,-0.14840248567018,
0.0101559778807678));
#8389=CARTESIAN_POINT('Ctrl Pts',(0.0466089112902633,-0.148402870221514,
0.0101558855466552));
#8390=CARTESIAN_POINT('Ctrl Pts',(0.0466064798309384,-0.148403633848262,
0.0101557021877516));
#8391=CARTESIAN_POINT('Ctrl Pts',(0.046605272765933,-0.148404012924226,
0.0101556111629068));
#8392=CARTESIAN_POINT('Ctrl Pts',(0.0466028756256244,-0.148404765708445,
0.0101554303967867));
#8393=CARTESIAN_POINT('Ctrl Pts',(0.0466016855514885,-0.148405139416787,
0.010155340655566));
#8394=CARTESIAN_POINT('Ctrl Pts',(0.0465993220602246,-0.148405881571588,
0.0101551624315061));
#8395=CARTESIAN_POINT('Ctrl Pts',(0.0465981486452686,-0.148406250017801,
0.0101550739487984));
#8396=CARTESIAN_POINT('Ctrl Pts',(0.0465958181561974,-0.148406981748924,
0.0101548982178271));
#8397=CARTESIAN_POINT('Ctrl Pts',(0.046594661080117,-0.148407345034873,
0.010154810969384));
#8398=CARTESIAN_POINT('Ctrl Pts',(0.0465923629565717,-0.148408066544758,
0.0101546376833051));
#8399=CARTESIAN_POINT('Ctrl Pts',(0.0465912219070507,-0.148408424769749,
0.010154551645484));
#8400=CARTESIAN_POINT('Ctrl Pts',(0.0465889555256895,-0.148409136256554,
0.0101543807571137));
#8401=CARTESIAN_POINT('Ctrl Pts',(0.0465878301955188,-0.14840948951824,
0.0101542959066611));
#8402=CARTESIAN_POINT('Ctrl Pts',(0.0465855949552014,-0.148410191173057,
0.0101541273704966));
#8403=CARTESIAN_POINT('Ctrl Pts',(0.0465844850461195,-0.148410539566235,
0.0101540436848368));
#8404=CARTESIAN_POINT('Ctrl Pts',(0.0465822803588516,-0.148411231575936,
0.0101538774563735));
#8405=CARTESIAN_POINT('Ctrl Pts',(0.0465811855808898,-0.148411575192757,
0.0101537949135595));
#8406=CARTESIAN_POINT('Ctrl Pts',(0.0465790108671126,-0.148412257741477,
0.0101536309489353));
#8407=CARTESIAN_POINT('Ctrl Pts',(0.0465779309332553,-0.148412596673119,
0.0101535495272461));
#8408=CARTESIAN_POINT('Ctrl Pts',(0.0462855042456526,-0.148504369766908,
0.0101315022555262));
#8409=CARTESIAN_POINT('Ctrl Pts',(0.045993885571223,-0.148594946877211,
0.0101095855078975));
#8410=CARTESIAN_POINT('Ctrl Pts',(0.0451710318809876,-0.148847871804948,
0.0100479345324943));
#8411=CARTESIAN_POINT('Ctrl Pts',(0.0446391841159549,-0.14900823577186,
0.0100083107017172));
#8412=CARTESIAN_POINT('Ctrl Pts',(0.0415404932451031,-0.149924480561179,
0.00977868969122265));
#8413=CARTESIAN_POINT('Ctrl Pts',(0.0389551547198484,-0.150616933343872,
0.00959203927228974));
#8414=CARTESIAN_POINT('Ctrl Pts',(0.0208776402604556,-0.154962094998815,
0.00831261627153842));
#8415=CARTESIAN_POINT('Ctrl Pts',(0.00492201038245046,-0.156285049961146,
0.00730396116553906));
#8416=CARTESIAN_POINT('Ctrl Pts',(-0.0149121393797758,-0.154884285211148,
0.00594895935770095));
#8417=CARTESIAN_POINT('Ctrl Pts',(-0.0188535971841461,-0.154454042139276,
0.0056752698206136));
#8418=CARTESIAN_POINT('Ctrl Pts',(-0.0237223738176185,-0.153733439655815,
0.00532961666321505));
#8419=CARTESIAN_POINT('Ctrl Pts',(-0.0246693454163375,-0.153584324763353,
0.00526203192250643));
#8420=CARTESIAN_POINT('Ctrl Pts',(-0.0261568474217181,-0.153335983288259,
0.00515528200138179));
#8421=CARTESIAN_POINT('Ctrl Pts',(-0.0266983452501157,-0.153242627180339,
0.0051162987199291));
#8422=CARTESIAN_POINT('Ctrl Pts',(-0.0276539843532365,-0.153072652770617,
0.00504727817049372));
#8423=CARTESIAN_POINT('Ctrl Pts',(-0.028068332820119,-0.152997217501706,
0.0050172779711637));
#8424=CARTESIAN_POINT('Ctrl Pts',(-0.0290176366931578,-0.152820403463939,
0.00494837240085321));
#8425=CARTESIAN_POINT('Ctrl Pts',(-0.0295523737923494,-0.152717897260602,
0.004909432220776));
#8426=CARTESIAN_POINT('Ctrl Pts',(-0.0310303763384798,-0.15242651889748,
0.00480144636119746));
#8427=CARTESIAN_POINT('Ctrl Pts',(-0.0319724308261527,-0.152231703366812,
0.00473221574503593));
#8428=CARTESIAN_POINT('Ctrl Pts',(-0.0373153219638589,-0.151075020128567,
0.00433721632589114));
#8429=CARTESIAN_POINT('Ctrl Pts',(-0.0416741038301823,-0.149931172198991,
0.00400576933909942));
#8430=CARTESIAN_POINT('Ctrl Pts',(-0.0612423353659838,-0.14387677254724,
0.00247333227659507));
#8431=CARTESIAN_POINT('Ctrl Pts',(-0.0756810659941349,-0.136832281527354,
0.00120507771614184));
#8432=CARTESIAN_POINT('Ctrl Pts',(-0.0887899522119582,-0.127719015366539,
5.89805981832114E-17));
#8433=CARTESIAN_POINT('',(0.090360677865021,-0.126612599672283,0.));
#8434=CARTESIAN_POINT('Origin',(0.,0.,0.));
#8435=CARTESIAN_POINT('Ctrl Pts',(0.0903606778650134,-0.126612599672289,
0.));
#8436=CARTESIAN_POINT('Ctrl Pts',(0.0989406669312652,-0.12048924678239,
0.000754967019532015));
#8437=CARTESIAN_POINT('Ctrl Pts',(0.106907661992801,-0.113481681412107,
0.00150993403906405));
#8438=CARTESIAN_POINT('Ctrl Pts',(0.114086638781495,-0.105735714645245,
0.00226490105859606));
#8439=CARTESIAN_POINT('Ctrl Pts',(0.12126935076715,-0.0979857176784843,
0.00302026088487475));
#8440=CARTESIAN_POINT('Ctrl Pts',(0.127662609751503,-0.0894971609184212,
0.00377562071115349));
#8441=CARTESIAN_POINT('Ctrl Pts',(0.13312848579982,-0.0804525249364313,
0.00453098053743217));
#8442=CARTESIAN_POINT('Ctrl Pts',(0.138594284951268,-0.0714080161992201,
0.00528632973690464));
#8443=CARTESIAN_POINT('Ctrl Pts',(0.143132299633338,-0.061808197917734,
0.00604167893637711));
#8444=CARTESIAN_POINT('Ctrl Pts',(0.146649814579393,-0.0518616851233123,
0.00679702813584959));
#8445=CARTESIAN_POINT('Ctrl Pts',(0.150178599016343,-0.0418833054748524,
0.007554797339517));
#8446=CARTESIAN_POINT('Ctrl Pts',(0.152680093031621,-0.0315568445592943,
0.0083125665431844));
#8447=CARTESIAN_POINT('Ctrl Pts',(0.154111282327439,-0.0211072300265195,
0.00907033574685182));
#8448=CARTESIAN_POINT('Ctrl Pts',(0.155398345573063,-0.0117099302875016,
0.00975179479182663));
#8449=CARTESIAN_POINT('Ctrl Pts',(0.155820496503437,-0.00221365697179131,
0.0104332538368014));
#8450=CARTESIAN_POINT('Ctrl Pts',(0.155382497872137,0.0072167759432721,
0.0111147128817762));
#8451=CARTESIAN_POINT('Ctrl Pts',(0.154913520415882,0.0173142057611671,
0.0118443702519497));
#8452=CARTESIAN_POINT('Ctrl Pts',(0.153453826316537,0.0274118070963533,
0.0125740276221232));
#8453=CARTESIAN_POINT('Ctrl Pts',(0.151012327303487,0.0372971782094091,
0.0133036849922967));
#8454=CARTESIAN_POINT('Ctrl Pts',(0.148523466529631,0.0473743120795403,
0.0140474967232347));
#8455=CARTESIAN_POINT('Ctrl Pts',(0.145014246588351,0.0572298640738792,
0.0147913084541726));
#8456=CARTESIAN_POINT('Ctrl Pts',(0.14054958495577,0.0666454549745192,0.0155351201851106));
#8457=CARTESIAN_POINT('Ctrl Pts',(0.13618211944294,0.0758560675417475,0.0162627390620271));
#8458=CARTESIAN_POINT('Ctrl Pts',(0.130900902593814,0.0846448311825029,
0.0169903579389437));
#8459=CARTESIAN_POINT('Ctrl Pts',(0.124815278386068,0.092827521680848,0.0177179768158602));
#8460=CARTESIAN_POINT('Ctrl Pts',(0.118526504643136,0.101283365715225,0.0184698849738089));
#8461=CARTESIAN_POINT('Ctrl Pts',(0.111379145922307,0.109090974738866,0.0192217931317575));
#8462=CARTESIAN_POINT('Ctrl Pts',(0.103539598349753,0.116083392755259,0.0199737012897062));
#8463=CARTESIAN_POINT('Ctrl Pts',(0.0957000507771991,0.123075810771653,
0.0207256094476549));
#8464=CARTESIAN_POINT('Ctrl Pts',(0.0871692388652433,0.129252422489904,
0.0214775176056037));
#8465=CARTESIAN_POINT('Ctrl Pts',(0.0781478618527984,0.134494290539918,
0.0222294257635524));
#8466=CARTESIAN_POINT('Ctrl Pts',(0.0692877936203789,0.139642430178069,
0.0229678892569579));
#8467=CARTESIAN_POINT('Ctrl Pts',(0.0598842350155881,0.143930256984207,
0.0237063527503634));
#8468=CARTESIAN_POINT('Ctrl Pts',(0.0501269156700459,0.14725180754547,0.0244448162437689));
#8469=CARTESIAN_POINT('Ctrl Pts',(0.040384345395474,0.150568337282547,0.0251821634827927));
#8470=CARTESIAN_POINT('Ctrl Pts',(0.0302899137296858,0.152921108078114,
0.0259195107218165));
#8471=CARTESIAN_POINT('Ctrl Pts',(0.0200541531958801,0.154251850684509,
0.0266568579608404));
#8472=CARTESIAN_POINT('Ctrl Pts',(0.00982881691130718,0.155581238043042,
0.0273934542745797));
#8473=CARTESIAN_POINT('Ctrl Pts',(-0.00053664974832034,0.155890524510869,
0.028130050588319));
#8474=CARTESIAN_POINT('Ctrl Pts',(-0.0108238371310163,0.155172958500382,
0.0288666469020583));
#8475=CARTESIAN_POINT('Ctrl Pts',(-0.0211310953995098,0.154453992477928,
0.0296046803569658));
#8476=CARTESIAN_POINT('Ctrl Pts',(-0.0313588440257055,0.152704250068778,
0.0303427138118732));
#8477=CARTESIAN_POINT('Ctrl Pts',(-0.041292688961979,0.149969051268218,
0.0310807472667807));
#8478=CARTESIAN_POINT('Ctrl Pts',(-0.0489637393553047,0.147856893491499,
0.0316506667552441));
#8479=CARTESIAN_POINT('Ctrl Pts',(-0.0564595315799098,0.14515822080781,
0.0322205862437075));
#8480=CARTESIAN_POINT('Ctrl Pts',(-0.0636886258329924,0.141913922641526,
0.0327905057321709));
#8481=CARTESIAN_POINT('Origin',(0.,0.,-0.129405622560373));
#8482=CARTESIAN_POINT('',(-0.0636886257863082,0.141913922662477,0.116740348554263));
#8483=CARTESIAN_POINT('',(-0.0636886551490397,0.141913909484965,0.102789135277549));
#8484=CARTESIAN_POINT('',(-0.0636886258329924,0.141913922641526,-0.129405622560373));
#8485=CARTESIAN_POINT('Ctrl Pts',(-0.0636886257863082,0.141913922662477,
0.116740348554263));
#8486=CARTESIAN_POINT('Ctrl Pts',(-0.0620424217405237,0.14265271186281,
0.116615168449032));
#8487=CARTESIAN_POINT('Ctrl Pts',(-0.060383508450654,0.143362791762632,
0.116489085809456));
#8488=CARTESIAN_POINT('Ctrl Pts',(-0.0580251874220437,0.144324049354148,
0.116309752685824));
#8489=CARTESIAN_POINT('Ctrl Pts',(-0.0573357548266734,0.144599324969004,
0.116257315595819));
#8490=CARTESIAN_POINT('Ctrl Pts',(-0.0562406645258442,0.145027507962682,
0.116173995856029));
#8491=CARTESIAN_POINT('Ctrl Pts',(-0.0558362859078551,0.145183675326336,
0.116143222574248));
#8492=CARTESIAN_POINT('Ctrl Pts',(-0.0550009614651376,0.14550226400819,
0.116079638619344));
#8493=CARTESIAN_POINT('Ctrl Pts',(-0.0545699370206578,0.145664465669511,
0.116046820987017));
#8494=CARTESIAN_POINT('Ctrl Pts',(-0.0536046374289098,0.146022838204867,
0.115973301883517));
#8495=CARTESIAN_POINT('Ctrl Pts',(-0.0530699954896766,0.146217994768411,
0.115932567177777));
#8496=CARTESIAN_POINT('Ctrl Pts',(-0.0517144100575374,0.146704400279421,
0.115829238947803));
#8497=CARTESIAN_POINT('Ctrl Pts',(-0.0508920781983923,0.146991692242151,
0.115766515520857));
#8498=CARTESIAN_POINT('Ctrl Pts',(-0.0462264976389446,0.148577827833571,
0.115410366051632));
#8499=CARTESIAN_POINT('Ctrl Pts',(-0.0423363550000382,0.149732719843836,
0.11511227047896));
#8500=CARTESIAN_POINT('Ctrl Pts',(-0.0365936699490618,0.15119590928656,
0.114670077836691));
#8501=CARTESIAN_POINT('Ctrl Pts',(-0.0347733839474204,0.151624902111698,
0.114529616664305));
#8502=CARTESIAN_POINT('Ctrl Pts',(-0.018532365430285,0.15514464355927,0.113273956077463));
#8503=CARTESIAN_POINT('Ctrl Pts',(-0.00375017290465386,0.156202328724143,
0.112104252392861));
#8504=CARTESIAN_POINT('Ctrl Pts',(0.0135060121633154,0.154983584715789,
0.110803350586831));
#8505=CARTESIAN_POINT('Ctrl Pts',(0.0160487586668345,0.154740955461415,
0.110613591171677));
#8506=CARTESIAN_POINT('Ctrl Pts',(0.0191202559914391,0.154371336158605,
0.110387594302892));
#8507=CARTESIAN_POINT('Ctrl Pts',(0.0196556150860335,0.154304084312003,
0.110348322492503));
#8508=CARTESIAN_POINT('Ctrl Pts',(0.0204887762746792,0.154195016018532,
0.110287401994921));
#8509=CARTESIAN_POINT('Ctrl Pts',(0.0207868182158148,0.154155120287452,
0.110265648549342));
#8510=CARTESIAN_POINT('Ctrl Pts',(0.0213401906058271,0.154079412116607,
0.110225334398859));
#8511=CARTESIAN_POINT('Ctrl Pts',(0.0215955451519675,0.154043829492524,
0.110206761463916));
#8512=CARTESIAN_POINT('Ctrl Pts',(0.0221735181575856,0.153961825870212,
0.110164790378353));
#8513=CARTESIAN_POINT('Ctrl Pts',(0.022496079293076,0.153915025759317,0.110141413858272));
#8514=CARTESIAN_POINT('Ctrl Pts',(0.023471178059506,0.153770418691644,0.110070882932183));
#8515=CARTESIAN_POINT('Ctrl Pts',(0.0241232542399938,0.153669471628086,
0.110023901317037));
#8516=CARTESIAN_POINT('Ctrl Pts',(0.0291301855315081,0.152861698739198,
0.109664435415316));
#8517=CARTESIAN_POINT('Ctrl Pts',(0.0334543419803127,0.151973954159337,
0.109361424648245));
#8518=CARTESIAN_POINT('Ctrl Pts',(0.0520779461492593,0.147316878891845,
0.108065797467015));
#8519=CARTESIAN_POINT('Ctrl Pts',(0.0658360290695337,0.141704062681687,
0.107125770940083));
#8520=CARTESIAN_POINT('Ctrl Pts',(0.0819844109561111,0.132248931608589,
0.105851090010686));
#8521=CARTESIAN_POINT('Ctrl Pts',(0.085296588201257,0.130137277885921,0.105579892784939));
#8522=CARTESIAN_POINT('Ctrl Pts',(0.0892757280571787,0.127383202256364,
0.105239884234909));
#8523=CARTESIAN_POINT('Ctrl Pts',(0.0900217455712659,0.126857089270066,
0.10517550248814));
#8524=CARTESIAN_POINT('Ctrl Pts',(0.091191820718928,0.126016399931856,0.105073491205992));
#8525=CARTESIAN_POINT('Ctrl Pts',(0.0916189904716938,0.12570617244299,0.10503602875127));
#8526=CARTESIAN_POINT('Ctrl Pts',(0.0924157990538203,0.125121279781125,
0.104965730633107));
#8527=CARTESIAN_POINT('Ctrl Pts',(0.0927858145336516,0.124847135256586,
0.104932915401712));
#8528=CARTESIAN_POINT('Ctrl Pts',(0.0936097381018163,0.124231004254791,
0.104859458681007));
#8529=CARTESIAN_POINT('Ctrl Pts',(0.094062998284304,0.123888166600215,0.104818784236378));
#8530=CARTESIAN_POINT('Ctrl Pts',(0.0952040084068251,0.123015256188798,
0.104715715820081));
#8531=CARTESIAN_POINT('Ctrl Pts',(0.0958892096394038,0.122481900253955,
0.104653193107215));
#8532=CARTESIAN_POINT('Ctrl Pts',(0.0997178081236886,0.119449927700367,
0.104300245200098));
#8533=CARTESIAN_POINT('Ctrl Pts',(0.102767714767939,0.116836286286229,0.104005248543059));
#8534=CARTESIAN_POINT('Ctrl Pts',(0.107112586733107,0.112811067830142,0.103563450863328));
#8535=CARTESIAN_POINT('Ctrl Pts',(0.108488276448277,0.11148872862088,0.103420161536768));
#8536=CARTESIAN_POINT('Ctrl Pts',(0.120263270408494,0.0997460443329424,
0.102163703646519));
#8537=CARTESIAN_POINT('Ctrl Pts',(0.129157277509931,0.0879252375315936,
0.100996246852023));
#8538=CARTESIAN_POINT('Ctrl Pts',(0.137506680229921,0.0727628020848725,
0.0996941507690236));
#8539=CARTESIAN_POINT('Ctrl Pts',(0.138699407337796,0.0704626782054384,
0.0995016226795695));
#8540=CARTESIAN_POINT('Ctrl Pts',(0.140070380004365,0.0676489604699325,
0.0992729768596523));
#8541=CARTESIAN_POINT('Ctrl Pts',(0.140304030234754,0.067163028001066,0.0992337329494705));
#8542=CARTESIAN_POINT('Ctrl Pts',(0.140664010968958,0.0664042836522418,
0.0991728461428898));
#8543=CARTESIAN_POINT('Ctrl Pts',(0.140792082175231,0.0661323103345795,
0.0991510986731898));
#8544=CARTESIAN_POINT('Ctrl Pts',(0.141028515351933,0.0656264185744549,
0.0991107927785622));
#8545=CARTESIAN_POINT('Ctrl Pts',(0.141137083211397,0.0653926043351209,
0.0990922221368308));
#8546=CARTESIAN_POINT('Ctrl Pts',(0.141381613834733,0.0648625317080488,
0.0990502515201702));
#8547=CARTESIAN_POINT('Ctrl Pts',(0.14151722668911,0.0645661157697593,0.0990268731973769));
#8548=CARTESIAN_POINT('Ctrl Pts',(0.141924684838699,0.0636680625841192,
0.0989563138682866));
#8549=CARTESIAN_POINT('Ctrl Pts',(0.14219363741077,0.0630651082709919,0.0989093059459589));
#8550=CARTESIAN_POINT('Ctrl Pts',(0.144236152422842,0.0584065738729217,
0.0985487844421466));
#8551=CARTESIAN_POINT('Ctrl Pts',(0.145839920019718,0.0542781948779205,
0.098244810634397));
#8552=CARTESIAN_POINT('Ctrl Pts',(0.152027122322435,0.0360864539923843,
0.0969481510169046));
#8553=CARTESIAN_POINT('Ctrl Pts',(0.154768156470612,0.0214789260872862,
0.0960079134648093));
#8554=CARTESIAN_POINT('Ctrl Pts',(0.155574130201168,0.00279381243316039,
0.0947338128348807));
#8555=CARTESIAN_POINT('Ctrl Pts',(0.155595166007918,-0.00112037355489537,
0.0944635500631644));
#8556=CARTESIAN_POINT('Ctrl Pts',(0.155439132628317,-0.00594220989985941,
0.0941245856004825));
#8557=CARTESIAN_POINT('Ctrl Pts',(0.155401632513466,-0.0068532006863372,
0.0940602818139225));
#8558=CARTESIAN_POINT('Ctrl Pts',(0.155329791835799,-0.0082907571383169,
0.093958371248773));
#8559=CARTESIAN_POINT('Ctrl Pts',(0.15530077648645,-0.00881757880059143,
0.0939209310804517));
#8560=CARTESIAN_POINT('Ctrl Pts',(0.155241422728809,-0.00980383414171339,
0.0938506610407032));
#8561=CARTESIAN_POINT('Ctrl Pts',(0.155211723532694,-0.0102633018265468,
0.093817851527963));
#8562=CARTESIAN_POINT('Ctrl Pts',(0.155140798579042,-0.0112897418853935,
0.0937443898396944));
#8563=CARTESIAN_POINT('Ctrl Pts',(0.155098503974531,-0.0118566312491732,
0.0937037046278102));
#8564=CARTESIAN_POINT('Ctrl Pts',(0.154983698814881,-0.0132894985631701,
0.0936005757014586));
#8565=CARTESIAN_POINT('Ctrl Pts',(0.154907037762978,-0.0141551144439102,
0.0935380029090524));
#8566=CARTESIAN_POINT('Ctrl Pts',(0.154434245828433,-0.0190285497217535,
0.0931841433825164));
#8567=CARTESIAN_POINT('Ctrl Pts',(0.153889870631527,-0.0230200817577691,
0.0928882561223398));
#8568=CARTESIAN_POINT('Ctrl Pts',(0.152862412609119,-0.0288527177048803,
0.0924464454901346));
#8569=CARTESIAN_POINT('Ctrl Pts',(0.152499428661536,-0.0307135190158705,
0.0923040716077476));
#8570=CARTESIAN_POINT('Ctrl Pts',(0.149022206790747,-0.0469536313242474,
0.0910492079518989));
#8571=CARTESIAN_POINT('Ctrl Pts',(0.143917074941132,-0.0608281133680812,
0.0898824871410277));
#8572=CARTESIAN_POINT('Ctrl Pts',(0.135708076983116,-0.0760648897494929,
0.0885804253885668));
#8573=CARTESIAN_POINT('Ctrl Pts',(0.134418872659339,-0.0783206131333061,
0.0883873531254169));
#8574=CARTESIAN_POINT('Ctrl Pts',(0.132794297997063,-0.0810047407770551,
0.0881581535448154));
#8575=CARTESIAN_POINT('Ctrl Pts',(0.132512518454237,-0.0814648763886238,
0.0881188820412622));
#8576=CARTESIAN_POINT('Ctrl Pts',(0.132069994028353,-0.082179131026283,
0.0880579640894007));
#8577=CARTESIAN_POINT('Ctrl Pts',(0.131910900688816,-0.0824342597621625,
0.088036212861481));
#8578=CARTESIAN_POINT('Ctrl Pts',(0.131614037400122,-0.0829072620813196,
0.0879959045761039));
#8579=CARTESIAN_POINT('Ctrl Pts',(0.131476466998102,-0.0831252523251769,
0.0879773352816231));
#8580=CARTESIAN_POINT('Ctrl Pts',(0.131163771188332,-0.0836180231536749,
0.0879353748081064));
#8581=CARTESIAN_POINT('Ctrl Pts',(0.130988324235096,-0.0838925955482885,
0.0879120052431236));
#8582=CARTESIAN_POINT('Ctrl Pts',(0.130455150987439,-0.0847212550308258,
0.0878415021975801));
#8583=CARTESIAN_POINT('Ctrl Pts',(0.130094756001872,-0.0852736300118598,
0.0877945413727638));
#8584=CARTESIAN_POINT('Ctrl Pts',(0.127300309468236,-0.0894977066437365,
0.0874355629769011));
#8585=CARTESIAN_POINT('Ctrl Pts',(0.124714502402889,-0.0930672350041507,
0.087132992378933));
#8586=CARTESIAN_POINT('Ctrl Pts',(0.112832350526481,-0.108083300538572,
0.0858405801862741));
#8587=CARTESIAN_POINT('Ctrl Pts',(0.102087439196792,-0.11828500668543,0.0849031470599794));
#8588=CARTESIAN_POINT('Ctrl Pts',(0.0868246806062007,-0.129124307259356,
0.0836284823518068));
#8589=CARTESIAN_POINT('Ctrl Pts',(0.0834960959158585,-0.131301215515034,
0.0833539682714985));
#8590=CARTESIAN_POINT('Ctrl Pts',(0.0793024801449853,-0.133819874399062,
0.0830102838809307));
#8591=CARTESIAN_POINT('Ctrl Pts',(0.0785128104048151,-0.134284700094577,
0.08294566149629));
#8592=CARTESIAN_POINT('Ctrl Pts',(0.0772611346561105,-0.135006663074031,
0.0828433559093042));
#8593=CARTESIAN_POINT('Ctrl Pts',(0.0768018360474147,-0.135268473673388,
0.0828058414584501));
#8594=CARTESIAN_POINT('Ctrl Pts',(0.0759400642149028,-0.135753899134797,
0.0827354982276535));
#8595=CARTESIAN_POINT('Ctrl Pts',(0.0755379143604969,-0.135978079001588,
0.0827026901430807));
#8596=CARTESIAN_POINT('Ctrl Pts',(0.0746380887361048,-0.136474466426095,
0.082629317281405));
#8597=CARTESIAN_POINT('Ctrl Pts',(0.074139909465216,-0.136745742475572,
0.0825887198845213));
#8598=CARTESIAN_POINT('Ctrl Pts',(0.0728784041261681,-0.137423756349601,
0.0824859736068982));
#8599=CARTESIAN_POINT('Ctrl Pts',(0.0721131573090637,-0.137826859080366,
0.0824236973756138));
#8600=CARTESIAN_POINT('Ctrl Pts',(0.0678200458718348,-0.140042764594081,
0.0820745617190062));
#8601=CARTESIAN_POINT('Ctrl Pts',(0.0642275231545033,-0.141726336682912,
0.0817832455929904));
#8602=CARTESIAN_POINT('Ctrl Pts',(0.0587786614215767,-0.144030117114458,
0.081342146320132));
#8603=CARTESIAN_POINT('Ctrl Pts',(0.0569683840613695,-0.144755684965672,
0.0811957296120877));
#8604=CARTESIAN_POINT('Ctrl Pts',(0.0413904993789112,-0.150661909183268,
0.0799370815355001));
#8605=CARTESIAN_POINT('Ctrl Pts',(0.0269680403509924,-0.153898768608725,
0.0787706492050606));
#8606=CARTESIAN_POINT('Ctrl Pts',(0.00970466905530235,-0.155268915258471,
0.077467670514589));
#8607=CARTESIAN_POINT('Ctrl Pts',(0.00709745880679463,-0.15540992539813,
0.0772736249341517));
#8608=CARTESIAN_POINT('Ctrl Pts',(0.00394751013914065,-0.155500841635551,
0.0770434164607347));
#8609=CARTESIAN_POINT('Ctrl Pts',(0.00340719718354766,-0.155513618748746,
0.077004078915776));
#8610=CARTESIAN_POINT('Ctrl Pts',(0.00256594683112066,-0.155529125796509,
0.0769430766562806));
#8611=CARTESIAN_POINT('Ctrl Pts',(0.00226505679554624,-0.155533798822233,
0.0769213067721626));
#8612=CARTESIAN_POINT('Ctrl Pts',(0.00170625040128141,-0.15554085551139,
0.0768809691482868));
#8613=CARTESIAN_POINT('Ctrl Pts',(0.00144834432381692,-0.155543470850301,
0.0768623891417416));
#8614=CARTESIAN_POINT('Ctrl Pts',(0.000864526454679085,-0.155547938948567,
0.0768204126446921));
#8615=CARTESIAN_POINT('Ctrl Pts',(0.000538615213439235,-0.155549408922255,
0.0767970377394832));
#8616=CARTESIAN_POINT('Ctrl Pts',(-0.000446417359977353,-0.155550755848506,
0.0767265585835222));
#8617=CARTESIAN_POINT('Ctrl Pts',(-0.00110554718381486,-0.155547467804036,
0.0766796265436433));
#8618=CARTESIAN_POINT('Ctrl Pts',(-0.00614768498146172,-0.155490263109722,
0.0763222232301394));
#8619=CARTESIAN_POINT('Ctrl Pts',(-0.0105271793515263,-0.155255284526461,
0.0760210954838136));
#8620=CARTESIAN_POINT('Ctrl Pts',(-0.0296255250221091,-0.153418493025023,
0.0747258095397929));
#8621=CARTESIAN_POINT('Ctrl Pts',(-0.0440820349770182,-0.149905735658397,
0.0737846722921825));
#8622=CARTESIAN_POINT('Ctrl Pts',(-0.0614703784982253,-0.142942699521187,
0.0725087381242133));
#8623=CARTESIAN_POINT('Ctrl Pts',(-0.0650589438490988,-0.14134550615587,
0.0722375431063856));
#8624=CARTESIAN_POINT('Ctrl Pts',(-0.0694025467099712,-0.139211790956327,
0.0718975236628699));
#8625=CARTESIAN_POINT('Ctrl Pts',(-0.0702185156422144,-0.138802003690988,
0.0718331262762424));
#8626=CARTESIAN_POINT('Ctrl Pts',(-0.0715006475479744,-0.138143906129541,
0.0717310868852342));
#8627=CARTESIAN_POINT('Ctrl Pts',(-0.0719692443877624,-0.137900359862675,
0.0716936119503776));
#8628=CARTESIAN_POINT('Ctrl Pts',(-0.0728442761628356,-0.137439900196713,
0.0716232882724585));
#8629=CARTESIAN_POINT('Ctrl Pts',(-0.0732510064601142,-0.137223557671308,
0.0715904599580668));
#8630=CARTESIAN_POINT('Ctrl Pts',(-0.0741575620964936,-0.136736175790977,
0.0715169710569374));
#8631=CARTESIAN_POINT('Ctrl Pts',(-0.0746568722625348,-0.13646419748105,
0.0714762774888386));
#8632=CARTESIAN_POINT('Ctrl Pts',(-0.0759153361796357,-0.135769727998318,
0.071373155025313));
#8633=CARTESIAN_POINT('Ctrl Pts',(-0.0766724535884431,-0.135343607576513,
0.0713105972786505));
#8634=CARTESIAN_POINT('Ctrl Pts',(-0.0809120641337486,-0.132910481753134,
0.0709573261910329));
#8635=CARTESIAN_POINT('Ctrl Pts',(-0.0843189980026695,-0.130775606864694,
0.0706620337934866));
#8636=CARTESIAN_POINT('Ctrl Pts',(-0.0892166422127744,-0.127435626540591,
0.0702198337913709));
#8637=CARTESIAN_POINT('Ctrl Pts',(-0.0907741064144418,-0.126330951227118,
0.0700764441889221));
#8638=CARTESIAN_POINT('Ctrl Pts',(-0.104166813738272,-0.116456256076863,
0.0688191948786559));
#8639=CARTESIAN_POINT('Ctrl Pts',(-0.114719286602177,-0.106076350818248,
0.0676510071300562));
#8640=CARTESIAN_POINT('Ctrl Pts',(-0.125219507963493,-0.0923175723981026,
0.0663491698909107));
#8641=CARTESIAN_POINT('Ctrl Pts',(-0.126733642344316,-0.0902277416492988,
0.0661574216084644));
#8642=CARTESIAN_POINT('Ctrl Pts',(-0.128500239017742,-0.0876571796417167,
0.0659295738996789));
#8643=CARTESIAN_POINT('Ctrl Pts',(-0.128802981934727,-0.0872117219080123,
0.0658903735618032));
#8644=CARTESIAN_POINT('Ctrl Pts',(-0.12927103040024,-0.0865152790108211,
0.0658295381904516));
#8645=CARTESIAN_POINT('Ctrl Pts',(-0.129437928623524,-0.0862653779965664,
0.065807798884406));
#8646=CARTESIAN_POINT('Ctrl Pts',(-0.129746584477844,-0.0858003071483235,
0.0657675106319524));
#8647=CARTESIAN_POINT('Ctrl Pts',(-0.129888530418938,-0.0855852706839214,
0.0657489494466757));
#8648=CARTESIAN_POINT('Ctrl Pts',(-0.130208759221599,-0.0850975186224531,
0.0657069991243744));
#8649=CARTESIAN_POINT('Ctrl Pts',(-0.130386719592729,-0.0848245955655089,
0.0656836316371968));
#8650=CARTESIAN_POINT('Ctrl Pts',(-0.130922799657613,-0.083996780753346,
0.0656130681186414));
#8651=CARTESIAN_POINT('Ctrl Pts',(-0.131278250648963,-0.0834401557722822,
0.0655660455506756));
#8652=CARTESIAN_POINT('Ctrl Pts',(-0.13399905783635,-0.079119031505382,
0.0652041345617505));
#8653=CARTESIAN_POINT('Ctrl Pts',(-0.136205859503016,-0.0752565065471865,
0.0648988822822525));
#8654=CARTESIAN_POINT('Ctrl Pts',(-0.141714760659104,-0.0645758808156944,
0.0640881135628669));
#8655=CARTESIAN_POINT('Ctrl Pts',(-0.144689543731709,-0.0576026739184621,
0.063593327653544));
#8656=CARTESIAN_POINT('Ctrl Pts',(-0.150613829678048,-0.0403202637994308,
0.0623900042066171));
#8657=CARTESIAN_POINT('Ctrl Pts',(-0.153029106901279,-0.0298712104368924,
0.0616792021526925));
#8658=CARTESIAN_POINT('Ctrl Pts',(-0.154494129726095,-0.018129004019262,
0.0608506590700042));
#8659=CARTESIAN_POINT('Ctrl Pts',(-0.154622592056141,-0.0169985531895867,
0.0607706245342408));
#8660=CARTESIAN_POINT('Ctrl Pts',(-0.154798110114348,-0.0152868413419617,
0.0606489874582022));
#8661=CARTESIAN_POINT('Ctrl Pts',(-0.154854318963561,-0.0147065391824214,
0.0606076722568643));
#8662=CARTESIAN_POINT('Ctrl Pts',(-0.154949159031645,-0.0136665083244172,
0.0605334804305667));
#8663=CARTESIAN_POINT('Ctrl Pts',(-0.154989010070782,-0.0132068952923857,
0.0605006424688547));
#8664=CARTESIAN_POINT('Ctrl Pts',(-0.155069192505128,-0.012231739251074,
0.0604308592307879));
#8665=CARTESIAN_POINT('Ctrl Pts',(-0.155108998752173,-0.0117161599282944,
0.0603938978999998));
#8666=CARTESIAN_POINT('Ctrl Pts',(-0.1552085558945,-0.010337109253723,0.0602948536877656));
#8667=CARTESIAN_POINT('Ctrl Pts',(-0.15526367110381,-0.00947333255247916,
0.060232626508677));
#8668=CARTESIAN_POINT('Ctrl Pts',(-0.155495811388464,-0.00528545753706559,
0.0599299675461191));
#8669=CARTESIAN_POINT('Ctrl Pts',(-0.155573296462417,-0.0019569579792852,
0.0596864564976343));
#8670=CARTESIAN_POINT('Ctrl Pts',(-0.155411983463436,0.0163412818140053,
0.0583301774315003));
#8671=CARTESIAN_POINT('Ctrl Pts',(-0.15311936023218,0.0312124088466213,
0.0571524755466076));
#8672=CARTESIAN_POINT('Ctrl Pts',(-0.148476009409317,0.0463841534662506,
0.0559365572065336));
#8673=CARTESIAN_POINT('Ctrl Pts',(-0.148204713258434,0.0472438152887168,
0.0558676484324315));
#8674=CARTESIAN_POINT('Ctrl Pts',(-0.147636827434995,0.0489902427401683,
0.0557276896387132));
#8675=CARTESIAN_POINT('Ctrl Pts',(-0.147339682704012,0.0498767948979903,
0.0556566578947094));
#8676=CARTESIAN_POINT('Ctrl Pts',(-0.145999878873975,0.0537577053059277,
0.0553459295842282));
#8677=CARTESIAN_POINT('Ctrl Pts',(-0.144873707694657,0.056722729542674,
0.0551090871481001));
#8678=CARTESIAN_POINT('Ctrl Pts',(-0.143448677357211,0.0601546025319333,
0.0548372133532378));
#8679=CARTESIAN_POINT('Ctrl Pts',(-0.143237130899882,0.0606566038985881,
0.054797502630525));
#8680=CARTESIAN_POINT('Ctrl Pts',(-0.142892756882392,0.0614619571625992,
0.0547339004482372));
#8681=CARTESIAN_POINT('Ctrl Pts',(-0.142761592817414,0.0617660082042662,
0.0547099124555957));
#8682=CARTESIAN_POINT('Ctrl Pts',(-0.142526236218627,0.0623068327183942,
0.0546672904537251));
#8683=CARTESIAN_POINT('Ctrl Pts',(-0.142422423149672,0.0625437670930051,
0.0546486337898382));
#8684=CARTESIAN_POINT('Ctrl Pts',(-0.142199663998522,0.0630487434381924,
0.0546089057718721));
#8685=CARTESIAN_POINT('Ctrl Pts',(-0.142080551168763,0.0633167076993923,
0.0545878448247476));
#8686=CARTESIAN_POINT('Ctrl Pts',(-0.141753890060667,0.0640460230549665,
0.0545305754020657));
#8687=CARTESIAN_POINT('Ctrl Pts',(-0.141544845310254,0.0645067066410245,
0.0544944570395705));
#8688=CARTESIAN_POINT('Ctrl Pts',(-0.140453343128435,0.0668812564207846,
0.0543085402394668));
#8689=CARTESIAN_POINT('Ctrl Pts',(-0.139534248819734,0.0687781843952986,
0.0541608668139271));
#8690=CARTESIAN_POINT('Ctrl Pts',(-0.136701685617625,0.0743336613117928,
0.0537291738344154));
#8691=CARTESIAN_POINT('Ctrl Pts',(-0.134680722045666,0.0779355691557279,
0.0534503055345552));
#8692=CARTESIAN_POINT('Ctrl Pts',(-0.12703079751817,0.0903814811031068,
0.0524752682921748));
#8693=CARTESIAN_POINT('Ctrl Pts',(-0.120654684808217,0.098732428056966,
0.051797935341465));
#8694=CARTESIAN_POINT('Ctrl Pts',(-0.111442521379164,0.108560144880349,
0.0508963679610258));
#8695=CARTESIAN_POINT('Ctrl Pts',(-0.109335556218786,0.110681864931461,
0.0506946575231969));
#8696=CARTESIAN_POINT('Ctrl Pts',(-0.104522098578831,0.115257401612486,
0.05024149871917));
#8697=CARTESIAN_POINT('Ctrl Pts',(-0.101787768178444,0.117679158397521,
0.0499890649108242));
#8698=CARTESIAN_POINT('Ctrl Pts',(-0.0982578283029227,0.120590447827129,
0.0496676822709614));
#8699=CARTESIAN_POINT('Ctrl Pts',(-0.0975395019251896,0.121172201549451,
0.0496025083143314));
#8700=CARTESIAN_POINT('Ctrl Pts',(-0.0963964672043183,0.122081165563429,
0.0494991309605083));
#8701=CARTESIAN_POINT('Ctrl Pts',(-0.0959751703780766,0.122412648581027,
0.0494610983007411));
#8702=CARTESIAN_POINT('Ctrl Pts',(-0.0951890867126423,0.123024599153411,
0.0493902589202329));
#8703=CARTESIAN_POINT('Ctrl Pts',(-0.094824751407512,0.123305639523101,
0.0493574753332094));
#8704=CARTESIAN_POINT('Ctrl Pts',(-0.0940154479961255,0.12392421054803,
0.0492847577468119));
#8705=CARTESIAN_POINT('Ctrl Pts',(-0.0935698999852716,0.124260968222449,
0.0492447940238498));
#8706=CARTESIAN_POINT('Ctrl Pts',(-0.0922783358781314,0.125226283390147,
0.0491291395502704));
#8707=CARTESIAN_POINT('Ctrl Pts',(-0.0914277471660367,0.125848640321269,
0.0490532098600685));
#8708=CARTESIAN_POINT('Ctrl Pts',(-0.0850298019981282,0.130430779120129,
0.0484837363602214));
#8709=CARTESIAN_POINT('Ctrl Pts',(-0.0792347281175303,0.134030174044826,
0.0479766144168766));
#8710=CARTESIAN_POINT('Ctrl Pts',(-0.0700971602533137,0.138905522278269,
0.0471892813764483));
#8711=CARTESIAN_POINT('Ctrl Pts',(-0.066917046829144,0.140465061453259,
0.046917478598225));
#8712=CARTESIAN_POINT('Ctrl Pts',(-0.0636885943104762,0.141913936788307,
0.046644325870219));
#8713=CARTESIAN_POINT('',(-0.155549967545476,0.000100481845383891,0.045594377439629));
#8714=CARTESIAN_POINT('Ctrl Pts',(-0.0636886258329924,0.141913922641526,
0.0327905057321709));
#8715=CARTESIAN_POINT('Ctrl Pts',(-0.0660294620340356,0.140863393995925,
0.0329750500365568));
#8716=CARTESIAN_POINT('Ctrl Pts',(-0.0683424013010257,0.139755784576519,
0.0331595943409427));
#8717=CARTESIAN_POINT('Ctrl Pts',(-0.0706245494042477,0.138592840801562,
0.0333441386453286));
#8718=CARTESIAN_POINT('Ctrl Pts',(-0.079758546308512,0.133938311665045,
0.0340827528932735));
#8719=CARTESIAN_POINT('Ctrl Pts',(-0.0884632964101746,0.128360212860196,
0.0348213671412184));
#8720=CARTESIAN_POINT('Ctrl Pts',(-0.0965470015752083,0.121960973212076,
0.0355599813891633));
#8721=CARTESIAN_POINT('Ctrl Pts',(-0.104663083221479,0.11553610362593,0.0363015539006584));
#8722=CARTESIAN_POINT('Ctrl Pts',(-0.112152308750486,0.108283954652407,
0.0370431264121535));
#8723=CARTESIAN_POINT('Ctrl Pts',(-0.118849199871259,0.100352728861558,
0.0377846989236486));
#8724=CARTESIAN_POINT('Ctrl Pts',(-0.1255048724983,0.0924703187337775,0.0385217071527975));
#8725=CARTESIAN_POINT('Ctrl Pts',(-0.131377343306342,0.083917886634347,
0.0392587153819463));
#8726=CARTESIAN_POINT('Ctrl Pts',(-0.136342973587973,0.0748758709678172,
0.0399957236110952));
#8727=CARTESIAN_POINT('Ctrl Pts',(-0.141354731994914,0.0657498596737304,
0.0407395782637634));
#8728=CARTESIAN_POINT('Ctrl Pts',(-0.145442231278217,0.0561259457345724,
0.0414834329164317));
#8729=CARTESIAN_POINT('Ctrl Pts',(-0.14852637524592,0.046213832954086,0.0422272875690999));
#8730=CARTESIAN_POINT('Ctrl Pts',(-0.151610519213623,0.0363017201735995,
0.0429711422217682));
#8731=CARTESIAN_POINT('Ctrl Pts',(-0.153691150142048,0.0261023555329522,
0.0437149968744365));
#8732=CARTESIAN_POINT('Ctrl Pts',(-0.154741787599696,0.0158360875992346,
0.0444588515271047));
#8733=CARTESIAN_POINT('Ctrl Pts',(-0.155276401924124,0.0106121220382939,
0.0448373601646128));
#8734=CARTESIAN_POINT('Ctrl Pts',(-0.155546569792262,0.00536034147729075,
0.0452158688021209));
#8735=CARTESIAN_POINT('Ctrl Pts',(-0.155549967545476,0.000100481845383891,
0.045594377439629));
#8736=CARTESIAN_POINT('Ctrl Pts',(-0.155549962667911,0.000107768322894147,
0.0457021375939884));
#8737=CARTESIAN_POINT('Ctrl Pts',(-0.155558024611102,-0.0115286284275358,
0.0464889715817548));
#8738=CARTESIAN_POINT('Ctrl Pts',(-0.154260364033593,-0.0231303105295702,
0.0472366725437763));
#8739=CARTESIAN_POINT('Ctrl Pts',(-0.150258512393375,-0.0407348573768369,
0.0484402774613486));
#8740=CARTESIAN_POINT('Ctrl Pts',(-0.148451260673314,-0.0468951615387702,
0.0488747267934762));
#8741=CARTESIAN_POINT('Ctrl Pts',(-0.145763792723458,-0.0543224180017188,
0.0494253367338388));
#8742=CARTESIAN_POINT('Ctrl Pts',(-0.145238488188932,-0.0557116652596488,
0.0495295004996491));
#8743=CARTESIAN_POINT('Ctrl Pts',(-0.144459156074046,-0.0576867573758456,
0.0496793745242537));
#8744=CARTESIAN_POINT('Ctrl Pts',(-0.144221277345524,-0.0582789231962408,
0.0497245408636152));
#8745=CARTESIAN_POINT('Ctrl Pts',(-0.143803081270126,-0.0593017222636224,
0.0498029629727483));
#8746=CARTESIAN_POINT('Ctrl Pts',(-0.143624455195613,-0.0597330420054922,
0.0498361610287936));
#8747=CARTESIAN_POINT('Ctrl Pts',(-0.143277644681902,-0.060559918951737,
0.0499000521954672));
#8748=CARTESIAN_POINT('Ctrl Pts',(-0.143109756781965,-0.0609555965926227,
0.0499307349388027));
#8749=CARTESIAN_POINT('Ctrl Pts',(-0.142666536556045,-0.0619882520766492,
0.050011101922015));
#8750=CARTESIAN_POINT('Ctrl Pts',(-0.142388580540545,-0.0626240860287197,
0.0500608756447366));
#8751=CARTESIAN_POINT('Ctrl Pts',(-0.14141415028925,-0.0648131007742427,
0.0502332522957411));
#8752=CARTESIAN_POINT('Ctrl Pts',(-0.140696464959421,-0.0663566443604307,
0.0503565821150925));
#8753=CARTESIAN_POINT('Ctrl Pts',(-0.134421968092164,-0.0792917431082303,
0.0514056797504091));
#8754=CARTESIAN_POINT('Ctrl Pts',(-0.127518436468818,-0.0899741896379027,
0.0523810920631677));
#8755=CARTESIAN_POINT('Ctrl Pts',(-0.115949656265776,-0.103828851920947,
0.0537820188206415));
#8756=CARTESIAN_POINT('Ctrl Pts',(-0.112288856128531,-0.10777741771989,
0.0541992656013646));
#8757=CARTESIAN_POINT('Ctrl Pts',(-0.106503961533513,-0.113401628571723,
0.054813925867454));
#8758=CARTESIAN_POINT('Ctrl Pts',(-0.104528951963616,-0.115224664689301,
0.0550166942025176));
#8759=CARTESIAN_POINT('Ctrl Pts',(-0.101722769557173,-0.11768334368236,
0.0552940821521655));
#8760=CARTESIAN_POINT('Ctrl Pts',(-0.10093104274525,-0.118363068506035,
0.0553712058482486));
#8761=CARTESIAN_POINT('Ctrl Pts',(-0.0995519884880571,-0.119523134015233,
0.0555035075653008));
#8762=CARTESIAN_POINT('Ctrl Pts',(-0.0989678869695426,-0.120007230569266,
0.0555589268443804));
#8763=CARTESIAN_POINT('Ctrl Pts',(-0.098113854120641,-0.120704566655798,
0.0556390363765802));
#8764=CARTESIAN_POINT('Ctrl Pts',(-0.0978467327447785,-0.120921204424147,
0.0556639633352689));
#8765=CARTESIAN_POINT('Ctrl Pts',(-0.0973872367572115,-0.121291340096473,
0.055706617471833));
#8766=CARTESIAN_POINT('Ctrl Pts',(-0.0971952150907193,-0.12144526846428,
0.0557243754795696));
#8767=CARTESIAN_POINT('Ctrl Pts',(-0.096810301883321,-0.121752324829042,
0.055759837718814));
#8768=CARTESIAN_POINT('Ctrl Pts',(-0.0966174129919684,-0.121905449677483,
0.055777541853343));
#8769=CARTESIAN_POINT('Ctrl Pts',(-0.0960971635096071,-0.122316439295845,
0.0558251154853686));
#8770=CARTESIAN_POINT('Ctrl Pts',(-0.0957691257672256,-0.122573450294928,
0.0558549246400376));
#8771=CARTESIAN_POINT('Ctrl Pts',(-0.0945547644075812,-0.123517026958475,
0.0559646005871443));
#8772=CARTESIAN_POINT('Ctrl Pts',(-0.0936620297372567,-0.124195345321396,
0.0560439100399647));
#8773=CARTESIAN_POINT('Ctrl Pts',(-0.0824065301544903,-0.132557106066507,
0.0570285880487809));
#8774=CARTESIAN_POINT('Ctrl Pts',(-0.0711324056003403,-0.138933518089678,
0.0578577485246019));
#8775=CARTESIAN_POINT('Ctrl Pts',(-0.051084477838859,-0.147184125789049,
0.0592908711371011));
#8776=CARTESIAN_POINT('Ctrl Pts',(-0.0427036775644092,-0.149830411958971,
0.0598787750660659));
#8777=CARTESIAN_POINT('Ctrl Pts',(-0.0327776107720131,-0.152063789268373,
0.0605889673347968));
#8778=CARTESIAN_POINT('Ctrl Pts',(-0.0314058639598889,-0.152353008694267,
0.0606873811812471));
#8779=CARTESIAN_POINT('Ctrl Pts',(-0.0294149968837752,-0.152744734393208,
0.060830680738746));
#8780=CARTESIAN_POINT('Ctrl Pts',(-0.0287988413252484,-0.152862103361327,
0.060875095072924));
#8781=CARTESIAN_POINT('Ctrl Pts',(-0.0277210640757414,-0.153060657191675,
0.060952904455174));
#8782=CARTESIAN_POINT('Ctrl Pts',(-0.0272597505570381,-0.153143488807817,
0.0609862469561173));
#8783=CARTESIAN_POINT('Ctrl Pts',(-0.0263660076807935,-0.153299799513147,
0.061050921551755));
#8784=CARTESIAN_POINT('Ctrl Pts',(-0.0259336274836434,-0.153373536994129,
0.0610822451364215));
#8785=CARTESIAN_POINT('Ctrl Pts',(-0.0247862828144139,-0.153564213059886,
0.0611654598481627));
#8786=CARTESIAN_POINT('Ctrl Pts',(-0.0240708107705878,-0.153677986011225,
0.0612174502547086));
#8787=CARTESIAN_POINT('Ctrl Pts',(-0.0215139405372053,-0.154066281045172,
0.0614036168498079));
#8788=CARTESIAN_POINT('Ctrl Pts',(-0.0196685075761934,-0.15431272742267,
0.0615386684898708));
#8789=CARTESIAN_POINT('Ctrl Pts',(-0.0160355858013158,-0.154731657896973,
0.0618059932502063));
#8790=CARTESIAN_POINT('Ctrl Pts',(-0.0142486467287317,-0.154906428358918,
0.0619381738702446));
#8791=CARTESIAN_POINT('Ctrl Pts',(0.00318408565992699,-0.156307245454273,
0.063234632820172));
#8792=CARTESIAN_POINT('Ctrl Pts',(0.0189263985821658,-0.155189236581051,
0.0644731630295722));
#8793=CARTESIAN_POINT('Ctrl Pts',(0.0369547823508225,-0.151122305282958,
0.0658815128390439));
#8794=CARTESIAN_POINT('Ctrl Pts',(0.0396631080709215,-0.150434195178028,
0.0660924094410291));
#8795=CARTESIAN_POINT('Ctrl Pts',(0.0433859963875568,-0.149380766691674,
0.0663801336570163));
#8796=CARTESIAN_POINT('Ctrl Pts',(0.0444173646932103,-0.149077349095493,
0.0664596077686002));
#8797=CARTESIAN_POINT('Ctrl Pts',(0.0459673615309527,-0.148603842090421,
0.0665786077371196));
#8798=CARTESIAN_POINT('Ctrl Pts',(0.0464883513607945,-0.148441683569055,
0.0666185312696393));
#8799=CARTESIAN_POINT('Ctrl Pts',(0.0473328390247322,-0.148173953946187,
0.0666831105193796));
#8800=CARTESIAN_POINT('Ctrl Pts',(0.0476568567849441,-0.148070058706635,
0.0667078565054399));
#8801=CARTESIAN_POINT('Ctrl Pts',(0.0482775487280908,-0.147868787382596,
0.0667551950621032));
#8802=CARTESIAN_POINT('Ctrl Pts',(0.0485742752651706,-0.147771579744889,
0.0667777969958995));
#8803=CARTESIAN_POINT('Ctrl Pts',(0.0491093166747904,-0.147594514409789,
0.066818497369476));
#8804=CARTESIAN_POINT('Ctrl Pts',(0.0493477316498017,-0.14751497229936,
0.0668366138577791));
#8805=CARTESIAN_POINT('Ctrl Pts',(0.0498752900744485,-0.147337541454609,
0.0668766576513732));
#8806=CARTESIAN_POINT('Ctrl Pts',(0.0501643380131203,-0.147239379508195,
0.066898568653258));
#8807=CARTESIAN_POINT('Ctrl Pts',(0.0509679131858796,-0.146963840861739,
0.0669594073880247));
#8808=CARTESIAN_POINT('Ctrl Pts',(0.0514818081365596,-0.146784611420634,
0.0669982280784462));
#8809=CARTESIAN_POINT('Ctrl Pts',(0.054204916723793,-0.145818821585571,
0.0672035319946431));
#8810=CARTESIAN_POINT('Ctrl Pts',(0.0563972238880154,-0.144985021483711,
0.0673673975335468));
#8811=CARTESIAN_POINT('Ctrl Pts',(0.0601517844275243,-0.143458986269328,
0.0676469578857969));
#8812=CARTESIAN_POINT('Ctrl Pts',(0.0617229480510002,-0.142790041880342,
0.067763611754893));
#8813=CARTESIAN_POINT('Ctrl Pts',(0.0745635247938152,-0.137071429470947,
0.0687167466592353));
#8814=CARTESIAN_POINT('Ctrl Pts',(0.0852064307917572,-0.130721865472826,
0.0695085577317131));
#8815=CARTESIAN_POINT('Ctrl Pts',(0.0984826038764124,-0.120484294574988,
0.0706295555624915));
#8816=CARTESIAN_POINT('Ctrl Pts',(0.101861688190277,-0.117641318565557,
0.0709281200845115));
#8817=CARTESIAN_POINT('Ctrl Pts',(0.107085941658198,-0.112851903994566,
0.0714162424586966));
#8818=CARTESIAN_POINT('Ctrl Pts',(0.109009746513577,-0.11099470621197,0.071602268243785));
#8819=CARTESIAN_POINT('Ctrl Pts',(0.111448073854493,-0.108516242025504,
0.0718469891751459));
#8820=CARTESIAN_POINT('Ctrl Pts',(0.112007051120769,-0.107939188458225,
0.0719037267329255));
#8821=CARTESIAN_POINT('Ctrl Pts',(0.112909196081731,-0.106993316118218,
0.0719963556560799));
#8822=CARTESIAN_POINT('Ctrl Pts',(0.113255091767286,-0.106627109272011,
0.0720321289145246));
#8823=CARTESIAN_POINT('Ctrl Pts',(0.113917062813364,-0.105919411892233,
0.0721010942523742));
#8824=CARTESIAN_POINT('Ctrl Pts',(0.114233397141567,-0.105578170018578,
0.0721342747567758));
#8825=CARTESIAN_POINT('Ctrl Pts',(0.114954444913339,-0.104793314096841,
0.072210425512628));
#8826=CARTESIAN_POINT('Ctrl Pts',(0.115358127973879,-0.104348767967743,
0.0722534386550659));
#8827=CARTESIAN_POINT('Ctrl Pts',(0.116424182888106,-0.103161054502894,
0.0723680521683697));
#8828=CARTESIAN_POINT('Ctrl Pts',(0.1170820019893,-0.102413857713801,0.0724398408761141));
#8829=CARTESIAN_POINT('Ctrl Pts',(0.121990231966919,-0.0967296527928284,
0.0729836934464149));
#8830=CARTESIAN_POINT('Ctrl Pts',(0.125933277609011,-0.0915370390176759,
0.0734681461051096));
#8831=CARTESIAN_POINT('Ctrl Pts',(0.137430671811926,-0.0742416881248383,
0.0750451771246575));
#8832=CARTESIAN_POINT('Ctrl Pts',(0.14365234563892,-0.0613430800222112,
0.0761752967707421));
#8833=CARTESIAN_POINT('Ctrl Pts',(0.148733105106667,-0.0456015200528958,
0.0774156868990523));
#8834=CARTESIAN_POINT('Ctrl Pts',(0.149387677125026,-0.043409199728889,
0.0775853047829655));
#8835=CARTESIAN_POINT('Ctrl Pts',(0.150131188385693,-0.0407025577367529,
0.077790258551602));
#8836=CARTESIAN_POINT('Ctrl Pts',(0.150266179081798,-0.0402013355163685,
0.0778280264041635));
#8837=CARTESIAN_POINT('Ctrl Pts',(0.150474230345912,-0.0394131472304948,
0.0778871159788191));
#8838=CARTESIAN_POINT('Ctrl Pts',(0.150548983151571,-0.0391266386090154,
0.0779085327960744));
#8839=CARTESIAN_POINT('Ctrl Pts',(0.150687361646393,-0.038590000650366,
0.0779485281033003));
#8840=CARTESIAN_POINT('Ctrl Pts',(0.150751182210413,-0.038339929237776,
0.0779671172590649));
#8841=CARTESIAN_POINT('Ctrl Pts',(0.150895636425184,-0.0377679694572135,
0.0780095244812217));
#8842=CARTESIAN_POINT('Ctrl Pts',(0.15097586256843,-0.0374459815783716,
0.0780333188822446));
#8843=CARTESIAN_POINT('Ctrl Pts',(0.151219958242503,-0.0364527656206297,
0.078106479848725));
#8844=CARTESIAN_POINT('Ctrl Pts',(0.151380389455408,-0.0357806879209509,
0.0781556536594493));
#8845=CARTESIAN_POINT('Ctrl Pts',(0.153504691109276,-0.0266114656720041,
0.0788223059836024));
#8846=CARTESIAN_POINT('Ctrl Pts',(0.154755391654972,-0.017963342508237,
0.0794020841493169));
#8847=CARTESIAN_POINT('Ctrl Pts',(0.155752183254429,-0.00123921421103569,
0.080507138202634));
#8848=CARTESIAN_POINT('Ctrl Pts',(0.155608548296183,0.00680087273579766,
0.0810315888583669));
#8849=CARTESIAN_POINT('Ctrl Pts',(0.154460085448954,0.0188217121798087,
0.0818414361465043));
#8850=CARTESIAN_POINT('Ctrl Pts',(0.153918268762738,0.0228328106236434,
0.0821158983468834));
#8851=CARTESIAN_POINT('Ctrl Pts',(0.152787911037918,0.0292909474186763,
0.0825681029008388));
#8852=CARTESIAN_POINT('Ctrl Pts',(0.152295290364591,0.0317529312997165,
0.0827429436213154));
#8853=CARTESIAN_POINT('Ctrl Pts',(0.151570810338119,0.0349672362451497,
0.0829749201731549));
#8854=CARTESIAN_POINT('Ctrl Pts',(0.151392500530438,0.0357313433805167,
0.0830303425629312));
#8855=CARTESIAN_POINT('Ctrl Pts',(0.151091324107297,0.0369792290831497,
0.0831213226498433));
#8856=CARTESIAN_POINT('Ctrl Pts',(0.150971894803402,0.0374638301960137,
0.0831567696267183));
#8857=CARTESIAN_POINT('Ctrl Pts',(0.150736457502403,0.0383997397544758,
0.0832254568595244));
#8858=CARTESIAN_POINT('Ctrl Pts',(0.150620749542859,0.0388511188003107,
0.0832586871131321));
#8859=CARTESIAN_POINT('Ctrl Pts',(0.150349298437739,0.0398906141129895,
0.0833354557927926));
#8860=CARTESIAN_POINT('Ctrl Pts',(0.150192130468377,0.0404783468154918,
0.0833790398548015));
#8861=CARTESIAN_POINT('Ctrl Pts',(0.149761146365117,0.0420529477719267,
0.0834962955242785));
#8862=CARTESIAN_POINT('Ctrl Pts',(0.149481029097176,0.0430380439094717,
0.0835701701675548));
#8863=CARTESIAN_POINT('Ctrl Pts',(0.148557133993372,0.0461692604169829,
0.0838066811538148));
#8864=CARTESIAN_POINT('Ctrl Pts',(0.147876732132729,0.0483041798830264,
0.0839704940352888));
#8865=CARTESIAN_POINT('Ctrl Pts',(0.146901578784998,0.051149958571924,0.0841924081563293));
#8866=CARTESIAN_POINT('Ctrl Pts',(0.146647295184703,0.0518744916966867,
0.084249220159159));
#8867=CARTESIAN_POINT('Ctrl Pts',(0.146326965820198,0.0527660287916067,
0.0843195156183678));
#8868=CARTESIAN_POINT('Ctrl Pts',(0.146265977903483,0.0529348507889367,
0.0843328440527218));
#8869=CARTESIAN_POINT('Ctrl Pts',(0.146181554839517,0.0531672843044193,
0.0843512183737236));
#8870=CARTESIAN_POINT('Ctrl Pts',(0.146158369932953,0.0532309871608371,
0.0843562566718793));
#8871=CARTESIAN_POINT('Ctrl Pts',(0.145107936421894,0.0561112984219894,
0.0845841737184084));
#8872=CARTESIAN_POINT('Ctrl Pts',(0.143999574791482,0.0588974655605329,
0.0848094817287628));
#8873=CARTESIAN_POINT('Ctrl Pts',(0.137103080170915,0.0748731838230996,
0.0861292289374501));
#8874=CARTESIAN_POINT('Ctrl Pts',(0.129586648033349,0.0872381444160453,
0.0872713781692285));
#8875=CARTESIAN_POINT('Ctrl Pts',(0.11900619799879,0.100193495529096,0.088526201729839));
#8876=CARTESIAN_POINT('Ctrl Pts',(0.117494720853587,0.101961776490896,0.0886987074177071));
#8877=CARTESIAN_POINT('Ctrl Pts',(0.115596440733447,0.104084279688444,0.0889066365208618));
#8878=CARTESIAN_POINT('Ctrl Pts',(0.115246877053464,0.104471200524094,0.0889445770185912));
#8879=CARTESIAN_POINT('Ctrl Pts',(0.1146955270513,0.105075337068371,0.089003864028735));
#8880=CARTESIAN_POINT('Ctrl Pts',(0.114495058603682,0.105293741243097,0.0890253068505789));
#8881=CARTESIAN_POINT('Ctrl Pts',(0.114118889685862,0.105701221063637,0.0890653290028614));
#8882=CARTESIAN_POINT('Ctrl Pts',(0.113943345146594,0.105890430236815,0.0890839190988131));
#8883=CARTESIAN_POINT('Ctrl Pts',(0.113541427113537,0.106321477392285,0.0891262857528071));
#8884=CARTESIAN_POINT('Ctrl Pts',(0.113314751734507,0.106563029568117,0.089150038874487));
#8885=CARTESIAN_POINT('Ctrl Pts',(0.112615667305244,0.10730324227165,0.0892228704552363));
#8886=CARTESIAN_POINT('Ctrl Pts',(0.112140716672478,0.107799508512047,0.0892717590913689));
#8887=CARTESIAN_POINT('Ctrl Pts',(0.105410058011079,0.11473961231674,0.0899565808054583));
#8888=CARTESIAN_POINT('Ctrl Pts',(0.0986098782160602,0.120634188275095,
0.0905525431422003));
#8889=CARTESIAN_POINT('Ctrl Pts',(0.0835453215612041,0.131562374809492,
0.0917795091300265));
#8890=CARTESIAN_POINT('Ctrl Pts',(0.0752455179674333,0.136479212827507,
0.0924080151029762));
#8891=CARTESIAN_POINT('Ctrl Pts',(0.0625606422289995,0.142482974006043,
0.0933603769199756));
#8892=CARTESIAN_POINT('Ctrl Pts',(0.0584984990174048,0.144198305232682,
0.0936639678667445));
#8893=CARTESIAN_POINT('Ctrl Pts',(0.0534841057086612,0.146068975430538,
0.0940398198854358));
#8894=CARTESIAN_POINT('Ctrl Pts',(0.0525959262452387,0.146391132309801,
0.09410643001814));
#8895=CARTESIAN_POINT('Ctrl Pts',(0.0512003464698362,0.146882991526082,
0.094211176230548));
#8896=CARTESIAN_POINT('Ctrl Pts',(0.0506949004772042,0.147058205248446,
0.0942491297188462));
#8897=CARTESIAN_POINT('Ctrl Pts',(0.0497968667716964,0.147364330205717,
0.0943165967950538));
#8898=CARTESIAN_POINT('Ctrl Pts',(0.0494046393550158,0.147496289313962,
0.0943460755069624));
#8899=CARTESIAN_POINT('Ctrl Pts',(0.048499469048707,0.147796804847332,0.0944141348913068));
#8900=CARTESIAN_POINT('Ctrl Pts',(0.0479861683694208,0.147964258024481,
0.0944527513980877));
#8901=CARTESIAN_POINT('Ctrl Pts',(0.0465752887030418,0.14841641311634,0.0945589598256062));
#8902=CARTESIAN_POINT('Ctrl Pts',(0.0456759929124442,0.148695638130801,
0.0946267297538776));
#8903=CARTESIAN_POINT('Ctrl Pts',(0.0410682830418304,0.150080556510872,
0.0949743838729365));
#8904=CARTESIAN_POINT('Ctrl Pts',(0.0373223893648925,0.15105565743645,0.0952584556716677));
#8905=CARTESIAN_POINT('Ctrl Pts',(0.0315445934031727,0.152331661586899,
0.0956992788964798));
#8906=CARTESIAN_POINT('Ctrl Pts',(0.0295364100201812,0.152733743243059,
0.0958529679858877));
#8907=CARTESIAN_POINT('Ctrl Pts',(0.013002539994223,0.155705915445292,0.0971219733518095));
#8908=CARTESIAN_POINT('Ctrl Pts',(-0.00181097028508723,0.156237127116136,
0.0982917574966761));
#8909=CARTESIAN_POINT('Ctrl Pts',(-0.0190370354801933,0.15440215264804,
0.0995946714836518));
#8910=CARTESIAN_POINT('Ctrl Pts',(-0.0215906548923594,0.154065827447587,
0.0997860352101843));
#8911=CARTESIAN_POINT('Ctrl Pts',(-0.0246667820386182,0.153582688473664,
0.100013496516563));
#8912=CARTESIAN_POINT('Ctrl Pts',(-0.0251981988019866,0.153496394534569,
0.100052680492912));
#8913=CARTESIAN_POINT('Ctrl Pts',(-0.0260255327087407,0.153357635774511,
0.100113499571183));
#8914=CARTESIAN_POINT('Ctrl Pts',(-0.0263217568898874,0.153307070683407,
0.10013523875439));
#8915=CARTESIAN_POINT('Ctrl Pts',(-0.0268718887738776,0.153211522358686,
0.100175540737239));
#8916=CARTESIAN_POINT('Ctrl Pts',(-0.0271258287181839,0.153166766656477,
0.100194115696471));
#8917=CARTESIAN_POINT('Ctrl Pts',(-0.0277008428175408,0.153063948277369,
0.100236112945029));
#8918=CARTESIAN_POINT('Ctrl Pts',(-0.0280218456686519,0.153005506847545,
0.100259513500185));
#8919=CARTESIAN_POINT('Ctrl Pts',(-0.0289933446315104,0.152825476896183,
0.100330205888139));
#8920=CARTESIAN_POINT('Ctrl Pts',(-0.0296432624678985,0.152700744770797,
0.100377323741381));
#8921=CARTESIAN_POINT('Ctrl Pts',(-0.0346811631386657,0.151700494819882,
0.100741349702883));
#8922=CARTESIAN_POINT('Ctrl Pts',(-0.0390308352015495,0.150640056251004,
0.101048511024141));
#8923=CARTESIAN_POINT('Ctrl Pts',(-0.0502903072525949,0.147374423467926,
0.101839319898168));
#8924=CARTESIAN_POINT('Ctrl Pts',(-0.0570928375707449,0.144874005170402,
0.102313059788725));
#8925=CARTESIAN_POINT('Ctrl Pts',(-0.0636886551490397,0.141913909484965,
0.102789135277549));
#8926=CARTESIAN_POINT('Origin',(0.,0.,-0.129405622560373));
#8927=CARTESIAN_POINT('',(-0.0636885950184591,0.141913936470576,0.186516973639706));
#8928=CARTESIAN_POINT('',(-0.0636886258390813,0.141913922638794,0.172648810545196));
#8929=CARTESIAN_POINT('',(-0.0636886258329924,0.141913922641526,-0.129405622560373));
#8930=CARTESIAN_POINT('',(-0.155549942714367,-0.000133497404892293,0.12945317097425));
#8931=CARTESIAN_POINT('Ctrl Pts',(-0.063688595018437,0.141913936470586,
0.186516973639705));
#8932=CARTESIAN_POINT('Ctrl Pts',(-0.0547516337114912,0.145924694846607,
0.1858638558966));
#8933=CARTESIAN_POINT('Ctrl Pts',(-0.0454464797629655,0.149086491021556,
0.185228745135963));
#8934=CARTESIAN_POINT('Ctrl Pts',(-0.0292704465762964,0.152922845709905,
0.184118833909094));
#8935=CARTESIAN_POINT('Ctrl Pts',(-0.0225507434434849,0.154057132232873,
0.183656424950485));
#8936=CARTESIAN_POINT('Ctrl Pts',(-0.0147816897437891,0.154849310886087,
0.183109322551273));
#8937=CARTESIAN_POINT('Ctrl Pts',(-0.0137834585228433,0.154941355426672,
0.183038802246957));
#8938=CARTESIAN_POINT('Ctrl Pts',(-0.012183990092204,0.155073259663454,
0.182925416882625));
#8939=CARTESIAN_POINT('Ctrl Pts',(-0.0115832776387197,0.155119286801718,
0.182882744753399));
#8940=CARTESIAN_POINT('Ctrl Pts',(-0.0105179303025587,0.155194691857778,
0.182806904164193));
#8941=CARTESIAN_POINT('Ctrl Pts',(-0.0100533995318077,0.1552254759629,0.182773780085784));
#8942=CARTESIAN_POINT('Ctrl Pts',(-0.0090869914159759,0.155285162849253,
0.182704751594438));
#8943=CARTESIAN_POINT('Ctrl Pts',(-0.00858509890767695,0.155313718904405,
0.182668836736412));
#8944=CARTESIAN_POINT('Ctrl Pts',(-0.00728519311551275,0.15538135928089,
0.182575641941608));
#8945=CARTESIAN_POINT('Ctrl Pts',(-0.00648701011967386,0.155416728527545,
0.182518246658301));
#8946=CARTESIAN_POINT('Ctrl Pts',(-0.00305694329666138,0.155542253131225,
0.182270837842607));
#8947=CARTESIAN_POINT('Ctrl Pts',(-0.000423421283886921,0.155571708707789,
0.182078947633174));
#8948=CARTESIAN_POINT('Ctrl Pts',(0.0065303586225725,0.155472927086741,
0.181566769287899));
#8949=CARTESIAN_POINT('Ctrl Pts',(0.0108464483791228,0.155231520348021,
0.181243212047379));
#8950=CARTESIAN_POINT('Ctrl Pts',(0.027498725224259,0.153602276842521,0.179973542688244));
#8951=CARTESIAN_POINT('Ctrl Pts',(0.0396603851378657,0.150920006644976,
0.178996237327103));
#8952=CARTESIAN_POINT('Ctrl Pts',(0.0521330956168747,0.146555759436606,
0.177989540617218));
#8953=CARTESIAN_POINT('Ctrl Pts',(0.0528907209374828,0.146284045492707,
0.17792839330452));
#8954=CARTESIAN_POINT('Ctrl Pts',(0.0566934194818898,0.144886844377341,
0.177621595108224));
#8955=CARTESIAN_POINT('Ctrl Pts',(0.0597051221718255,0.143672000866532,
0.177378971935045));
#8956=CARTESIAN_POINT('Ctrl Pts',(0.0631791836847363,0.142142514713832,
0.177101236362889));
#8957=CARTESIAN_POINT('Ctrl Pts',(0.0636803457653474,0.141918699710725,
0.177061223958485));
#8958=CARTESIAN_POINT('Ctrl Pts',(0.0644832090229408,0.141555038117688,
0.176997221662148));
#8959=CARTESIAN_POINT('Ctrl Pts',(0.0647856585736385,0.141416871380987,
0.176973133507578));
#8960=CARTESIAN_POINT('Ctrl Pts',(0.0653228992149329,0.141169360759828,
0.176930388619169));
#8961=CARTESIAN_POINT('Ctrl Pts',(0.0655578625192123,0.141060399280504,
0.176911708817605));
#8962=CARTESIAN_POINT('Ctrl Pts',(0.0660577780660054,0.14082705040128,0.176871997332508));
#8963=CARTESIAN_POINT('Ctrl Pts',(0.0663226511489675,0.140702502167427,
0.176850975782961));
#8964=CARTESIAN_POINT('Ctrl Pts',(0.067041927429953,0.140361802729578,0.176793938174323));
#8965=CARTESIAN_POINT('Ctrl Pts',(0.0674956413189466,0.140144190463788,
0.176758010962983));
#8966=CARTESIAN_POINT('Ctrl Pts',(0.0698121476504684,0.13901927806143,0.176574803024153));
#8967=CARTESIAN_POINT('Ctrl Pts',(0.0716578485735978,0.138076969476781,
0.176429573657961));
#8968=CARTESIAN_POINT('Ctrl Pts',(0.0770308816922076,0.135197033132444,
0.176007360634448));
#8969=CARTESIAN_POINT('Ctrl Pts',(0.0805026809625757,0.133158996252508,
0.175735262078017));
#8970=CARTESIAN_POINT('Ctrl Pts',(0.0926941724550466,0.125350932158238,
0.17476811721607));
#8971=CARTESIAN_POINT('Ctrl Pts',(0.100905933775115,0.118840521275051,0.174092564810614));
#8972=CARTESIAN_POINT('Ctrl Pts',(0.11306205334004,0.107027949585954,0.172958987921739));
#8973=CARTESIAN_POINT('Ctrl Pts',(0.117432493036791,0.102213511529725,0.17251699971998));
#8974=CARTESIAN_POINT('Ctrl Pts',(0.122110043324089,0.0963635269647403,
0.171992199939395));
#8975=CARTESIAN_POINT('Ctrl Pts',(0.12272377571439,0.0955806821628197,0.171922216851082));
#8976=CARTESIAN_POINT('Ctrl Pts',(0.123695712300763,0.0943161360014855,
0.171809531129689));
#8977=CARTESIAN_POINT('Ctrl Pts',(0.124058717425556,0.0938381445057863,
0.171767017626774));
#8978=CARTESIAN_POINT('Ctrl Pts',(0.12469815147557,0.0929859663466096,0.171691359746565));
#8979=CARTESIAN_POINT('Ctrl Pts',(0.124975686944939,0.0926126156788095,
0.171658259027021));
#8980=CARTESIAN_POINT('Ctrl Pts',(0.125550247248289,0.0918324107704236,
0.171589179339217));
#8981=CARTESIAN_POINT('Ctrl Pts',(0.125846978403247,0.091425348059369,0.171553189517737));
#8982=CARTESIAN_POINT('Ctrl Pts',(0.126611954222842,0.0903651557686301,
0.171459583030827));
#8983=CARTESIAN_POINT('Ctrl Pts',(0.127077118727621,0.089709833240905,0.171401849089149));
#8984=CARTESIAN_POINT('Ctrl Pts',(0.129069537241057,0.0868563270160509,
0.171150967762642));
#8985=CARTESIAN_POINT('Ctrl Pts',(0.130544902077878,0.0846226557958453,
0.170955877687407));
#8986=CARTESIAN_POINT('Ctrl Pts',(0.134302246723993,0.0786018535376741,
0.170432986527685));
#8987=CARTESIAN_POINT('Ctrl Pts',(0.136481509337154,0.074753834456864,0.170101743536016));
#8988=CARTESIAN_POINT('Ctrl Pts',(0.144129260829888,0.0597977821701023,
0.168825938444051));
#8989=CARTESIAN_POINT('Ctrl Pts',(0.148428542713818,0.0481450395304601,
0.167851067287483));
#8990=CARTESIAN_POINT('Ctrl Pts',(0.152202686408833,0.0323298854149088,
0.166613409286367));
#8991=CARTESIAN_POINT('Ctrl Pts',(0.152962356934765,0.0285202210843172,
0.166321906167617));
#8992=CARTESIAN_POINT('Ctrl Pts',(0.153678950619842,0.0240620382810823,
0.165991304140812));
#8993=CARTESIAN_POINT('Ctrl Pts',(0.153775403873182,0.0234377206704377,
0.165945245724463));
#8994=CARTESIAN_POINT('Ctrl Pts',(0.153915635083043,0.0224918882546469,
0.165875845963868));
#8995=CARTESIAN_POINT('Ctrl Pts',(0.153962213322886,0.0221708058992135,
0.165852352608535));
#8996=CARTESIAN_POINT('Ctrl Pts',(0.154043985301968,0.0215944321772633,
0.16581030063509));
#8997=CARTESIAN_POINT('Ctrl Pts',(0.154079549351653,0.0213391982935048,
0.165791721538635));
#8998=CARTESIAN_POINT('Ctrl Pts',(0.154155384443697,0.020784874762471,0.165751463818454));
#8999=CARTESIAN_POINT('Ctrl Pts',(0.154195419341405,0.0204857567646991,
0.165729798643258));
#9000=CARTESIAN_POINT('Ctrl Pts',(0.154305253530392,0.01964657151326,0.165669174756813));
#9001=CARTESIAN_POINT('Ctrl Pts',(0.154373088639696,0.0191062441838966,
0.165630324681178));
#9002=CARTESIAN_POINT('Ctrl Pts',(0.154758007033303,0.0159042908461808,
0.165401129271739));
#9003=CARTESIAN_POINT('Ctrl Pts',(0.155009112345932,0.0132349776210906,
0.165214262687112));
#9004=CARTESIAN_POINT('Ctrl Pts',(0.156185481362583,-0.00405260664255331,
0.16402332579295));
#9005=CARTESIAN_POINT('Ctrl Pts',(0.155111150311053,-0.0187340395242954,
0.163094510693396));
#9006=CARTESIAN_POINT('Ctrl Pts',(0.151570014298421,-0.0350199697808364,
0.161974577435958));
#9007=CARTESIAN_POINT('Ctrl Pts',(0.1511033827012,-0.0369815462714318,0.161838293118428));
#9008=CARTESIAN_POINT('Ctrl Pts',(0.149623767401304,-0.0427048585837868,
0.161435745818667));
#9009=CARTESIAN_POINT('Ctrl Pts',(0.148507518051081,-0.046438017014586,
0.161166855466282));
#9010=CARTESIAN_POINT('Ctrl Pts',(0.14694833090306,-0.0510184385412151,
0.160827116432248));
#9011=CARTESIAN_POINT('Ctrl Pts',(0.146636119344421,-0.0519089728275574,
0.160760596641834));
#9012=CARTESIAN_POINT('Ctrl Pts',(0.14613242602927,-0.053304864116192,0.160655566323352));
#9013=CARTESIAN_POINT('Ctrl Pts',(0.145946376804749,-0.0538121692539915,
0.160617236041259));
#9014=CARTESIAN_POINT('Ctrl Pts',(0.145613203190448,-0.0547062039999561,
0.160549399037869));
#9015=CARTESIAN_POINT('Ctrl Pts',(0.145467171046953,-0.0550933375372713,
0.160519928967588));
#9016=CARTESIAN_POINT('Ctrl Pts',(0.145128992844146,-0.0559791346927276,
0.160452277246934));
#9017=CARTESIAN_POINT('Ctrl Pts',(0.144935819022094,-0.0564773975687085,
0.160414061513008));
#9018=CARTESIAN_POINT('Ctrl Pts',(0.144394878721728,-0.0578516182988463,
0.160308208370373));
#9019=CARTESIAN_POINT('Ctrl Pts',(0.144041717908249,-0.0587254133255446,
0.160240390613471));
#9020=CARTESIAN_POINT('Ctrl Pts',(0.142005700518275,-0.0636340757980171,
0.159856463657057));
#9021=CARTESIAN_POINT('Ctrl Pts',(0.140161435160248,-0.0675994054020957,
0.159534930030714));
#9022=CARTESIAN_POINT('Ctrl Pts',(0.133794953660373,-0.079903954863038,
0.15849919757464));
#9023=CARTESIAN_POINT('Ctrl Pts',(0.128676549976145,-0.0879092219880076,
0.157766253588319));
#9024=CARTESIAN_POINT('Ctrl Pts',(0.117240305671925,-0.102637907989317,
0.156320146337081));
#9025=CARTESIAN_POINT('Ctrl Pts',(0.110988697852455,-0.109368111070109,
0.155610275487766));
#9026=CARTESIAN_POINT('Ctrl Pts',(0.103671966195352,-0.115967209706039,
0.154888199958129));
#9027=CARTESIAN_POINT('Ctrl Pts',(0.103161038849738,-0.11642194987081,0.154838300314794));
#9028=CARTESIAN_POINT('Ctrl Pts',(0.102398636310875,-0.11709155029266,0.154764633015736));
#9029=CARTESIAN_POINT('Ctrl Pts',(0.102149458068934,-0.117308994071282,
0.154740680295833));
#9030=CARTESIAN_POINT('Ctrl Pts',(0.101704498029839,-0.117694792793475,
0.154698131151275));
#9031=CARTESIAN_POINT('Ctrl Pts',(0.101508989280126,-0.117863456038336,
0.15467951213126));
#9032=CARTESIAN_POINT('Ctrl Pts',(0.101087460535421,-0.118225277387001,
0.154639533007339));
#9033=CARTESIAN_POINT('Ctrl Pts',(0.100861307056234,-0.118418274069846,
0.15461818474709));
#9034=CARTESIAN_POINT('Ctrl Pts',(0.100234965217823,-0.118949690716906,
0.154559333214837));
#9035=CARTESIAN_POINT('Ctrl Pts',(0.099833612621343,-0.11928674270848,0.154521928579502));
#9036=CARTESIAN_POINT('Ctrl Pts',(0.0976178700080409,-0.121128485461158,
0.15431705865648));
#9037=CARTESIAN_POINT('Ctrl Pts',(0.0957710359323388,-0.122593918440155,
0.154152267516732));
#9038=CARTESIAN_POINT('Ctrl Pts',(0.0822858271866923,-0.132803381906686,
0.15298514996007));
#9039=CARTESIAN_POINT('Ctrl Pts',(0.0695030731198153,-0.139918307065511,
0.152061634398111));
#9040=CARTESIAN_POINT('Ctrl Pts',(0.053715630839533,-0.145999976098753,
0.150927747879091));
#9041=CARTESIAN_POINT('Ctrl Pts',(0.0514964701124916,-0.146797393795023,
0.1507686848099));
#9042=CARTESIAN_POINT('Ctrl Pts',(0.0454757451872059,-0.148807516398727,
0.150336782986503));
#9043=CARTESIAN_POINT('Ctrl Pts',(0.041644476239146,-0.149924825345288,
0.150061532498368));
#9044=CARTESIAN_POINT('Ctrl Pts',(0.0369341827546044,-0.151104002260415,
0.149720629425166));
#9045=CARTESIAN_POINT('Ctrl Pts',(0.0360918751996719,-0.151307401819402,
0.149659574805439));
#9046=CARTESIAN_POINT('Ctrl Pts',(0.0346949562912331,-0.151632400349437,
0.149558144119532));
#9047=CARTESIAN_POINT('Ctrl Pts',(0.0341412919989688,-0.151758021181475,
0.149517897102319));
#9048=CARTESIAN_POINT('Ctrl Pts',(0.0331373830802062,-0.151980026139405,
0.149444833196336));
#9049=CARTESIAN_POINT('Ctrl Pts',(0.0326873724276947,-0.152077447960423,
0.149412049888066));
#9050=CARTESIAN_POINT('Ctrl Pts',(0.0322357549628178,-0.152173120502424,
0.149379116121447));
#9051=CARTESIAN_POINT('Ctrl Pts',(0.0322345696545825,-0.152173371588628,
0.149379029683759));
#9052=CARTESIAN_POINT('Ctrl Pts',(0.0322322059491332,-0.152173872268217,
0.149378857311907));
#9053=CARTESIAN_POINT('Ctrl Pts',(0.0322310273115069,-0.152174121912682,
0.149378771360213));
#9054=CARTESIAN_POINT('Ctrl Pts',(0.0322286765883317,-0.152174619785296,
0.149378599934177));
#9055=CARTESIAN_POINT('Ctrl Pts',(0.032227504492861,-0.152174868015706,
0.149378514459115));
#9056=CARTESIAN_POINT('Ctrl Pts',(0.0322251667920374,-0.152175363073805,
0.149378343981833));
#9057=CARTESIAN_POINT('Ctrl Pts',(0.0322240011816163,-0.152175609902724,
0.149378258979246));
#9058=CARTESIAN_POINT('Ctrl Pts',(0.0322216764117314,-0.152176102166605,
0.149378089444066));
#9059=CARTESIAN_POINT('Ctrl Pts',(0.0322205172390236,-0.152176347604524,
0.14937800491051));
#9060=CARTESIAN_POINT('Ctrl Pts',(0.0322182052855862,-0.152176837099355,
0.149377836309097));
#9061=CARTESIAN_POINT('Ctrl Pts',(0.0322170524981316,-0.152177081157842,
0.149377752240753));
#9062=CARTESIAN_POINT('Ctrl Pts',(0.0322147532554497,-0.152177567906913,
0.149377584565415));
#9063=CARTESIAN_POINT('Ctrl Pts',(0.0322136067977378,-0.152177810598173,
0.149377500958242));
#9064=CARTESIAN_POINT('Ctrl Pts',(0.0322113201784562,-0.152178294620877,
0.149377334202621));
#9065=CARTESIAN_POINT('Ctrl Pts',(0.0322101800056327,-0.152178535954852,
0.149377251053355));
#9066=CARTESIAN_POINT('Ctrl Pts',(0.0316991731472682,-0.152286691905048,
0.149339984813314));
#9067=CARTESIAN_POINT('Ctrl Pts',(0.0311887731469123,-0.152392042203614,
0.149302720145424));
#9068=CARTESIAN_POINT('Ctrl Pts',(0.0298080652547318,-0.152669803513008,
0.14920179291402));
#9069=CARTESIAN_POINT('Ctrl Pts',(0.0289368074588397,-0.15283733435398,
0.149137976075716));
#9070=CARTESIAN_POINT('Ctrl Pts',(0.0269987402217567,-0.153192832351303,
0.14899571243784));
#9071=CARTESIAN_POINT('Ctrl Pts',(0.0259313131540722,-0.153377125886362,
0.14891715259092));
#9072=CARTESIAN_POINT('Ctrl Pts',(0.0226807515252329,-0.15390344023369,
0.148677258912362));
#9073=CARTESIAN_POINT('Ctrl Pts',(0.0204922597599656,-0.154210089745347,
0.148514839253952));
#9074=CARTESIAN_POINT('Ctrl Pts',(0.00334991008706172,-0.156240723797499,
0.147235129313097));
#9075=CARTESIAN_POINT('Ctrl Pts',(-0.0117747635777276,-0.155831865596905,
0.146050435500232));
#9076=CARTESIAN_POINT('Ctrl Pts',(-0.0275831092416756,-0.153088111616821,
0.144821713065297));
#9077=CARTESIAN_POINT('Ctrl Pts',(-0.0285644318820091,-0.152908047983781,
0.144745526597874));
#9078=CARTESIAN_POINT('Ctrl Pts',(-0.033316046149697,-0.151988830537548,
0.144377239524371));
#9079=CARTESIAN_POINT('Ctrl Pts',(-0.0370602039367026,-0.151119525722049,
0.144088885480912));
#9080=CARTESIAN_POINT('Ctrl Pts',(-0.0413767562929535,-0.149947202565584,
0.143761406030212));
#9081=CARTESIAN_POINT('Ctrl Pts',(-0.0419838287918148,-0.149778361838437,
0.143715466170576));
#9082=CARTESIAN_POINT('Ctrl Pts',(-0.0429015796008725,-0.149517096023816,
0.143646209426549));
#9083=CARTESIAN_POINT('Ctrl Pts',(-0.0432130126092813,-0.149427383976584,
0.143622741448045));
#9084=CARTESIAN_POINT('Ctrl Pts',(-0.0437715520658734,-0.149264597703823,
0.143580716442843));
#9085=CARTESIAN_POINT('Ctrl Pts',(-0.0440187580466708,-0.149191882625673,
0.143562139056385));
#9086=CARTESIAN_POINT('Ctrl Pts',(-0.0445553513344724,-0.149032595101734,
0.143521863778969));
#9087=CARTESIAN_POINT('Ctrl Pts',(-0.044844666728571,-0.14894579418543,
0.143500179431414));
#9088=CARTESIAN_POINT('Ctrl Pts',(-0.0456560346319368,-0.148699787765839,
0.143439448914677));
#9089=CARTESIAN_POINT('Ctrl Pts',(-0.0461775118148835,-0.148538674446524,
0.143400511992213));
#9090=CARTESIAN_POINT('Ctrl Pts',(-0.0492387501123485,-0.147575208140343,
0.143172441492734));
#9091=CARTESIAN_POINT('Ctrl Pts',(-0.0517586103782475,-0.146710412426594,
0.142986739257247));
#9092=CARTESIAN_POINT('Ctrl Pts',(-0.0598780282123614,-0.143688619595042,
0.142391194917996));
#9093=CARTESIAN_POINT('Ctrl Pts',(-0.0653756183348194,-0.141272218880717,
0.141992282973149));
#9094=CARTESIAN_POINT('Ctrl Pts',(-0.0790854035657697,-0.134274008029409,
0.140976151871489));
#9095=CARTESIAN_POINT('Ctrl Pts',(-0.0870461432685281,-0.129255440921728,
0.140364125473848));
#9096=CARTESIAN_POINT('Ctrl Pts',(-0.0947018146792362,-0.123399472859138,
0.139713436755087));
#9097=CARTESIAN_POINT('Ctrl Pts',(-0.094897796896862,-0.123248820475764,
0.139696735638923));
#9098=CARTESIAN_POINT('Ctrl Pts',(-0.0988960640349475,-0.120160144704847,
0.139355107221391));
#9099=CARTESIAN_POINT('Ctrl Pts',(-0.102560181859405,-0.117048251170178,
0.139025129970639));
#9100=CARTESIAN_POINT('Ctrl Pts',(-0.106746225794824,-0.1131454378215,0.138623658493219));
#9101=CARTESIAN_POINT('Ctrl Pts',(-0.107412724808465,-0.112512902842904,
0.138558956493561));
#9102=CARTESIAN_POINT('Ctrl Pts',(-0.108493486143699,-0.111468860443686,
0.138452728031849));
#9103=CARTESIAN_POINT('Ctrl Pts',(-0.108911111739892,-0.111060853170497,
0.138411353057405));
#9104=CARTESIAN_POINT('Ctrl Pts',(-0.109654962538559,-0.110325903559971,
0.138337064354729));
#9105=CARTESIAN_POINT('Ctrl Pts',(-0.109982049150166,-0.109999839372421,
0.138304189398948));
#9106=CARTESIAN_POINT('Ctrl Pts',(-0.110612332679272,-0.109365904511675,
0.13824043187762));
#9107=CARTESIAN_POINT('Ctrl Pts',(-0.110915708781466,-0.109058217246394,
0.138209557626091));
#9108=CARTESIAN_POINT('Ctrl Pts',(-0.111732858885005,-0.10822251847518,
0.138125889618168));
#9109=CARTESIAN_POINT('Ctrl Pts',(-0.112244164516321,-0.107692120218288,
0.138072989202101));
#9110=CARTESIAN_POINT('Ctrl Pts',(-0.114282925617486,-0.105546937631989,
0.137859818366441));
#9111=CARTESIAN_POINT('Ctrl Pts',(-0.115779387778606,-0.103903202772636,
0.137698235865585));
#9112=CARTESIAN_POINT('Ctrl Pts',(-0.119510575186018,-0.0996240972743058,
0.137281744278447));
#9113=CARTESIAN_POINT('Ctrl Pts',(-0.121693547429822,-0.0969454253964503,
0.137024860209447));
#9114=CARTESIAN_POINT('Ctrl Pts',(-0.127357582082388,-0.0895022097005319,
0.136321064310843));
#9115=CARTESIAN_POINT('Ctrl Pts',(-0.130659527387109,-0.0846089561619116,
0.135868700006317));
#9116=CARTESIAN_POINT('Ctrl Pts',(-0.139358985047391,-0.069988681580578,
0.134553029944301));
#9117=CARTESIAN_POINT('Ctrl Pts',(-0.14400283269987,-0.0598545485013284,
0.133681893259836));
#9118=CARTESIAN_POINT('Ctrl Pts',(-0.147891748703495,-0.0482198853745478,
0.132775143719688));
#9119=CARTESIAN_POINT('Ctrl Pts',(-0.14824443707268,-0.0471244497882592,
0.132690669564868));
#9120=CARTESIAN_POINT('Ctrl Pts',(-0.148709580649979,-0.0456228072575893,
0.132576187301951));
#9121=CARTESIAN_POINT('Ctrl Pts',(-0.148832578676592,-0.0452199453212849,
0.132545602567902));
#9122=CARTESIAN_POINT('Ctrl Pts',(-0.149025148762318,-0.0445799127353224,
0.132497221464874));
#9123=CARTESIAN_POINT('Ctrl Pts',(-0.14909579337474,-0.0443430714251948,
0.132479363601522));
#9124=CARTESIAN_POINT('Ctrl Pts',(-0.149240270165681,-0.0438544536130575,
0.132442616626082));
#9125=CARTESIAN_POINT('Ctrl Pts',(-0.149314029828064,-0.0436026586176383,
0.132423732196678));
#9126=CARTESIAN_POINT('Ctrl Pts',(-0.14948779402618,-0.0430038642967888,
0.132378944388203));
#9127=CARTESIAN_POINT('Ctrl Pts',(-0.149587228795776,-0.0426566981327582,
0.132353074050867));
#9128=CARTESIAN_POINT('Ctrl Pts',(-0.149795204919668,-0.0419209004237031,
0.132298441345078));
#9129=CARTESIAN_POINT('Ctrl Pts',(-0.149903445211676,-0.0415321855005446,
0.132269695981004));
#9130=CARTESIAN_POINT('Ctrl Pts',(-0.150195983137838,-0.0404655735940405,
0.132191128173938));
#9131=CARTESIAN_POINT('Ctrl Pts',(-0.15037720589022,-0.0397868319028949,
0.132141471370438));
#9132=CARTESIAN_POINT('Ctrl Pts',(-0.153859449839334,-0.0263808711836664,
0.131166952599816));
#9133=CARTESIAN_POINT('Ctrl Pts',(-0.155538655392449,-0.0132853806131935,
0.130322903296383));
#9134=CARTESIAN_POINT('Ctrl Pts',(-0.155549942714367,-0.000133497404892293,
0.12945317097425));
#9135=CARTESIAN_POINT('Ctrl Pts',(-0.155549942819317,-0.000133375062712872,
0.129453162883777));
#9136=CARTESIAN_POINT('Ctrl Pts',(-0.155555805801239,0.00670438369198078,
0.129000982730695));
#9137=CARTESIAN_POINT('Ctrl Pts',(-0.15511080758718,0.0135345765403181,
0.128543991051104));
#9138=CARTESIAN_POINT('Ctrl Pts',(-0.153889036609665,0.0228103386093192,
0.127900308785973));
#9139=CARTESIAN_POINT('Ctrl Pts',(-0.153499510118162,0.0252991361586018,
0.127725349529218));
#9140=CARTESIAN_POINT('Ctrl Pts',(-0.152927239502439,0.0284522860789925,
0.127500326413089));
#9141=CARTESIAN_POINT('Ctrl Pts',(-0.152800265776766,0.0291264813650497,
0.127452016581095));
#9142=CARTESIAN_POINT('Ctrl Pts',(-0.152575058385035,0.0302802523595054,
0.127368995110126));
#9143=CARTESIAN_POINT('Ctrl Pts',(-0.152479012274388,0.0307602491876375,
0.127334352818693));
#9144=CARTESIAN_POINT('Ctrl Pts',(-0.152294159988247,0.0316619175589571,
0.12726907925613));
#9145=CARTESIAN_POINT('Ctrl Pts',(-0.152205863943051,0.0320836900085918,
0.12723846445441));
#9146=CARTESIAN_POINT('Ctrl Pts',(-0.15201824844092,0.0329616844614085,
0.127174560832495));
#9147=CARTESIAN_POINT('Ctrl Pts',(-0.151918625268515,0.0334178363955861,
0.127141262607256));
#9148=CARTESIAN_POINT('Ctrl Pts',(-0.15168388345004,0.0344699200981673,
0.127064232807068));
#9149=CARTESIAN_POINT('Ctrl Pts',(-0.151547304691091,0.0350655145577277,
0.127020454924969));
#9150=CARTESIAN_POINT('Ctrl Pts',(-0.151170654181454,0.0366647057491829,
0.12690244209779));
#9151=CARTESIAN_POINT('Ctrl Pts',(-0.150924102806883,0.0376667284193124,
0.126828000522904));
#9152=CARTESIAN_POINT('Ctrl Pts',(-0.148639944313082,0.046567232605343,
0.126162222061261));
#9153=CARTESIAN_POINT('Ctrl Pts',(-0.145994319561966,0.0542950834051834,
0.125551126060616));
#9154=CARTESIAN_POINT('Ctrl Pts',(-0.140446089421772,0.0671156830038609,
0.124480997822295));
#9155=CARTESIAN_POINT('Ctrl Pts',(-0.137839138849583,0.072318636030586,
0.124029726649834));
#9156=CARTESIAN_POINT('Ctrl Pts',(-0.131829396085029,0.0828016316060835,
0.123092878355514));
#9157=CARTESIAN_POINT('Ctrl Pts',(-0.128385455108062,0.0880470720303393,
0.122608181432154));
#9158=CARTESIAN_POINT('Ctrl Pts',(-0.123043581632665,0.0952005544037684,
0.121936086612204));
#9159=CARTESIAN_POINT('Ctrl Pts',(-0.12139862353349,0.0972894909191922,
0.121738402845313));
#9160=CARTESIAN_POINT('Ctrl Pts',(-0.119352307386806,0.0997553357799539,
0.121504285668986));
#9161=CARTESIAN_POINT('Ctrl Pts',(-0.119001600882609,0.100173446114688,
0.121464561512281));
#9162=CARTESIAN_POINT('Ctrl Pts',(-0.118453381361028,0.100820088103071,
0.121403093998487));
#9163=CARTESIAN_POINT('Ctrl Pts',(-0.118257395637145,0.101049899071366,
0.121381242869438));
#9164=CARTESIAN_POINT('Ctrl Pts',(-0.117892967677068,0.101474711469062,
0.121340841395603));
#9165=CARTESIAN_POINT('Ctrl Pts',(-0.117724711838345,0.101669863381236,
0.121322278333307));
#9166=CARTESIAN_POINT('Ctrl Pts',(-0.117343725813944,0.102109537029153,
0.121280447758162));
#9167=CARTESIAN_POINT('Ctrl Pts',(-0.117130716333378,0.102353812027828,
0.121257201277273));
#9168=CARTESIAN_POINT('Ctrl Pts',(-0.116501310208449,0.103071064350553,
0.121188919361571));
#9169=CARTESIAN_POINT('Ctrl Pts',(-0.116082794324041,0.103542186981093,
0.121144037342716));
#9170=CARTESIAN_POINT('Ctrl Pts',(-0.113091338590442,0.106868727399821,
0.120826794204234));
#9171=CARTESIAN_POINT('Ctrl Pts',(-0.110415935172786,0.109630758853381,
0.120561605863823));
#9172=CARTESIAN_POINT('Ctrl Pts',(-0.106527884950608,0.113357789048688,
0.120196224490214));
#9173=CARTESIAN_POINT('Ctrl Pts',(-0.10539928090054,0.114407912574821,0.120092377707706));
#9174=CARTESIAN_POINT('Ctrl Pts',(-0.101295536149757,0.118114016999504,
0.119721818812999));
#9175=CARTESIAN_POINT('Ctrl Pts',(-0.0982340339323089,0.120672215885626,
0.119458303932637));
#9176=CARTESIAN_POINT('Ctrl Pts',(-0.0888463985780042,0.127922258405213,
0.1186767935642));
#9177=CARTESIAN_POINT('Ctrl Pts',(-0.0822592730425939,0.132254265392426,
0.118161557082653));
#9178=CARTESIAN_POINT('Ctrl Pts',(-0.0720657925292953,0.137900744710627,
0.117378082407623));
#9179=CARTESIAN_POINT('Ctrl Pts',(-0.0686934037247811,0.139611269791126,
0.117121065525822));
#9180=CARTESIAN_POINT('Ctrl Pts',(-0.0647390242514229,0.14143900980572,
0.116820229350733));
#9181=CARTESIAN_POINT('Ctrl Pts',(-0.0642144734262393,0.14167793092233,
0.116780334887106));
#9182=CARTESIAN_POINT('Ctrl Pts',(-0.0636886257863082,0.141913922662477,
0.116740348554263));
#9183=CARTESIAN_POINT('Ctrl Pts',(-0.0636886551490397,0.141913909484965,
0.102789135277549));
#9184=CARTESIAN_POINT('Ctrl Pts',(-0.0706385455446796,0.138794911676096,
0.103290767172019));
#9185=CARTESIAN_POINT('Ctrl Pts',(-0.0773589325761553,0.135165584427428,
0.103795169971365));
#9186=CARTESIAN_POINT('Ctrl Pts',(-0.0869787906224297,0.129014663481055,
0.104573891824348));
#9187=CARTESIAN_POINT('Ctrl Pts',(-0.0900881810529839,0.12686295364493,
0.104835181778715));
#9188=CARTESIAN_POINT('Ctrl Pts',(-0.0938384349741554,0.124060324867915,
0.105164181681259));
#9189=CARTESIAN_POINT('Ctrl Pts',(-0.0945562316998756,0.123514108790094,
0.105227803857689));
#9190=CARTESIAN_POINT('Ctrl Pts',(-0.0956845658241266,0.122639889221374,
0.105328874323912));
#9191=CARTESIAN_POINT('Ctrl Pts',(-0.0960982697677787,0.122315988736132,
0.105366160660117));
#9192=CARTESIAN_POINT('Ctrl Pts',(-0.0968715270618784,0.121704239348659,
0.105436288563915));
#9193=CARTESIAN_POINT('Ctrl Pts',(-0.0972314593618795,0.121416876638781,
0.105469110516049));
#9194=CARTESIAN_POINT('Ctrl Pts',(-0.0980350073753849,0.120769475653918,
0.105542791609919));
#9195=CARTESIAN_POINT('Ctrl Pts',(-0.098477924362814,0.120408584901165,
0.105583684721936));
#9196=CARTESIAN_POINT('Ctrl Pts',(-0.0995967513221978,0.119486657152731,
0.105687702708321));
#9197=CARTESIAN_POINT('Ctrl Pts',(-0.100269907734776,0.118922326143927,
0.105750960580353));
#9198=CARTESIAN_POINT('Ctrl Pts',(-0.104109502649637,0.115647680672805,
0.106115722098118));
#9199=CARTESIAN_POINT('Ctrl Pts',(-0.107170473938427,0.112816922366711,
0.106422163583893));
#9200=CARTESIAN_POINT('Ctrl Pts',(-0.111360857793215,0.108617120598283,
0.106865248268274));
#9201=CARTESIAN_POINT('Ctrl Pts',(-0.112586450099176,0.107346217333874,
0.1069979209144));
#9202=CARTESIAN_POINT('Ctrl Pts',(-0.12384338939518,0.0952682286987803,
0.108245627673472));
#9203=CARTESIAN_POINT('Ctrl Pts',(-0.132310477421477,0.0831088504158885,
0.109415149140087));
#9204=CARTESIAN_POINT('Ctrl Pts',(-0.140084268475597,0.0676659855061544,
0.110715156732754));
#9205=CARTESIAN_POINT('Ctrl Pts',(-0.141173384041356,0.0653633348979577,
0.110904371977293));
#9206=CARTESIAN_POINT('Ctrl Pts',(-0.142422875056337,0.0625445024681927,
0.111129599785222));
#9207=CARTESIAN_POINT('Ctrl Pts',(-0.142637675483297,0.0620530715100431,
0.111168633544894));
#9208=CARTESIAN_POINT('Ctrl Pts',(-0.14296862570722,0.0612851083708011,
0.111229259908833));
#9209=CARTESIAN_POINT('Ctrl Pts',(-0.143086521887947,0.0610093411109938,
0.111250955742889));
#9210=CARTESIAN_POINT('Ctrl Pts',(-0.143304259411854,0.0604959351692327,
0.11129120712845));
#9211=CARTESIAN_POINT('Ctrl Pts',(-0.143404306649491,0.0602583917290455,
0.111309774674413));
#9212=CARTESIAN_POINT('Ctrl Pts',(-0.143629797761343,0.0597192630568167,
0.111351789720478));
#9213=CARTESIAN_POINT('Ctrl Pts',(-0.143754882240401,0.0594175312712788,
0.111375215322197));
#9214=CARTESIAN_POINT('Ctrl Pts',(-0.144131302840691,0.0585013736832179,
0.111446080995303));
#9215=CARTESIAN_POINT('Ctrl Pts',(-0.144379661478246,0.0578857199578396,
0.11149334570905));
#9216=CARTESIAN_POINT('Ctrl Pts',(-0.146297497227193,0.0530424759419743,
0.11186252198048));
#9217=CARTESIAN_POINT('Ctrl Pts',(-0.147785087627223,0.0487446373652794,
0.112174367869767));
#9218=CARTESIAN_POINT('Ctrl Pts',(-0.153364496529452,0.0300052360032902,
0.113492463580175));
#9219=CARTESIAN_POINT('Ctrl Pts',(-0.155543053855193,0.0150793605078501,
0.114446301523442));
#9220=CARTESIAN_POINT('Ctrl Pts',(-0.155550077037969,-0.000130914471409132,
0.115485075421146));
#9221=CARTESIAN_POINT('Ctrl Pts',(-0.15554977427191,-0.000333650716531503,
0.115498931426319));
#9222=CARTESIAN_POINT('Ctrl Pts',(-0.155545683823176,-0.0015198766800267,
0.115580065613003));
#9223=CARTESIAN_POINT('Ctrl Pts',(-0.155532964948277,-0.00250330332611001,
0.115647577023153));
#9224=CARTESIAN_POINT('Ctrl Pts',(-0.155460202960187,-0.00574873535517704,
0.115871280317847));
#9225=CARTESIAN_POINT('Ctrl Pts',(-0.155360130892678,-0.00800946243452763,
0.116028569190131));
#9226=CARTESIAN_POINT('Ctrl Pts',(-0.15515259455218,-0.0111468487396825,
0.116249262821473));
#9227=CARTESIAN_POINT('Ctrl Pts',(-0.155086922608274,-0.0120260638629871,
0.116311372687011));
#9228=CARTESIAN_POINT('Ctrl Pts',(-0.154966303389103,-0.0134749703139348,
0.116414182947297));
#9229=CARTESIAN_POINT('Ctrl Pts',(-0.154915679293732,-0.0140450099368733,
0.116454747896279));
#9230=CARTESIAN_POINT('Ctrl Pts',(-0.154818637195961,-0.0150732946732276,
0.116528138660411));
#9231=CARTESIAN_POINT('Ctrl Pts',(-0.154773327121212,-0.015531639932309,
0.116560929371149));
#9232=CARTESIAN_POINT('Ctrl Pts',(-0.154672056728187,-0.0165115888872842,
0.116631205947826));
#9233=CARTESIAN_POINT('Ctrl Pts',(-0.154615492142895,-0.0170331229394871,
0.116668710403071));
#9234=CARTESIAN_POINT('Ctrl Pts',(-0.154454891891054,-0.0184471184536732,
0.116770678309198));
#9235=CARTESIAN_POINT('Ctrl Pts',(-0.154345761308043,-0.0193389687322384,
0.116835301005697));
#9236=CARTESIAN_POINT('Ctrl Pts',(-0.153743151429852,-0.0239331731630626,
0.117169831901331));
#9237=CARTESIAN_POINT('Ctrl Pts',(-0.153124203003052,-0.0276175197948567,
0.117443652502398));
#9238=CARTESIAN_POINT('Ctrl Pts',(-0.149374584530788,-0.0458854074301121,
0.118830662725052));
#9239=CARTESIAN_POINT('Ctrl Pts',(-0.144290258070929,-0.0599866995284198,
0.12000600546946));
#9240=CARTESIAN_POINT('Ctrl Pts',(-0.135162584725455,-0.077117738665688,
0.121489934379906));
#9241=CARTESIAN_POINT('Ctrl Pts',(-0.13287388269345,-0.0809975966507191,
0.121829326261002));
#9242=CARTESIAN_POINT('Ctrl Pts',(-0.130058755849486,-0.0853285498316267,
0.122207707320979));
#9243=CARTESIAN_POINT('Ctrl Pts',(-0.129694153688685,-0.0858817089419614,
0.122256024792016));
#9244=CARTESIAN_POINT('Ctrl Pts',(-0.129144677336626,-0.0867038714488613,
0.122327804337203));
#9245=CARTESIAN_POINT('Ctrl Pts',(-0.128962479095646,-0.0869746399787034,
0.122351438296505));
#9246=CARTESIAN_POINT('Ctrl Pts',(-0.128634863998955,-0.0874582225768048,
0.122393634613066));
#9247=CARTESIAN_POINT('Ctrl Pts',(-0.128489769814232,-0.0876712495002865,
0.122412218121612));
#9248=CARTESIAN_POINT('Ctrl Pts',(-0.12817456538751,-0.088131568544732,
0.122452363684521));
#9249=CARTESIAN_POINT('Ctrl Pts',(-0.128004269168859,-0.0883787285783763,
0.122473912839279));
#9250=CARTESIAN_POINT('Ctrl Pts',(-0.127527134651975,-0.0890669473196047,
0.122533903784023));
#9251=CARTESIAN_POINT('Ctrl Pts',(-0.127218720921191,-0.0895069173154188,
0.122572240524891));
#9252=CARTESIAN_POINT('Ctrl Pts',(-0.125426776620938,-0.0920352555871656,
0.122792517972867));
#9253=CARTESIAN_POINT('Ctrl Pts',(-0.123894007031203,-0.0940884777344814,
0.122971287695339));
#9254=CARTESIAN_POINT('Ctrl Pts',(-0.113207281920229,-0.107689555128207,
0.124161840311325));
#9255=CARTESIAN_POINT('Ctrl Pts',(-0.102502498883451,-0.11792487910962,
0.125095824726007));
#9256=CARTESIAN_POINT('Ctrl Pts',(-0.0890095334445175,-0.127579531110364,
0.126210421160723));
#9257=CARTESIAN_POINT('Ctrl Pts',(-0.0874839894727898,-0.12863042024781,
0.126335537418819));
#9258=CARTESIAN_POINT('Ctrl Pts',(-0.0825409520511248,-0.131906877151387,
0.126738774955476));
#9259=CARTESIAN_POINT('Ctrl Pts',(-0.0790548178875261,-0.134025235668758,
0.127019978917594));
#9260=CARTESIAN_POINT('Ctrl Pts',(-0.0747268648359269,-0.136427487850475,
0.127367469037761));
#9261=CARTESIAN_POINT('Ctrl Pts',(-0.0739604589619583,-0.13684448919969,
0.127428941143569));
#9262=CARTESIAN_POINT('Ctrl Pts',(-0.0726880633310731,-0.137522988267405,
0.127530916425332));
#9263=CARTESIAN_POINT('Ctrl Pts',(-0.0721840657197892,-0.137788197946449,
0.127571288046938));
#9264=CARTESIAN_POINT('Ctrl Pts',(-0.0712699716560731,-0.138262813737666,
0.127644477611306));
#9265=CARTESIAN_POINT('Ctrl Pts',(-0.0708603781886651,-0.138473179053262,
0.127677261372564));
#9266=CARTESIAN_POINT('Ctrl Pts',(-0.069980228040502,-0.138920292451442,
0.127747687074279));
#9267=CARTESIAN_POINT('Ctrl Pts',(-0.0695093919410487,-0.139156474483865,
0.127785348316346));
#9268=CARTESIAN_POINT('Ctrl Pts',(-0.0682237139890469,-0.139793246569915,
0.127888157680868));
#9269=CARTESIAN_POINT('Ctrl Pts',(-0.0674065608818435,-0.140189095232688,
0.127953469464895));
#9270=CARTESIAN_POINT('Ctrl Pts',(-0.0630960554115809,-0.142230807515395,
0.128297872962092));
#9271=CARTESIAN_POINT('Ctrl Pts',(-0.0595460741624127,-0.143753173753649,
0.128581157103115));
#9272=CARTESIAN_POINT('Ctrl Pts',(-0.0421081658824659,-0.150474436659898,
0.129972576881888));
#9273=CARTESIAN_POINT('Ctrl Pts',(-0.0275824082838605,-0.153800898223667,
0.13114129354303));
#9274=CARTESIAN_POINT('Ctrl Pts',(-0.00838123767623072,-0.155387607567937,
0.132613616267623));
#9275=CARTESIAN_POINT('Ctrl Pts',(-0.00393791286297731,-0.15556367088544,
0.132948527677967));
#9276=CARTESIAN_POINT('Ctrl Pts',(0.00116806411789234,-0.155547017669804,
0.133322537632243));
#9277=CARTESIAN_POINT('Ctrl Pts',(0.00182879797403608,-0.155540652627275,
0.133370726395007));
#9278=CARTESIAN_POINT('Ctrl Pts',(0.00281550095454516,-0.155524858999269,
0.133442356247465));
#9279=CARTESIAN_POINT('Ctrl Pts',(0.00314150183058143,-0.155518615554276,
0.133465968105366));
#9280=CARTESIAN_POINT('Ctrl Pts',(0.00372517554819278,-0.155505601200461,
0.13350814297036));
#9281=CARTESIAN_POINT('Ctrl Pts',(0.00398285225734731,-0.155499214882348,
0.1335267270211));
#9282=CARTESIAN_POINT('Ctrl Pts',(0.00454083203693389,-0.155483997890049,
0.133566893148311));
#9283=CARTESIAN_POINT('Ctrl Pts',(0.00484112495049768,-0.155474937751516,
0.133588462238073));
#9284=CARTESIAN_POINT('Ctrl Pts',(0.00567968161233166,-0.155447205790621,
0.133648565287772));
#9285=CARTESIAN_POINT('Ctrl Pts',(0.00621788457832035,-0.155426608100472,
0.133686993559254));
#9286=CARTESIAN_POINT('Ctrl Pts',(0.00933626859016975,-0.155291039856502,
0.133908853816108));
#9287=CARTESIAN_POINT('Ctrl Pts',(0.0119135682168439,-0.155114609135302,
0.134089061214026));
#9288=CARTESIAN_POINT('Ctrl Pts',(0.0291399058049222,-0.153503418054419,
0.135279603111998));
#9289=CARTESIAN_POINT('Ctrl Pts',(0.0435270414129684,-0.150059786605862,
0.13621260504786));
#9290=CARTESIAN_POINT('Ctrl Pts',(0.0589601803972402,-0.143954902099785,
0.137327611070788));
#9291=CARTESIAN_POINT('Ctrl Pts',(0.0606907156997419,-0.143233911310728,
0.137454243946822));
#9292=CARTESIAN_POINT('Ctrl Pts',(0.0661193951893142,-0.140856122829706,
0.137857310731186));
#9293=CARTESIAN_POINT('Ctrl Pts',(0.0697657881507205,-0.13908613041145,
0.138136764490696));
#9294=CARTESIAN_POINT('Ctrl Pts',(0.0741064250623704,-0.136765486042756,
0.138482306125629));
#9295=CARTESIAN_POINT('Ctrl Pts',(0.0748706950355498,-0.136348595071883,
0.138543643759503));
#9296=CARTESIAN_POINT('Ctrl Pts',(0.0761285374417257,-0.135648707823806,
0.138645440343138));
#9297=CARTESIAN_POINT('Ctrl Pts',(0.0766241359575988,-0.135369375858926,
0.138685768526715));
#9298=CARTESIAN_POINT('Ctrl Pts',(0.0775180035234204,-0.134859087870266,
0.138758909283748));
#9299=CARTESIAN_POINT('Ctrl Pts',(0.0779168026918441,-0.134629069302972,
0.138791687864545));
#9300=CARTESIAN_POINT('Ctrl Pts',(0.078770020180844,-0.13413189139421,0.138862135586966));
#9301=CARTESIAN_POINT('Ctrl Pts',(0.0792241121522437,-0.133864186432881,
0.138899824172253));
#9302=CARTESIAN_POINT('Ctrl Pts',(0.0804582186444308,-0.133128153684733,
0.139002792480867));
#9303=CARTESIAN_POINT('Ctrl Pts',(0.0812354882759923,-0.13265528873801,
0.139068236751931));
#9304=CARTESIAN_POINT('Ctrl Pts',(0.0853118684529381,-0.130126093320621,
0.13941464773595));
#9305=CARTESIAN_POINT('Ctrl Pts',(0.0885368940020133,-0.127953618400233,
0.139699865841379));
#9306=CARTESIAN_POINT('Ctrl Pts',(0.103637272725672,-0.116937183228877,
0.141091840840225));
#9307=CARTESIAN_POINT('Ctrl Pts',(0.11428966313307,-0.10654912072968,0.142258824418465));
#9308=CARTESIAN_POINT('Ctrl Pts',(0.1260177190381,-0.0912965134908927,0.143729114425927));
#9309=CARTESIAN_POINT('Ctrl Pts',(0.128572703051685,-0.0876617820074358,
0.144063723923184));
#9310=CARTESIAN_POINT('Ctrl Pts',(0.131325279211541,-0.0833661195061936,
0.144437433129076));
#9311=CARTESIAN_POINT('Ctrl Pts',(0.131678127393583,-0.082807666611234,
0.14448560873573));
#9312=CARTESIAN_POINT('Ctrl Pts',(0.132199785065882,-0.0819702726658703,
0.144557221078397));
#9313=CARTESIAN_POINT('Ctrl Pts',(0.132371286333957,-0.081693031110227,
0.144580828507199));
#9314=CARTESIAN_POINT('Ctrl Pts',(0.132676812490045,-0.0811956424406442,
0.144622997045343));
#9315=CARTESIAN_POINT('Ctrl Pts',(0.132811162379304,-0.0809757005209628,
0.144641579184054));
#9316=CARTESIAN_POINT('Ctrl Pts',(0.133100936291169,-0.0804986553469477,
0.144681743273674));
#9317=CARTESIAN_POINT('Ctrl Pts',(0.13325616190262,-0.0802414361374415,
0.144703312229576));
#9318=CARTESIAN_POINT('Ctrl Pts',(0.133687596400143,-0.0795218156850044,
0.144763417137694));
#9319=CARTESIAN_POINT('Ctrl Pts',(0.133962153944662,-0.0790584210221566,
0.144801847379823));
#9320=CARTESIAN_POINT('Ctrl Pts',(0.135539619336425,-0.076364181691027,
0.145023760204471));
#9321=CARTESIAN_POINT('Ctrl Pts',(0.136789294943068,-0.0741024125780319,
0.145204016194217));
#9322=CARTESIAN_POINT('Ctrl Pts',(0.144776204159051,-0.0587557354086258,
0.146394483986495));
#9323=CARTESIAN_POINT('Ctrl Pts',(0.149683989514654,-0.044801767878852,
0.147327385335938));
#9324=CARTESIAN_POINT('Ctrl Pts',(0.152922665071086,-0.0285299791630497,
0.148441992503164));
#9325=CARTESIAN_POINT('Ctrl Pts',(0.153254666718231,-0.026689097881679,
0.14856834276781));
#9326=CARTESIAN_POINT('Ctrl Pts',(0.154201303969297,-0.0208379144722291,
0.148971439284641));
#9327=CARTESIAN_POINT('Ctrl Pts',(0.154692251054584,-0.0168096217345331,
0.149251217219409));
#9328=CARTESIAN_POINT('Ctrl Pts',(0.155096657365621,-0.0118990686046017,
0.149597117011384));
#9329=CARTESIAN_POINT('Ctrl Pts',(0.155160845717928,-0.011030542182039,
0.149658476653839));
#9330=CARTESIAN_POINT('Ctrl Pts',(0.155254906593456,-0.00959376006181592,
0.149760301869139));
#9331=CARTESIAN_POINT('Ctrl Pts',(0.155288960858057,-0.00902578935509894,
0.149800636539955));
#9332=CARTESIAN_POINT('Ctrl Pts',(0.155344929875334,-0.00799795057847217,
0.149873783726313));
#9333=CARTESIAN_POINT('Ctrl Pts',(0.155367920773401,-0.00753814550303406,
0.1499065622167));
#9334=CARTESIAN_POINT('Ctrl Pts',(0.15541285306968,-0.00655174644955265,
0.149977003829522));
#9335=CARTESIAN_POINT('Ctrl Pts',(0.155434159908823,-0.0060251308377031,
0.150014686369657));
#9336=CARTESIAN_POINT('Ctrl Pts',(0.155484937423368,-0.0045895362622885,
0.15011762309413));
#9337=CARTESIAN_POINT('Ctrl Pts',(0.155509112833656,-0.00368040338539662,
0.150183041662213));
#9338=CARTESIAN_POINT('Ctrl Pts',(0.1555944850618,0.00111098136566404,0.150529081178344));
#9339=CARTESIAN_POINT('Ctrl Pts',(0.155518273397871,0.00499396816634459,
0.150813942742622));
#9340=CARTESIAN_POINT('Ctrl Pts',(0.154452482579347,0.0236545031885006,
0.152205798608921));
#9341=CARTESIAN_POINT('Ctrl Pts',(0.151500880857875,0.0382418732409599,
0.153373084026912));
#9342=CARTESIAN_POINT('Ctrl Pts',(0.145044118074665,0.0563713509820373,
0.154843732628452));
#9343=CARTESIAN_POINT('Ctrl Pts',(0.143375461416402,0.0604897642121254,
0.155178398590222));
#9344=CARTESIAN_POINT('Ctrl Pts',(0.141258570236774,0.0651325971259948,
0.155552163182417));
#9345=CARTESIAN_POINT('Ctrl Pts',(0.140980686608145,0.0657319170508707,
0.155600340546433));
#9346=CARTESIAN_POINT('Ctrl Pts',(0.14055997408423,0.0666243383575321,0.155671955038173));
#9347=CARTESIAN_POINT('Ctrl Pts',(0.140420033035468,0.0669187799033785,
0.155695562871136));
#9348=CARTESIAN_POINT('Ctrl Pts',(0.140167800177061,0.0674452127238864,
0.15573773207893));
#9349=CARTESIAN_POINT('Ctrl Pts',(0.140055857030071,0.0676773657950092,
0.155756314483062));
#9350=CARTESIAN_POINT('Ctrl Pts',(0.139812174826001,0.0681795315913519,
0.155796479226402));
#9351=CARTESIAN_POINT('Ctrl Pts',(0.13968023073895,0.068449440483249,0.155818048570095));
#9352=CARTESIAN_POINT('Ctrl Pts',(0.139309555190041,0.0692021707518959,
0.155878154041943));
#9353=CARTESIAN_POINT('Ctrl Pts',(0.139069093580581,0.0696841433729341,
0.155916584463651));
#9354=CARTESIAN_POINT('Ctrl Pts',(0.137660855033631,0.072470442480767,0.156138488983379));
#9355=CARTESIAN_POINT('Ctrl Pts',(0.136438234202659,0.0747468152831139,
0.15631873690612));
#9356=CARTESIAN_POINT('Ctrl Pts',(0.127874780907324,0.0897799784498791,
0.157509242008481));
#9357=CARTESIAN_POINT('Ctrl Pts',(0.118811545855129,0.101470833689925,0.158442183290816));
#9358=CARTESIAN_POINT('Ctrl Pts',(0.106893470341627,0.113018133323992,0.159557040303562));
#9359=CARTESIAN_POINT('Ctrl Pts',(0.105524545501431,0.11429734191863,0.159683595479395));
#9360=CARTESIAN_POINT('Ctrl Pts',(0.101121530682333,0.118265258634068,0.160086693782468));
#9361=CARTESIAN_POINT('Ctrl Pts',(0.0980054928101562,0.120860058956407,
0.160366260603895));
#9362=CARTESIAN_POINT('Ctrl Pts',(0.094101552809794,0.123860640956834,0.160711927862183));
#9363=CARTESIAN_POINT('Ctrl Pts',(0.0934067752787468,0.124385428795347,
0.160773273949869));
#9364=CARTESIAN_POINT('Ctrl Pts',(0.0922507889961369,0.125243435454709,
0.160875081962068));
#9365=CARTESIAN_POINT('Ctrl Pts',(0.0917920857036551,0.125580011074519,
0.160915413072385));
#9366=CARTESIAN_POINT('Ctrl Pts',(0.0909588761914181,0.126184378200024,
0.160988557380435));
#9367=CARTESIAN_POINT('Ctrl Pts',(0.0905850060835521,0.12645303920516,0.161021336574019));
#9368=CARTESIAN_POINT('Ctrl Pts',(0.0897805339143425,0.127025729993788,
0.161091783670405));
#9369=CARTESIAN_POINT('Ctrl Pts',(0.0893495692330081,0.127329237866431,
0.161129471008738));
#9370=CARTESIAN_POINT('Ctrl Pts',(0.0881706474560099,0.128150563790848,
0.16123243097855));
#9371=CARTESIAN_POINT('Ctrl Pts',(0.0874196874277055,0.128664013062905,
0.161297868107159));
#9372=CARTESIAN_POINT('Ctrl Pts',(0.0857538929141479,0.129781640612057,
0.161442720110232));
#9373=CARTESIAN_POINT('Ctrl Pts',(0.0848370946983941,0.130382788889746,
0.161522244269175));
#9374=CARTESIAN_POINT('Ctrl Pts',(0.0820218871204731,0.132186468348424,
0.16176587904077));
#9375=CARTESIAN_POINT('Ctrl Pts',(0.0801037812441496,0.133357548151939,
0.161931115291894));
#9376=CARTESIAN_POINT('Ctrl Pts',(0.0650421375642345,0.142111089809795,
0.163223215049242));
#9377=CARTESIAN_POINT('Ctrl Pts',(0.050879186398803,0.147774078272349,0.164418481600227));
#9378=CARTESIAN_POINT('Ctrl Pts',(0.0347539700387688,0.151624383686798,
0.165686709717775));
#9379=CARTESIAN_POINT('Ctrl Pts',(0.0333775532430762,0.15193331209725,0.165794162855451));
#9380=CARTESIAN_POINT('Ctrl Pts',(0.0287818774268354,0.152899314435191,
0.166149914789407));
#9381=CARTESIAN_POINT('Ctrl Pts',(0.0255457471264085,0.153473175890718,
0.166395528692922));
#9382=CARTESIAN_POINT('Ctrl Pts',(0.0217486045534025,0.154023062962571,
0.16667626967173));
#9383=CARTESIAN_POINT('Ctrl Pts',(0.0212032050239982,0.154099090994946,
0.166716414963485));
#9384=CARTESIAN_POINT('Ctrl Pts',(0.0203273623986443,0.154216444388624,
0.166780584531424));
#9385=CARTESIAN_POINT('Ctrl Pts',(0.0199971770621088,0.154259606822837,
0.166804707909536));
#9386=CARTESIAN_POINT('Ctrl Pts',(0.0194099426809959,0.154334454025935,
0.166847487464418));
#9387=CARTESIAN_POINT('Ctrl Pts',(0.01915295057938,0.154366557461666,0.166866166886917));
#9388=CARTESIAN_POINT('Ctrl Pts',(0.0186057947031262,0.154433520679718,
0.166905846112276));
#9389=CARTESIAN_POINT('Ctrl Pts',(0.0183156131141099,0.154468204579988,
0.166926835921389));
#9390=CARTESIAN_POINT('Ctrl Pts',(0.0175272744608783,0.154560177885348,
0.166983717073892));
#9391=CARTESIAN_POINT('Ctrl Pts',(0.017028929414945,0.154615877320389,0.167019520352928));
#9392=CARTESIAN_POINT('Ctrl Pts',(0.0145473139817467,0.154881100729164,
0.167197084292279));
#9393=CARTESIAN_POINT('Ctrl Pts',(0.0125602941128886,0.155054892639742,
0.167336952961936));
#9394=CARTESIAN_POINT('Ctrl Pts',(0.00675750056292725,0.155450133505772,
0.16774015847685));
#9395=CARTESIAN_POINT('Ctrl Pts',(0.00293604720025901,0.155569252188962,
0.167999091479927));
#9396=CARTESIAN_POINT('Ctrl Pts',(-0.0157568263655786,0.155462752540304,
0.169250138880972));
#9397=CARTESIAN_POINT('Ctrl Pts',(-0.0305377273157059,0.153246232063803,
0.170199377360572));
#9398=CARTESIAN_POINT('Ctrl Pts',(-0.0465836892157773,0.148422745643242,
0.171351101493234));
#9399=CARTESIAN_POINT('Ctrl Pts',(-0.0483777548045196,0.147847704941779,
0.171481521519002));
#9400=CARTESIAN_POINT('Ctrl Pts',(-0.0515087282835301,0.146781064760352,
0.17171233302246));
#9401=CARTESIAN_POINT('Ctrl Pts',(-0.0528501750027187,0.146303413587647,
0.171812271354078));
#9402=CARTESIAN_POINT('Ctrl Pts',(-0.0547165074119037,0.145609848661826,
0.171952870023323));
#9403=CARTESIAN_POINT('Ctrl Pts',(-0.0552470865653726,0.145409365658874,
0.171993018146018));
#9404=CARTESIAN_POINT('Ctrl Pts',(-0.0562163050216766,0.145037069284581,
0.17206668871895));
#9405=CARTESIAN_POINT('Ctrl Pts',(-0.0566552848764634,0.144866155825285,
0.172100180800954));
#9406=CARTESIAN_POINT('Ctrl Pts',(-0.0574960644800473,0.144534398606088,
0.172164572023355));
#9407=CARTESIAN_POINT('Ctrl Pts',(-0.0578979832298198,0.14437386654816,
0.172195460436706));
#9408=CARTESIAN_POINT('Ctrl Pts',(-0.0589058701179005,0.143966416677378,
0.172273192262356));
#9409=CARTESIAN_POINT('Ctrl Pts',(-0.0595109549000239,0.143717350685,0.172320107727856));
#9410=CARTESIAN_POINT('Ctrl Pts',(-0.0613123071259736,0.142962548624937,
0.172460533182733));
#9411=CARTESIAN_POINT('Ctrl Pts',(-0.0625037940408128,0.14244565559127,
0.172554418520559));
#9412=CARTESIAN_POINT('Ctrl Pts',(-0.0636886258390813,0.141913922638794,
0.172648810545196));
#9413=CARTESIAN_POINT('Origin',(0.,0.,-0.129405622560373));
#9414=CARTESIAN_POINT('',(-0.0636886236493968,0.141913923621488,0.256547255026181));
#9415=CARTESIAN_POINT('',(-0.0636886300394901,0.141913920753719,0.24285329779702));
#9416=CARTESIAN_POINT('',(-0.0636886258329924,0.141913922641526,-0.129405622560373));
#9417=CARTESIAN_POINT('Ctrl Pts',(-0.0636886236493968,0.141913923621488,
0.256547255026181));
#9418=CARTESIAN_POINT('Ctrl Pts',(-0.0596258587468564,0.143737225368426,
0.256203084221599));
#9419=CARTESIAN_POINT('Ctrl Pts',(-0.0554857265475,0.145385644314302,0.255861098235132));
#9420=CARTESIAN_POINT('Ctrl Pts',(-0.0487210271369214,0.147747786242891,
0.255321422368869));
#9421=CARTESIAN_POINT('Ctrl Pts',(-0.0461393551279011,0.148574254700172,
0.25511980497706));
#9422=CARTESIAN_POINT('Ctrl Pts',(-0.0430107014145476,0.149486396793805,
0.254881685933237));
#9423=CARTESIAN_POINT('Ctrl Pts',(-0.042483383832882,0.149637112325167,
0.254841762452393));
#9424=CARTESIAN_POINT('Ctrl Pts',(-0.0416638641902283,0.149866662404458,
0.254780053494691));
#9425=CARTESIAN_POINT('Ctrl Pts',(-0.0413722178174534,0.149947436379034,
0.254758158912198));
#9426=CARTESIAN_POINT('Ctrl Pts',(-0.0408318511512882,0.150095399012549,
0.25471771689295));
#9427=CARTESIAN_POINT('Ctrl Pts',(-0.0405832019144654,0.150162820290285,
0.254699156528942));
#9428=CARTESIAN_POINT('Ctrl Pts',(-0.0400220919321353,0.150313469826336,
0.254657382146159));
#9429=CARTESIAN_POINT('Ctrl Pts',(-0.0397095391888852,0.150396341565945,
0.25463418890867));
#9430=CARTESIAN_POINT('Ctrl Pts',(-0.0387905117082392,0.150636952264702,
0.254566209070282));
#9431=CARTESIAN_POINT('Ctrl Pts',(-0.03818332966159,0.150792004290077,0.254521573856897));
#9432=CARTESIAN_POINT('Ctrl Pts',(-0.0339295689682465,0.151850917634577,
0.254210701831179));
#9433=CARTESIAN_POINT('Ctrl Pts',(-0.0302518548848313,0.152626170763884,
0.253951313406448));
#9434=CARTESIAN_POINT('Ctrl Pts',(-0.0255057473517231,0.153448300871223,
0.253624265643544));
#9435=CARTESIAN_POINT('Ctrl Pts',(-0.0244603498923309,0.153618408929923,
0.253552702985084));
#9436=CARTESIAN_POINT('Ctrl Pts',(-0.00851377657193091,0.156046337069236,
0.252467194721703));
#9437=CARTESIAN_POINT('Ctrl Pts',(0.00663601846216799,0.156137586936553,
0.251508635130492));
#9438=CARTESIAN_POINT('Ctrl Pts',(0.0237559746747839,0.153741209671331,
0.250325505914376));
#9439=CARTESIAN_POINT('Ctrl Pts',(0.0259420532007912,0.153387466740599,
0.250172719422126));
#9440=CARTESIAN_POINT('Ctrl Pts',(0.0291867268719838,0.15279108081497,0.249942966645793));
#9441=CARTESIAN_POINT('Ctrl Pts',(0.030251599433257,0.152583813134891,0.249867082809595));
#9442=CARTESIAN_POINT('Ctrl Pts',(0.0321851572007719,0.152186427693648,
0.249728368169083));
#9443=CARTESIAN_POINT('Ctrl Pts',(0.033054553059676,0.151999965728812,0.249665654071608));
#9444=CARTESIAN_POINT('Ctrl Pts',(0.0344309252335927,0.151692404289917,
0.249565802787035));
#9445=CARTESIAN_POINT('Ctrl Pts',(0.0349389836902074,0.151576190539167,
0.249528821935665));
#9446=CARTESIAN_POINT('Ctrl Pts',(0.0354475720214446,0.151457162719788,
0.249491676815272));
#9447=CARTESIAN_POINT('Ctrl Pts',(0.0354487011050552,0.151456898460613,
0.249491594351204));
#9448=CARTESIAN_POINT('Ctrl Pts',(0.0354509655190462,0.151456368453513,
0.24949142896558));
#9449=CARTESIAN_POINT('Ctrl Pts',(0.0354521008360992,0.15145610270856,0.249491346044991));
#9450=CARTESIAN_POINT('Ctrl Pts',(0.0354543777614074,0.151455569719061,
0.24949117974306));
#9451=CARTESIAN_POINT('Ctrl Pts',(0.0354555193611961,0.151455302476347,
0.249491096362329));
#9452=CARTESIAN_POINT('Ctrl Pts',(0.0354578089034049,0.151454766478837,
0.249490929136336));
#9453=CARTESIAN_POINT('Ctrl Pts',(0.0354589568386282,0.151454497725573,
0.249490845291593));
#9454=CARTESIAN_POINT('Ctrl Pts',(0.0354612590898024,0.151453958697588,
0.249490677134772));
#9455=CARTESIAN_POINT('Ctrl Pts',(0.0354624134048996,0.151453688422913,
0.249490592822749));
#9456=CARTESIAN_POINT('Ctrl Pts',(0.035464728492523,0.151453146333684,0.249490423725745));
#9457=CARTESIAN_POINT('Ctrl Pts',(0.0354658892492579,0.151452874522671,
0.249490338941909));
#9458=CARTESIAN_POINT('Ctrl Pts',(0.0354682172506913,0.151452329353148,
0.249490168899028));
#9459=CARTESIAN_POINT('Ctrl Pts',(0.0354693844937416,0.151452055994865,
0.249490083640095));
#9460=CARTESIAN_POINT('Ctrl Pts',(0.035471725536426,0.151451507714256,0.249489912641983));
#9461=CARTESIAN_POINT('Ctrl Pts',(0.0354728993247909,0.151451232794408,
0.249489826903621));
#9462=CARTESIAN_POINT('Ctrl Pts',(0.0354752534239846,0.15145068139818,0.249489654949119));
#9463=CARTESIAN_POINT('Ctrl Pts',(0.0354764337314762,0.151450404922424,
0.249489568733218));
#9464=CARTESIAN_POINT('Ctrl Pts',(0.0359259530510062,0.151345103770182,
0.249456733205643));
#9465=CARTESIAN_POINT('Ctrl Pts',(0.0363738187839839,0.151238089899761,
0.249423920402388));
#9466=CARTESIAN_POINT('Ctrl Pts',(0.0373733284774284,0.150994568651274,
0.24935046878823));
#9467=CARTESIAN_POINT('Ctrl Pts',(0.0379247103895052,0.150857024263675,
0.24930979702264));
#9468=CARTESIAN_POINT('Ctrl Pts',(0.0393166063561113,0.150501697175272,
0.249206734811483));
#9469=CARTESIAN_POINT('Ctrl Pts',(0.0401560640196117,0.150279895041299,
0.249144215627597));
#9470=CARTESIAN_POINT('Ctrl Pts',(0.0448670077661596,0.148992876200802,
0.248791279934466));
#9471=CARTESIAN_POINT('Ctrl Pts',(0.0486976212035569,0.147785187826468,
0.248496291899387));
#9472=CARTESIAN_POINT('Ctrl Pts',(0.0542724639820242,0.14578731141018,0.248054556541746));
#9473=CARTESIAN_POINT('Ctrl Pts',(0.0560559470143578,0.14511089137054,0.247911321550669));
#9474=CARTESIAN_POINT('Ctrl Pts',(0.0714907385975114,0.138929949042804,
0.246655105097999));
#9475=CARTESIAN_POINT('Ctrl Pts',(0.084307089362347,0.131547304337279,0.245487849135746));
#9476=CARTESIAN_POINT('Ctrl Pts',(0.0979359571737378,0.12087627570952,0.244185706443168));
#9477=CARTESIAN_POINT('Ctrl Pts',(0.0999374137352741,0.119226847729202,
0.243992984120682));
#9478=CARTESIAN_POINT('Ctrl Pts',(0.102304333794042,0.11717472701326,0.243764139692011));
#9479=CARTESIAN_POINT('Ctrl Pts',(0.102709991048182,0.11681930972974,0.243724885080256));
#9480=CARTESIAN_POINT('Ctrl Pts',(0.103338892288381,0.116262488471385,0.243663985705807));
#9481=CARTESIAN_POINT('Ctrl Pts',(0.103563409379002,0.116062539722903,0.243642236295117));
#9482=CARTESIAN_POINT('Ctrl Pts',(0.103979378092587,0.115689921329102,0.243601927256693));
#9483=CARTESIAN_POINT('Ctrl Pts',(0.104170978245185,0.115517428377475,0.243583355411083));
#9484=CARTESIAN_POINT('Ctrl Pts',(0.104603862476082,0.115125760392618,0.243541383448499));
#9485=CARTESIAN_POINT('Ctrl Pts',(0.104844886554169,0.114906303219695,0.243518004977626));
#9486=CARTESIAN_POINT('Ctrl Pts',(0.105571883313801,0.11424016648358,0.243447454848087));
#9487=CARTESIAN_POINT('Ctrl Pts',(0.106055712961506,0.113791141897657,0.243400456155864));
#9488=CARTESIAN_POINT('Ctrl Pts',(0.109757603991422,0.110311430203864,0.243040360589159));
#9489=CARTESIAN_POINT('Ctrl Pts',(0.112848388530236,0.107147531994782,0.242736776146803));
#9490=CARTESIAN_POINT('Ctrl Pts',(0.125673865399182,0.0928469784568871,
0.241440426676367));
#9491=CARTESIAN_POINT('Ctrl Pts',(0.133927058098072,0.0804864806074241,
0.240500175752082));
#9492=CARTESIAN_POINT('Ctrl Pts',(0.142002245479188,0.0636121967864243,
0.239225803629711));
#9493=CARTESIAN_POINT('Ctrl Pts',(0.143559070248352,0.0600161493556608,
0.238955246419852));
#9494=CARTESIAN_POINT('Ctrl Pts',(0.145308947749686,0.0555152612595681,
0.238615950133217));
#9495=CARTESIAN_POINT('Ctrl Pts',(0.145631987607913,0.0546622232524051,
0.238551618546124));
#9496=CARTESIAN_POINT('Ctrl Pts',(0.14613005648988,0.0533112334902872,0.238449670528884));
#9497=CARTESIAN_POINT('Ctrl Pts',(0.146310089472281,0.0528151373388031,
0.238412220858117));
#9498=CARTESIAN_POINT('Ctrl Pts',(0.146642474551011,0.05188447944842,0.238341936945519));
#9499=CARTESIAN_POINT('Ctrl Pts',(0.146795428728212,0.0514501374750816,
0.238309123085164));
#9500=CARTESIAN_POINT('Ctrl Pts',(0.147132889565193,0.0504780988835804,
0.238235656765934));
#9501=CARTESIAN_POINT('Ctrl Pts',(0.147316380973068,0.0499400594697156,
0.23819497129149));
#9502=CARTESIAN_POINT('Ctrl Pts',(0.147772863138489,0.0485771383314743,
0.238091851192322));
#9503=CARTESIAN_POINT('Ctrl Pts',(0.148041896144577,0.0477509620593361,
0.238029287576418));
#9504=CARTESIAN_POINT('Ctrl Pts',(0.149517951399497,0.0430857277075011,
0.237675655393155));
#9505=CARTESIAN_POINT('Ctrl Pts',(0.150582446166689,0.0392035597913857,
0.237379994151165));
#9506=CARTESIAN_POINT('Ctrl Pts',(0.151926003049149,0.0334350038671785,
0.236938157212352));
#9507=CARTESIAN_POINT('Ctrl Pts',(0.152322908894079,0.0315775362257211,
0.236795520633883));
#9508=CARTESIAN_POINT('Ctrl Pts',(0.155498428181152,0.0152597312852637,
0.235539474234401));
#9509=CARTESIAN_POINT('Ctrl Pts',(0.15624439241789,0.000482274377844819,
0.234371745700547));
#9510=CARTESIAN_POINT('Ctrl Pts',(0.154666742041082,-0.0167537689945947,
0.233069796527146));
#9511=CARTESIAN_POINT('Ctrl Pts',(0.154366823993576,-0.0193229306758924,
0.232877599284345));
#9512=CARTESIAN_POINT('Ctrl Pts',(0.153927139774798,-0.0224171485201451,
0.232649294187079));
#9513=CARTESIAN_POINT('Ctrl Pts',(0.153848551614192,-0.0229502962151324,
0.232610070700915));
#9514=CARTESIAN_POINT('Ctrl Pts',(0.153721819580926,-0.0237801390687977,
0.232549209020646));
#9515=CARTESIAN_POINT('Ctrl Pts',(0.153675584934285,-0.0240771142101452,
0.232527466384051));
#9516=CARTESIAN_POINT('Ctrl Pts',(0.153588090315213,-0.0246285907801381,
0.232487163479456));
#9517=CARTESIAN_POINT('Ctrl Pts',(0.153547058770791,-0.0248831210898303,
0.232468591026818));
#9518=CARTESIAN_POINT('Ctrl Pts',(0.153452696495623,-0.0254593552739257,
0.232426609519356));
#9519=CARTESIAN_POINT('Ctrl Pts',(0.153398986985806,-0.0257809935757978,
0.232403222152111));
#9520=CARTESIAN_POINT('Ctrl Pts',(0.153233396958214,-0.0267537860532619,
0.232332618625719));
#9521=CARTESIAN_POINT('Ctrl Pts',(0.153118376956247,-0.0274044100732752,
0.232285575818465));
#9522=CARTESIAN_POINT('Ctrl Pts',(0.15219851451412,-0.0324210472492138,
0.231924090080054));
#9523=CARTESIAN_POINT('Ctrl Pts',(0.151211139808182,-0.0367520416818871,
0.231619242733859));
#9524=CARTESIAN_POINT('Ctrl Pts',(0.146129659764793,-0.0553317303273859,
0.230319548948886));
#9525=CARTESIAN_POINT('Ctrl Pts',(0.140196585757463,-0.0689959663259818,
0.229377205379866));
#9526=CARTESIAN_POINT('Ctrl Pts',(0.130388495262271,-0.0849094890022917,
0.228103274816019));
#9527=CARTESIAN_POINT('Ctrl Pts',(0.128235763064192,-0.0881269866405828,
0.227835911822118));
#9528=CARTESIAN_POINT('Ctrl Pts',(0.12543228587363,-0.0919965760411361,
0.22750015845956));
#9529=CARTESIAN_POINT('Ctrl Pts',(0.124892691580831,-0.0927277944839427,
0.227436063992362));
#9530=CARTESIAN_POINT('Ctrl Pts',(0.124030105616744,-0.0938755193746218,
0.227334407001755));
#9531=CARTESIAN_POINT('Ctrl Pts',(0.123711344706754,-0.0942951929610783,
0.227297009617457));
#9532=CARTESIAN_POINT('Ctrl Pts',(0.123110027680156,-0.0950785764644416,
0.227226772408556));
#9533=CARTESIAN_POINT('Ctrl Pts',(0.122827976138389,-0.0954426680645701,
0.227193952707544));
#9534=CARTESIAN_POINT('Ctrl Pts',(0.12219355263619,-0.0962541558679592,
0.227120406433537));
#9535=CARTESIAN_POINT('Ctrl Pts',(0.1218403338052,-0.0967008783310393,0.227079646514371));
#9536=CARTESIAN_POINT('Ctrl Pts',(0.120939961857918,-0.0978268309344642,
0.226976211906629));
#9537=CARTESIAN_POINT('Ctrl Pts',(0.120389540524285,-0.0985034095837423,
0.226913406849116));
#9538=CARTESIAN_POINT('Ctrl Pts',(0.117237690786658,-0.102311787731468,
0.226556120251975));
#9539=CARTESIAN_POINT('Ctrl Pts',(0.11452002201463,-0.105344847460616,0.226256934656299));
#9540=CARTESIAN_POINT('Ctrl Pts',(0.110394105753442,-0.109601062977842,
0.225814568179489));
#9541=CARTESIAN_POINT('Ctrl Pts',(0.109077725997197,-0.110911229363431,
0.225675066286808));
#9542=CARTESIAN_POINT('Ctrl Pts',(0.0970953577860628,-0.122417365791118,
0.224419809700923));
#9543=CARTESIAN_POINT('Ctrl Pts',(0.0850542719953016,-0.131069497372375,
0.223249495071439));
#9544=CARTESIAN_POINT('Ctrl Pts',(0.0697168198519296,-0.139075022750094,
0.221948578382555));
#9545=CARTESIAN_POINT('Ctrl Pts',(0.0674288166643111,-0.140198622146559,
0.221759229396775));
#9546=CARTESIAN_POINT('Ctrl Pts',(0.0646267639890398,-0.141490182649355,
0.221533852407647));
#9547=CARTESIAN_POINT('Ctrl Pts',(0.0641382974053375,-0.141712276245282,
0.221494799560585));
#9548=CARTESIAN_POINT('Ctrl Pts',(0.0633749083746817,-0.14205461454463,
0.221434144565686));
#9549=CARTESIAN_POINT('Ctrl Pts',(0.0631007771810436,-0.142176595993263,
0.221412439098915));
#9550=CARTESIAN_POINT('Ctrl Pts',(0.0625903893861014,-0.142401938731089,
0.221372169732452));
#9551=CARTESIAN_POINT('Ctrl Pts',(0.0623542311269034,-0.142505504666513,
0.221353593830727));
#9552=CARTESIAN_POINT('Ctrl Pts',(0.0618182166993383,-0.142738983358968,
0.221311559413954));
#9553=CARTESIAN_POINT('Ctrl Pts',(0.0615182085670214,-0.142868538545967,
0.221288122815917));
#9554=CARTESIAN_POINT('Ctrl Pts',(0.0606072280412788,-0.143258533839776,
0.221217223426876));
#9555=CARTESIAN_POINT('Ctrl Pts',(0.0599949829821342,-0.143516011887271,
0.221169936131201));
#9556=CARTESIAN_POINT('Ctrl Pts',(0.0551767173472634,-0.145506098425994,
0.220800483957709));
#9557=CARTESIAN_POINT('Ctrl Pts',(0.0508976762024639,-0.147057577975895,
0.220488398728771));
#9558=CARTESIAN_POINT('Ctrl Pts',(0.0322029590506205,-0.152921748668273,
0.219167604578315));
#9559=CARTESIAN_POINT('Ctrl Pts',(0.0172725964325838,-0.155318366635986,
0.218211498471092));
#9560=CARTESIAN_POINT('Ctrl Pts',(-0.00134619254742183,-0.155585281866863,
0.216939416396649));
#9561=CARTESIAN_POINT('Ctrl Pts',(-0.00492252785037709,-0.155513206634467,
0.216691943320553));
#9562=CARTESIAN_POINT('Ctrl Pts',(-0.00937815905213374,-0.155269567283624,
0.216378293833576));
#9563=CARTESIAN_POINT('Ctrl Pts',(-0.0102628952470384,-0.155213599000284,
0.216315752873355));
#9564=CARTESIAN_POINT('Ctrl Pts',(-0.0116678433714427,-0.155112657499286,
0.216216003096434));
#9565=CARTESIAN_POINT('Ctrl Pts',(-0.0121884006488223,-0.155072621577634,
0.216178948971282));
#9566=CARTESIAN_POINT('Ctrl Pts',(-0.0131683409589588,-0.154992289963757,
0.216109011449784));
#9567=CARTESIAN_POINT('Ctrl Pts',(-0.0136277667241898,-0.154952570541831,
0.216076146465476));
#9568=CARTESIAN_POINT('Ctrl Pts',(-0.0146612422527259,-0.15485859017616,
0.216002042014398));
#9569=CARTESIAN_POINT('Ctrl Pts',(-0.0152351778821357,-0.154803179276406,
0.21596076691561));
#9570=CARTESIAN_POINT('Ctrl Pts',(-0.0166993874260494,-0.154653594883159,
0.215855149643284));
#9571=CARTESIAN_POINT('Ctrl Pts',(-0.017589169990822,-0.154554925471253,
0.21579066735978));
#9572=CARTESIAN_POINT('Ctrl Pts',(-0.0228745183800269,-0.153922593036332,
0.215405803480896));
#9573=CARTESIAN_POINT('Ctrl Pts',(-0.0272460844993458,-0.153209176604658,
0.215079828086814));
#9574=CARTESIAN_POINT('Ctrl Pts',(-0.0422569970654817,-0.150096729167453,
0.213932546947964));
#9575=CARTESIAN_POINT('Ctrl Pts',(-0.0526695479242094,-0.146766949687107,
0.213084662781003));
#9576=CARTESIAN_POINT('Ctrl Pts',(-0.0693864159392888,-0.139411425143715,
0.211670861524967));
#9577=CARTESIAN_POINT('Ctrl Pts',(-0.0759079812786701,-0.135970686414469,
0.21110532117864));
#9578=CARTESIAN_POINT('Ctrl Pts',(-0.0828770836505378,-0.131635484747435,
0.21050200566044));
#9579=CARTESIAN_POINT('Ctrl Pts',(-0.0835886271819541,-0.131184806019123,
0.210440425484894));
#9580=CARTESIAN_POINT('Ctrl Pts',(-0.0845990160951622,-0.130533285207041,
0.210353046301048));
#9581=CARTESIAN_POINT('Ctrl Pts',(-0.0849008621752209,-0.130337161547275,
0.210326950719709));
#9582=CARTESIAN_POINT('Ctrl Pts',(-0.0854213789154936,-0.129996381725557,
0.21028196837972));
#9583=CARTESIAN_POINT('Ctrl Pts',(-0.0856403684051018,-0.129852218084454,
0.210263049211255));
#9584=CARTESIAN_POINT('Ctrl Pts',(-0.0860653638710163,-0.129570895226066,
0.210226344738713));
#9585=CARTESIAN_POINT('Ctrl Pts',(-0.0862714068031839,-0.129433798207739,
0.210208555346182));
#9586=CARTESIAN_POINT('Ctrl Pts',(-0.0868286530495609,-0.129061095457826,
0.210160455673437));
#9587=CARTESIAN_POINT('Ctrl Pts',(-0.0871792277184288,-0.128824545863323,
0.210130208182306));
#9588=CARTESIAN_POINT('Ctrl Pts',(-0.0884891728219151,-0.127932866602835,
0.210017217335792));
#9589=CARTESIAN_POINT('Ctrl Pts',(-0.0894421917464415,-0.127268403831028,
0.209935075911212));
#9590=CARTESIAN_POINT('Ctrl Pts',(-0.097507886421842,-0.121509491581732,
0.209239581405412));
#9591=CARTESIAN_POINT('Ctrl Pts',(-0.104187617431709,-0.115833208423761,
0.208661060256938));
#9592=CARTESIAN_POINT('Ctrl Pts',(-0.116882277964981,-0.103053911551563,
0.20747450593467));
#9593=CARTESIAN_POINT('Ctrl Pts',(-0.122808935963316,-0.095914150571156,
0.206868549556619));
#9594=CARTESIAN_POINT('Ctrl Pts',(-0.130514797297375,-0.0847367457109193,
0.205946608661568));
#9595=CARTESIAN_POINT('Ctrl Pts',(-0.132815269694958,-0.0810834549056396,
0.205649212796718));
#9596=CARTESIAN_POINT('Ctrl Pts',(-0.135427581208484,-0.0765248611403557,
0.205280209092682));
#9597=CARTESIAN_POINT('Ctrl Pts',(-0.135887031577635,-0.0757060017737411,
0.205214007796385));
#9598=CARTESIAN_POINT('Ctrl Pts',(-0.136595927150349,-0.0744153206732391,
0.205109766032161));
#9599=CARTESIAN_POINT('Ctrl Pts',(-0.136850411266116,-0.073946279070383,
0.205071905338756));
#9600=CARTESIAN_POINT('Ctrl Pts',(-0.137297911801987,-0.0731112652080053,
0.205004536943811));
#9601=CARTESIAN_POINT('Ctrl Pts',(-0.13749189210496,-0.072745812833661,
0.204975063728403));
#9602=CARTESIAN_POINT('Ctrl Pts',(-0.137936215592312,-0.0719005964696098,
0.204906921571));
#9603=CARTESIAN_POINT('Ctrl Pts',(-0.138185516512878,-0.0714202937337249,
0.204868216359888));
#9604=CARTESIAN_POINT('Ctrl Pts',(-0.138864267843637,-0.0700957543385004,
0.204761519373261));
#9605=CARTESIAN_POINT('Ctrl Pts',(-0.139288514952702,-0.0692488930493088,
0.2046933467738));
#9606=CARTESIAN_POINT('Ctrl Pts',(-0.140757040059304,-0.0662493958690764,
0.204452009153767));
#9607=CARTESIAN_POINT('Ctrl Pts',(-0.141759312481047,-0.0640766956419882,
0.204277409810209));
#9608=CARTESIAN_POINT('Ctrl Pts',(-0.14928409784167,-0.0467231450698623,
0.202883733406977));
#9609=CARTESIAN_POINT('Ctrl Pts',(-0.153399030139654,-0.0306151836416825,
0.201578915861666));
#9610=CARTESIAN_POINT('Ctrl Pts',(-0.155162654095302,-0.011333878156473,
0.200102186883096));
#9611=CARTESIAN_POINT('Ctrl Pts',(-0.155344101418235,-0.00849225672462064,
0.199887123865749));
#9612=CARTESIAN_POINT('Ctrl Pts',(-0.155486965269954,-0.00455962930237522,
0.199594346526066));
#9613=CARTESIAN_POINT('Ctrl Pts',(-0.155515059080838,-0.00347176520191675,
0.199513870672425));
#9614=CARTESIAN_POINT('Ctrl Pts',(-0.155543910366021,-0.00158924274323212,
0.199375595710535));
#9615=CARTESIAN_POINT('Ctrl Pts',(-0.155549999139583,-0.000794722658689682,
0.199317540579627));
#9616=CARTESIAN_POINT('Ctrl Pts',(-0.155550000342681,0.000316399235418375,
0.199236808123642));
#9617=CARTESIAN_POINT('Ctrl Pts',(-0.155549034291159,0.000632969976002597,
0.199213858398416));
#9618=CARTESIAN_POINT('Ctrl Pts',(-0.155545500768554,0.00121180770477676,
0.199171993106568));
#9619=CARTESIAN_POINT('Ctrl Pts',(-0.155543236412517,0.00147407517694016,
0.199153060811953));
#9620=CARTESIAN_POINT('Ctrl Pts',(-0.155537225019332,0.00201257227774423,
0.199114265051489));
#9621=CARTESIAN_POINT('Ctrl Pts',(-0.155533405467419,0.0022887989999451,
0.199094405706065));
#9622=CARTESIAN_POINT('Ctrl Pts',(-0.155521771441978,0.00299422378799091,
0.1990437911553));
#9623=CARTESIAN_POINT('Ctrl Pts',(-0.155512916086898,0.00342340627076611,
0.199013093580586));
#9624=CARTESIAN_POINT('Ctrl Pts',(-0.155469633330967,0.00517044689907013,
0.198888507771571));
#9625=CARTESIAN_POINT('Ctrl Pts',(-0.155420228645702,0.00648793083959554,
0.198795417662487));
#9626=CARTESIAN_POINT('Ctrl Pts',(-0.154901820251506,0.016806970299302,
0.198071936466645));
#9627=CARTESIAN_POINT('Ctrl Pts',(-0.153667860153803,0.0257543453427825,
0.19747768483264));
#9628=CARTESIAN_POINT('Ctrl Pts',(-0.149025949330323,0.0461337386908556,
0.196101592696785));
#9629=CARTESIAN_POINT('Ctrl Pts',(-0.145067540140679,0.0573795779779629,
0.195322362706915));
#9630=CARTESIAN_POINT('Ctrl Pts',(-0.139108203529722,0.0696256006050569,
0.194375803831849));
#9631=CARTESIAN_POINT('Ctrl Pts',(-0.138322478190227,0.0711737883865281,
0.19425429999787));
#9632=CARTESIAN_POINT('Ctrl Pts',(-0.137182550484042,0.073329695147618,
0.194082342792856));
#9633=CARTESIAN_POINT('Ctrl Pts',(-0.136849867339884,0.0739486992961989,
0.194032646061073));
#9634=CARTESIAN_POINT('Ctrl Pts',(-0.136305052632136,0.0749461361058689,
0.19395203023885));
#9635=CARTESIAN_POINT('Ctrl Pts',(-0.136095509439666,0.0753259782123471,
0.193921203362643));
#9636=CARTESIAN_POINT('Ctrl Pts',(-0.135655618494086,0.0761155477302487,
0.193856856391696));
#9637=CARTESIAN_POINT('Ctrl Pts',(-0.13542499734438,0.0765251169266757,
0.193823326765658));
#9638=CARTESIAN_POINT('Ctrl Pts',(-0.134875730528528,0.0774903224899755,
0.193743947605972));
#9639=CARTESIAN_POINT('Ctrl Pts',(-0.134555504345432,0.0780450446397574,
0.193698041582094));
#9640=CARTESIAN_POINT('Ctrl Pts',(-0.133483075168693,0.0798765746846046,
0.193545512743486));
#9641=CARTESIAN_POINT('Ctrl Pts',(-0.132716073458506,0.0811445753146967,
0.193438355998556));
#9642=CARTESIAN_POINT('Ctrl Pts',(-0.128566572611405,0.0877882525102592,
0.192868419126585));
#9643=CARTESIAN_POINT('Ctrl Pts',(-0.124875769773437,0.0929632321347478,
0.192394341750511));
#9644=CARTESIAN_POINT('Ctrl Pts',(-0.11529448917821,0.104793764352739,0.191235705825436));
#9645=CARTESIAN_POINT('Ctrl Pts',(-0.109129819953951,0.111198982606901,
0.190543835551954));
#9646=CARTESIAN_POINT('Ctrl Pts',(-0.0972553415262483,0.121593274999628,
0.189324169066063));
#9647=CARTESIAN_POINT('Ctrl Pts',(-0.0917591668694762,0.125792717316811,
0.188795656672878));
#9648=CARTESIAN_POINT('Ctrl Pts',(-0.0854152377620299,0.130002054799282,
0.188237493636357));
#9649=CARTESIAN_POINT('Ctrl Pts',(-0.0848265842732654,0.130386915543376,
0.188186170394339));
#9650=CARTESIAN_POINT('Ctrl Pts',(-0.0839541341241629,0.13094891271503,
0.188110815417013));
#9651=CARTESIAN_POINT('Ctrl Pts',(-0.0836723552062635,0.13112914000228,
0.188086586328329));
#9652=CARTESIAN_POINT('Ctrl Pts',(-0.0831717076586671,0.131447085974692,
0.18804373280791));
#9653=CARTESIAN_POINT('Ctrl Pts',(-0.0829530751686131,0.131585168959528,
0.18802508451289));
#9654=CARTESIAN_POINT('Ctrl Pts',(-0.0824843871801998,0.131879548541915,
0.187985248994558));
#9655=CARTESIAN_POINT('Ctrl Pts',(-0.0822342318788695,0.13203567913011,
0.187964072722744));
#9656=CARTESIAN_POINT('Ctrl Pts',(-0.081547611027205,0.13246151468995,0.187906177572484));
#9657=CARTESIAN_POINT('Ctrl Pts',(-0.0811102473070708,0.132729776387485,
0.187869552113901));
#9658=CARTESIAN_POINT('Ctrl Pts',(-0.0787891303430609,0.134137700643264,
0.187676465984875));
#9659=CARTESIAN_POINT('Ctrl Pts',(-0.0768825435241392,0.135239512115259,
0.187522329798283));
#9660=CARTESIAN_POINT('Ctrl Pts',(-0.0712721377913392,0.13832473211187,
0.187079641027565));
#9661=CARTESIAN_POINT('Ctrl Pts',(-0.0675141063018767,0.140197111154279,
0.186796543977972));
#9662=CARTESIAN_POINT('Ctrl Pts',(-0.063688595018437,0.141913936470586,
0.186516973639705));
#9663=CARTESIAN_POINT('',(-0.155549922407231,-0.000136919941883599,0.185534971438302));
#9664=CARTESIAN_POINT('Ctrl Pts',(-0.0636886258390813,0.141913922638794,
0.172648810545196));
#9665=CARTESIAN_POINT('Ctrl Pts',(-0.0639417182132668,0.141800338959176,
0.172668973661729));
#9666=CARTESIAN_POINT('Ctrl Pts',(-0.0641945069200826,0.141686078141358,
0.172689159868843));
#9667=CARTESIAN_POINT('Ctrl Pts',(-0.0664530499226049,0.140657928652624,
0.172869938830651));
#9668=CARTESIAN_POINT('Ctrl Pts',(-0.068439374571081,0.139702225593533,
0.173031938049245));
#9669=CARTESIAN_POINT('Ctrl Pts',(-0.0758515134502319,0.135939923572788,
0.173648113200886));
#9670=CARTESIAN_POINT('Ctrl Pts',(-0.0811301671444233,0.13285704690294,
0.174111221789556));
#9671=CARTESIAN_POINT('Ctrl Pts',(-0.0937175181050919,0.124475337870062,
0.175273711163105));
#9672=CARTESIAN_POINT('Ctrl Pts',(-0.100772789699689,0.118835700746529,
0.175979128346218));
#9673=CARTESIAN_POINT('Ctrl Pts',(-0.108069580434532,0.111883415748812,
0.1767505997933));
#9674=CARTESIAN_POINT('Ctrl Pts',(-0.108831817555137,0.111142109540443,
0.176831734698813));
#9675=CARTESIAN_POINT('Ctrl Pts',(-0.112215640062796,0.107783012044303,
0.177194182808041));
#9676=CARTESIAN_POINT('Ctrl Pts',(-0.114751068644906,0.105079614864521,
0.177471969523666));
#9677=CARTESIAN_POINT('Ctrl Pts',(-0.117562240940566,0.101858952975878,
0.177784917250049));
#9678=CARTESIAN_POINT('Ctrl Pts',(-0.117934367268449,0.101427865205498,
0.177826448339971));
#9679=CARTESIAN_POINT('Ctrl Pts',(-0.118523905850323,0.100737286171255,
0.177892398762503));
#9680=CARTESIAN_POINT('Ctrl Pts',(-0.118742848218726,0.100479117661241,
0.177916925959434));
#9681=CARTESIAN_POINT('Ctrl Pts',(-0.119128283924557,0.100021607277894,
0.177960162936685));
#9682=CARTESIAN_POINT('Ctrl Pts',(-0.119295122807983,0.0998225607353291,
0.177978897771885));
#9683=CARTESIAN_POINT('Ctrl Pts',(-0.119646643576512,0.0994010401302771,
0.178018411165874));
#9684=CARTESIAN_POINT('Ctrl Pts',(-0.11983120366099,0.0991784690897692,
0.178039180924485));
#9685=CARTESIAN_POINT('Ctrl Pts',(-0.120325243415529,0.0985792874081295,
0.1780948469974));
#9686=CARTESIAN_POINT('Ctrl Pts',(-0.12063357869763,0.098201730211959,0.178129661530982));
#9687=CARTESIAN_POINT('Ctrl Pts',(-0.122063964529137,0.0964333163224236,
0.178291543773438));
#9688=CARTESIAN_POINT('Ctrl Pts',(-0.123163828363868,0.0950245655411512,
0.178417107605077));
#9689=CARTESIAN_POINT('Ctrl Pts',(-0.128636549858209,0.0877601655425551,
0.17904937617282));
#9690=CARTESIAN_POINT('Ctrl Pts',(-0.132617635979318,0.0816198383153492,
0.179534711032005));
#9691=CARTESIAN_POINT('Ctrl Pts',(-0.139242256336471,0.06962914980104,0.18043828420425));
#9692=CARTESIAN_POINT('Ctrl Pts',(-0.141984421590115,0.0638517545748268,
0.180856422367196));
#9693=CARTESIAN_POINT('Ctrl Pts',(-0.147171965812737,0.0509224721587812,
0.181783073294908));
#9694=CARTESIAN_POINT('Ctrl Pts',(-0.149467234747206,0.0437287776299269,
0.182293263309149));
#9695=CARTESIAN_POINT('Ctrl Pts',(-0.151470288887039,0.0354061329755489,
0.182892819001806));
#9696=CARTESIAN_POINT('Ctrl Pts',(-0.151699172719634,0.0344122590999078,
0.182964551070705));
#9697=CARTESIAN_POINT('Ctrl Pts',(-0.152048761681122,0.0328229430008052,
0.183079506224629));
#9698=CARTESIAN_POINT('Ctrl Pts',(-0.152175783291413,0.0322289074697977,
0.183122527642506));
#9699=CARTESIAN_POINT('Ctrl Pts',(-0.15239413391884,0.0311776811385245,
0.183198763695134));
#9700=CARTESIAN_POINT('Ctrl Pts',(-0.152486893764593,0.03072079223285,0.183231932316995));
#9701=CARTESIAN_POINT('Ctrl Pts',(-0.152661409101821,0.0298409490938165,
0.183295875579051));
#9702=CARTESIAN_POINT('Ctrl Pts',(-0.152743464424159,0.0294180580697884,
0.183326640343285));
#9703=CARTESIAN_POINT('Ctrl Pts',(-0.152915246019541,0.0285126447769438,
0.183392576434651));
#9704=CARTESIAN_POINT('Ctrl Pts',(-0.153004447144712,0.0280300289172811,
0.183427764112988));
#9705=CARTESIAN_POINT('Ctrl Pts',(-0.15321345475542,0.0268684775677711,
0.183512556799489));
#9706=CARTESIAN_POINT('Ctrl Pts',(-0.153331033459057,0.026189157199468,
0.183562231826929));
#9707=CARTESIAN_POINT('Ctrl Pts',(-0.153844156489786,0.0231025828091486,
0.183788339211882));
#9708=CARTESIAN_POINT('Ctrl Pts',(-0.154187532123694,0.020687133824531,
0.183966401283114));
#9709=CARTESIAN_POINT('Ctrl Pts',(-0.155196166219536,0.01215661187438,0.184599556860343));
#9710=CARTESIAN_POINT('Ctrl Pts',(-0.155555358047335,0.00601193323586903,
0.185063661244219));
#9711=CARTESIAN_POINT('Ctrl Pts',(-0.155549939608074,-0.0001370690496796,
0.185534952791332));
#9712=CARTESIAN_POINT('Ctrl Pts',(-0.155549939737365,-0.000136922248412486,
0.18553494153972));
#9713=CARTESIAN_POINT('Ctrl Pts',(-0.155539040632619,-0.0125188039811671,
0.186483953207384));
#9714=CARTESIAN_POINT('Ctrl Pts',(-0.154049857623245,-0.0248552119677568,
0.187460691532931));
#9715=CARTESIAN_POINT('Ctrl Pts',(-0.150751720167338,-0.0383672971839581,
0.188503754085351));
#9716=CARTESIAN_POINT('Ctrl Pts',(-0.150368100501018,-0.0398442644059964,
0.188617331311801));
#9717=CARTESIAN_POINT('Ctrl Pts',(-0.149776773575888,-0.0419906071237111,
0.188781519094411));
#9718=CARTESIAN_POINT('Ctrl Pts',(-0.149586192350252,-0.0426645531431382,
0.188832948329596));
#9719=CARTESIAN_POINT('Ctrl Pts',(-0.149278893054669,-0.0437238685240643,
0.188913563499235));
#9720=CARTESIAN_POINT('Ctrl Pts',(-0.149165222518933,-0.0441101007792151,
0.188942909595204));
#9721=CARTESIAN_POINT('Ctrl Pts',(-0.148946938349915,-0.0448412978529119,
0.188998372175556));
#9722=CARTESIAN_POINT('Ctrl Pts',(-0.148842622927789,-0.0451863479829484,
0.189024504992108));
#9723=CARTESIAN_POINT('Ctrl Pts',(-0.148660359450103,-0.0457817515632065,
0.189069526069329));
#9724=CARTESIAN_POINT('Ctrl Pts',(-0.148582976562012,-0.0460322748563397,
0.189088446929479));
#9725=CARTESIAN_POINT('Ctrl Pts',(-0.148431400839802,-0.0465186291977152,
0.189125134358384));
#9726=CARTESIAN_POINT('Ctrl Pts',(-0.148357279329619,-0.0467544788223972,
0.189142905092716));
#9727=CARTESIAN_POINT('Ctrl Pts',(-0.148155160929256,-0.0473922856611791,
0.189190910152681));
#9728=CARTESIAN_POINT('Ctrl Pts',(-0.14802608940055,-0.0477939046130302,
0.189221082094392));
#9729=CARTESIAN_POINT('Ctrl Pts',(-0.147537417258178,-0.0492934866071408,
0.189333546493853));
#9730=CARTESIAN_POINT('Ctrl Pts',(-0.147167209420562,-0.0503879945550053,
0.18941524402898));
#9731=CARTESIAN_POINT('Ctrl Pts',(-0.143149849314013,-0.0618430598842776,
0.190267220108078));
#9732=CARTESIAN_POINT('Ctrl Pts',(-0.138426652492428,-0.0717954492526159,
0.190982359402924));
#9733=CARTESIAN_POINT('Ctrl Pts',(-0.130282029608854,-0.0851102105377999,
0.192010144725049));
#9734=CARTESIAN_POINT('Ctrl Pts',(-0.127696403078665,-0.088942571788872,
0.192315137291708));
#9735=CARTESIAN_POINT('Ctrl Pts',(-0.122354309116098,-0.0961463952623667,
0.19291508442459));
#9736=CARTESIAN_POINT('Ctrl Pts',(-0.119619403428955,-0.0995283860882286,
0.193209290599335));
#9737=CARTESIAN_POINT('Ctrl Pts',(-0.115004899189347,-0.104769377468851,
0.193690324877848));
#9738=CARTESIAN_POINT('Ctrl Pts',(-0.113213280178866,-0.106702863364689,
0.193873724654354));
#9739=CARTESIAN_POINT('Ctrl Pts',(-0.110826779967445,-0.109150541291889,
0.194114330936187));
#9740=CARTESIAN_POINT('Ctrl Pts',(-0.110275844173366,-0.10970712818174,
0.194169630695438));
#9741=CARTESIAN_POINT('Ctrl Pts',(-0.109412750689971,-0.110566004150522,
0.194255898309681));
#9742=CARTESIAN_POINT('Ctrl Pts',(-0.109103483664113,-0.110871191626771,
0.194286738370071));
#9743=CARTESIAN_POINT('Ctrl Pts',(-0.108497324292503,-0.11146436291253,
0.194347047854914));
#9744=CARTESIAN_POINT('Ctrl Pts',(-0.108200553692674,-0.111752466427655,
0.194376511702652));
#9745=CARTESIAN_POINT('Ctrl Pts',(-0.10751312742206,-0.112414511409432,
0.194444617820238));
#9746=CARTESIAN_POINT('Ctrl Pts',(-0.1071216656877,-0.112787604239748,0.194483296271171));
#9747=CARTESIAN_POINT('Ctrl Pts',(-0.106040065093725,-0.113807741608618,
0.194589882350488));
#9748=CARTESIAN_POINT('Ctrl Pts',(-0.105345966559504,-0.114450533905703,
0.194657970263093));
#9749=CARTESIAN_POINT('Ctrl Pts',(-0.101740745794513,-0.117728683008753,
0.195010087022277));
#9750=CARTESIAN_POINT('Ctrl Pts',(-0.0987367041809033,-0.120259221109373,
0.195298435400113));
#9751=CARTESIAN_POINT('Ctrl Pts',(-0.0949865095207073,-0.123183005964574,
0.195652880595562));
#9752=CARTESIAN_POINT('Ctrl Pts',(-0.0943285717427634,-0.123687551749149,
0.195714865043418));
#9753=CARTESIAN_POINT('Ctrl Pts',(-0.0849881302849278,-0.130732485279815,
0.196592016886436));
#9754=CARTESIAN_POINT('Ctrl Pts',(-0.0756482806278708,-0.136349707891492,
0.197438200822188));
#9755=CARTESIAN_POINT('Ctrl Pts',(-0.0611031768996177,-0.143140085480536,
0.198680184268759));
#9756=CARTESIAN_POINT('Ctrl Pts',(-0.0562982223114,-0.145097212887848,0.199078819580188));
#9757=CARTESIAN_POINT('Ctrl Pts',(-0.0491056384804594,-0.147615614205386,
0.199651193415899));
#9758=CARTESIAN_POINT('Ctrl Pts',(-0.046788377874307,-0.148366380235098,
0.199831988181158));
#9759=CARTESIAN_POINT('Ctrl Pts',(-0.0439445929522421,-0.149214470235712,
0.20004873305551));
#9760=CARTESIAN_POINT('Ctrl Pts',(-0.0434341267887402,-0.149363857843226,
0.200087439793114));
#9761=CARTESIAN_POINT('Ctrl Pts',(-0.0426355489305593,-0.149593120965101,
0.200147671155916));
#9762=CARTESIAN_POINT('Ctrl Pts',(-0.0423479628520096,-0.149674787185721,
0.200169296854877));
#9763=CARTESIAN_POINT('Ctrl Pts',(-0.0418118470724394,-0.149825359858296,
0.20020948808987));
#9764=CARTESIAN_POINT('Ctrl Pts',(-0.041563384092665,-0.149894476605321,
0.200228065262291));
#9765=CARTESIAN_POINT('Ctrl Pts',(-0.0409984699345812,-0.150050110245684,
0.20027019176312));
#9766=CARTESIAN_POINT('Ctrl Pts',(-0.0406819167577055,-0.150136244045255,
0.200293718732734));
#9767=CARTESIAN_POINT('Ctrl Pts',(-0.0397171973602681,-0.150395468036203,
0.20036518570801));
#9768=CARTESIAN_POINT('Ctrl Pts',(-0.0390681700670027,-0.150565370198937,
0.200412946014653));
#9769=CARTESIAN_POINT('Ctrl Pts',(-0.0368219814581839,-0.151137874468279,
0.200577199289516));
#9770=CARTESIAN_POINT('Ctrl Pts',(-0.0352194708975504,-0.151519321703812,
0.200692575539621));
#9771=CARTESIAN_POINT('Ctrl Pts',(-0.0332048303776652,-0.151965176593364,
0.20083571951493));
#9772=CARTESIAN_POINT('Ctrl Pts',(-0.0327981751398694,-0.152053462219372,
0.200864516449855));
#9773=CARTESIAN_POINT('Ctrl Pts',(-0.020153787612586,-0.15474549680438,
0.201757056412309));
#9774=CARTESIAN_POINT('Ctrl Pts',(-0.00764527844441893,-0.155865249716474,
0.202559841615445));
#9775=CARTESIAN_POINT('Ctrl Pts',(0.0122924810377385,-0.155241555213235,
0.203883259336207));
#9776=CARTESIAN_POINT('Ctrl Pts',(0.0196942376803756,-0.154477052668175,
0.204383650834542));
#9777=CARTESIAN_POINT('Ctrl Pts',(0.0280927467869705,-0.152996090114723,
0.204977436648777));
#9778=CARTESIAN_POINT('Ctrl Pts',(0.0291710553323685,-0.152794160348969,
0.205054160035188));
#9779=CARTESIAN_POINT('Ctrl Pts',(0.0311270520522133,-0.152406410130376,
0.205194268801548));
#9780=CARTESIAN_POINT('Ctrl Pts',(0.0320054474960424,-0.152224368905421,
0.205257533736885));
#9781=CARTESIAN_POINT('Ctrl Pts',(0.0333933507292141,-0.151924192019136,
0.205358064116007));
#9782=CARTESIAN_POINT('Ctrl Pts',(0.033903931901778,-0.151811064758285,
0.205395169551933));
#9783=CARTESIAN_POINT('Ctrl Pts',(0.0348172919223506,-0.15160385799833,
0.205461769859831));
#9784=CARTESIAN_POINT('Ctrl Pts',(0.0352202863708006,-0.151510742189058,
0.205491233613483));
#9785=CARTESIAN_POINT('Ctrl Pts',(0.0361493430622541,-0.15129216759957,
0.205559342127009));
#9786=CARTESIAN_POINT('Ctrl Pts',(0.036675129299857,-0.151165571007426,
0.205598023079656));
#9787=CARTESIAN_POINT('Ctrl Pts',(0.0381189568383495,-0.150809956155432,
0.205704622763903));
#9788=CARTESIAN_POINT('Ctrl Pts',(0.0390355720223534,-0.150575302720666,
0.205772721856004));
#9789=CARTESIAN_POINT('Ctrl Pts',(0.0437469016346806,-0.149323293186211,
0.206124989748362));
#9790=CARTESIAN_POINT('Ctrl Pts',(0.0475038953559363,-0.148170888050607,
0.206413482501409));
#9791=CARTESIAN_POINT('Ctrl Pts',(0.05308832834334,-0.146223720771394,0.206854316864829));
#9792=CARTESIAN_POINT('Ctrl Pts',(0.0549509344600306,-0.145533986854355,
0.207003406573533));
#9793=CARTESIAN_POINT('Ctrl Pts',(0.0704348690671795,-0.139460573714846,
0.208259923048057));
#9794=CARTESIAN_POINT('Ctrl Pts',(0.0832441977050638,-0.132214401296347,
0.209421037031592));
#9795=CARTESIAN_POINT('Ctrl Pts',(0.0969721060850179,-0.121652696283706,
0.210725124399454));
#9796=CARTESIAN_POINT('Ctrl Pts',(0.0990513773965682,-0.119965807017144,
0.210924210972425));
#9797=CARTESIAN_POINT('Ctrl Pts',(0.101499867628294,-0.117872284904401,
0.211159572001594));
#9798=CARTESIAN_POINT('Ctrl Pts',(0.101911653301926,-0.117516439795512,
0.211199187026749));
#9799=CARTESIAN_POINT('Ctrl Pts',(0.102548770129102,-0.116960007000574,
0.211260518436819));
#9800=CARTESIAN_POINT('Ctrl Pts',(0.102775394138162,-0.116760917504689,
0.21128234188055));
#9801=CARTESIAN_POINT('Ctrl Pts',(0.103194486828238,-0.116390578467316,
0.211322711688262));
#9802=CARTESIAN_POINT('Ctrl Pts',(0.103387107416474,-0.116219511656509,
0.211341270659615));
#9803=CARTESIAN_POINT('Ctrl Pts',(0.103821302796505,-0.115831967959875,
0.211383116384302));
#9804=CARTESIAN_POINT('Ctrl Pts',(0.104062625483538,-0.115615213957759,
0.211406381996453));
#9805=CARTESIAN_POINT('Ctrl Pts',(0.104771887443112,-0.114974141041409,
0.211474791185273));
#9806=CARTESIAN_POINT('Ctrl Pts',(0.105237929833943,-0.114547717861974,
0.211519780446197));
#9807=CARTESIAN_POINT('Ctrl Pts',(0.108552007508273,-0.111478078079297,
0.211840097204828));
#9808=CARTESIAN_POINT('Ctrl Pts',(0.111303018961708,-0.108731525560737,
0.212108092150111));
#9809=CARTESIAN_POINT('Ctrl Pts',(0.114742620665422,-0.105029968757704,
0.212450751858512));
#9810=CARTESIAN_POINT('Ctrl Pts',(0.115527081287693,-0.104166486649202,
0.212529447045909));
#9811=CARTESIAN_POINT('Ctrl Pts',(0.126194902614687,-0.0921552993154266,
0.213608545809946));
#9812=CARTESIAN_POINT('Ctrl Pts',(0.134436370571208,-0.079653286324288,
0.214557409736697));
#9813=CARTESIAN_POINT('Ctrl Pts',(0.142178070761036,-0.0631829780156148,
0.215803638933402));
#9814=CARTESIAN_POINT('Ctrl Pts',(0.143486370149046,-0.0601527335660158,
0.21603236352221));
#9815=CARTESIAN_POINT('Ctrl Pts',(0.145014113161251,-0.0562801478210873,
0.216325085975819));
#9816=CARTESIAN_POINT('Ctrl Pts',(0.14532428254892,-0.0554743265172514,
0.21638601734551));
#9817=CARTESIAN_POINT('Ctrl Pts',(0.145809375075496,-0.0541820617366619,
0.216483782936316));
#9818=CARTESIAN_POINT('Ctrl Pts',(0.145988613521935,-0.0536972474540742,
0.216520472952763));
#9819=CARTESIAN_POINT('Ctrl Pts',(0.146323398127622,-0.0527776363513783,
0.216590094185665));
#9820=CARTESIAN_POINT('Ctrl Pts',(0.146479431362818,-0.0523430216708083,
0.216623008796056));
#9821=CARTESIAN_POINT('Ctrl Pts',(0.146828557048109,-0.0513567805645438,
0.216697728280902));
#9822=CARTESIAN_POINT('Ctrl Pts',(0.147020479484016,-0.0508047504651751,
0.216739571343013));
#9823=CARTESIAN_POINT('Ctrl Pts',(0.147578621128321,-0.0491697072885763,
0.216863573141082));
#9824=CARTESIAN_POINT('Ctrl Pts',(0.147936009512592,-0.0480837445370402,
0.216946020730349));
#9825=CARTESIAN_POINT('Ctrl Pts',(0.15136369309761,-0.0372682781845446,
0.217768186914167));
#9826=CARTESIAN_POINT('Ctrl Pts',(0.153481040981572,-0.0272650307074598,
0.218539484931237));
#9827=CARTESIAN_POINT('Ctrl Pts',(0.155159659068066,-0.0121136537890807,
0.219716330160525));
#9828=CARTESIAN_POINT('Ctrl Pts',(0.155470921744708,-0.00707472707619059,
0.220108622139947));
#9829=CARTESIAN_POINT('Ctrl Pts',(0.155630367645457,0.0051437616091677,
0.221054161423279));
#9830=CARTESIAN_POINT('Ctrl Pts',(0.155227609625231,0.0123161003060405,
0.221604600471537));
#9831=CARTESIAN_POINT('Ctrl Pts',(0.154225810689665,0.0202709210587499,
0.222193957570673));
#9832=CARTESIAN_POINT('Ctrl Pts',(0.154113864242088,0.0211051618566121,
0.222255497506975));
#9833=CARTESIAN_POINT('Ctrl Pts',(0.153944403243728,0.0222946779221939,
0.222342824933219));
#9834=CARTESIAN_POINT('Ctrl Pts',(0.153892421774163,0.0226507059775128,
0.22236890859857));
#9835=CARTESIAN_POINT('Ctrl Pts',(0.153800441095285,0.0232657582659785,
0.222413872321446));
#9836=CARTESIAN_POINT('Ctrl Pts',(0.153761021927958,0.0235248661827032,
0.222432784752465));
#9837=CARTESIAN_POINT('Ctrl Pts',(0.153683117329499,0.024028382410436,0.222469477474416));
#9838=CARTESIAN_POINT('Ctrl Pts',(0.153644703714674,0.0242727982760551,
0.222487261845966));
#9839=CARTESIAN_POINT('Ctrl Pts',(0.153539063058975,0.0249346625191474,
0.222535350488864));
#9840=CARTESIAN_POINT('Ctrl Pts',(0.153470716147304,0.0253519343738573,
0.222565591990565));
#9841=CARTESIAN_POINT('Ctrl Pts',(0.153208222685584,0.0269145399586885,
0.222678573819157));
#9842=CARTESIAN_POINT('Ctrl Pts',(0.153002942919686,0.0280580047711293,
0.222760712225859));
#9843=CARTESIAN_POINT('Ctrl Pts',(0.151149541019614,0.0377559641137137,
0.223453601070469));
#9844=CARTESIAN_POINT('Ctrl Pts',(0.148797985581871,0.0461617040687934,
0.22402981835978));
#9845=CARTESIAN_POINT('Ctrl Pts',(0.142509464031649,0.063033131529343,0.225215937878361));
#9846=CARTESIAN_POINT('Ctrl Pts',(0.138491357502649,0.0714300384728149,
0.225823718626687));
#9847=CARTESIAN_POINT('Ctrl Pts',(0.1315410438247,0.0831351019374812,0.22674810901456));
#9848=CARTESIAN_POINT('Ctrl Pts',(0.129180047215683,0.0867582900619423,
0.22704599610356));
#9849=CARTESIAN_POINT('Ctrl Pts',(0.126126322670216,0.0910430411351392,
0.22741552848657));
#9850=CARTESIAN_POINT('Ctrl Pts',(0.125574320258971,0.0918029118922866,
0.227481747791953));
#9851=CARTESIAN_POINT('Ctrl Pts',(0.12469797974035,0.0929865638714944,0.227586004124916));
#9852=CARTESIAN_POINT('Ctrl Pts',(0.124378277615167,0.0934137637424796,
0.22762386121688));
#9853=CARTESIAN_POINT('Ctrl Pts',(0.123806864785654,0.0941691765304058,
0.227691216556504));
#9854=CARTESIAN_POINT('Ctrl Pts',(0.123556029690901,0.0944980481143688,
0.22772068030149));
#9855=CARTESIAN_POINT('Ctrl Pts',(0.122974180111206,0.095254637886217,0.227788790944785));
#9856=CARTESIAN_POINT('Ctrl Pts',(0.12264224224166,0.095681635736158,0.227827474045571));
#9857=CARTESIAN_POINT('Ctrl Pts',(0.121723412751251,0.0968509616772653,
0.227934085173705));
#9858=CARTESIAN_POINT('Ctrl Pts',(0.121131971932128,0.0975896679567658,
0.228002193624759));
#9859=CARTESIAN_POINT('Ctrl Pts',(0.118049496013169,0.101368468161948,0.228354586947536));
#9860=CARTESIAN_POINT('Ctrl Pts',(0.115450844851062,0.104318488833734,0.228643199428682));
#9861=CARTESIAN_POINT('Ctrl Pts',(0.111376150293414,0.108605223431768,0.229084051436817));
#9862=CARTESIAN_POINT('Ctrl Pts',(0.109981454016877,0.110017364946379,0.229233034262993));
#9863=CARTESIAN_POINT('Ctrl Pts',(0.098069786755476,0.121625129633186,0.23048952974803));
#9864=CARTESIAN_POINT('Ctrl Pts',(0.0861898460025061,0.130313420816375,
0.231650738469756));
#9865=CARTESIAN_POINT('Ctrl Pts',(0.0709113945192309,0.138472143661504,
0.232954787576607));
#9866=CARTESIAN_POINT('Ctrl Pts',(0.0685190535638948,0.139671407539156,
0.233153768794131));
#9867=CARTESIAN_POINT('Ctrl Pts',(0.0656042043121951,0.141039664511051,
0.233389021999629));
#9868=CARTESIAN_POINT('Ctrl Pts',(0.0651104125233813,0.141268300738876,
0.233428631059508));
#9869=CARTESIAN_POINT('Ctrl Pts',(0.0643410447789384,0.141619643548459,
0.233489955264347));
#9870=CARTESIAN_POINT('Ctrl Pts',(0.0640663012192808,0.141744144621015,
0.233511777428152));
#9871=CARTESIAN_POINT('Ctrl Pts',(0.0635562333071361,0.141973497795979,
0.233552146077209));
#9872=CARTESIAN_POINT('Ctrl Pts',(0.0633210128548923,0.142078563483618,
0.23357070516352));
#9873=CARTESIAN_POINT('Ctrl Pts',(0.0627890094543122,0.142314609309305,
0.233612552681419));
#9874=CARTESIAN_POINT('Ctrl Pts',(0.0624920777659436,0.142445245455279,
0.233635819964093));
#9875=CARTESIAN_POINT('Ctrl Pts',(0.0616156562571677,0.142827562285832,
0.233704238579944));
#9876=CARTESIAN_POINT('Ctrl Pts',(0.0610350297570965,0.143076646674438,
0.233749235534027));
#9877=CARTESIAN_POINT('Ctrl Pts',(0.0568701835940164,0.14483336680916,0.234069757140718));
#9878=CARTESIAN_POINT('Ctrl Pts',(0.0532316838368128,0.146209836283875,
0.234337938566508));
#9879=CARTESIAN_POINT('Ctrl Pts',(0.0378214697027433,0.151387909529295,
0.235440350439778));
#9880=CARTESIAN_POINT('Ctrl Pts',(0.0256693213776257,0.153915221001169,
0.236233154463579));
#9881=CARTESIAN_POINT('Ctrl Pts',(0.00893888478883866,0.155355912811346,
0.237355792582719));
#9882=CARTESIAN_POINT('Ctrl Pts',(0.00451858627127134,0.15554722916914,
0.237654887105966));
#9883=CARTESIAN_POINT('Ctrl Pts',(-0.00258099136772841,0.155551629629462,
0.238143804550222));
#9884=CARTESIAN_POINT('Ctrl Pts',(-0.00525784153340671,0.155484161887903,
0.238330076431399));
#9885=CARTESIAN_POINT('Ctrl Pts',(-0.00873399088828066,0.155306682406141,
0.23857505944318));
#9886=CARTESIAN_POINT('Ctrl Pts',(-0.00953615489689704,0.155259492151519,
0.238631805749427));
#9887=CARTESIAN_POINT('Ctrl Pts',(-0.0108404041280703,0.155172619250435,
0.238724433414779));
#9888=CARTESIAN_POINT('Ctrl Pts',(-0.0113427333478066,0.155136709118216,
0.238760196489967));
#9889=CARTESIAN_POINT('Ctrl Pts',(-0.0123085667496582,0.155062948345425,
0.238829131359007));
#9890=CARTESIAN_POINT('Ctrl Pts',(-0.0127720936900695,0.155025457197018,
0.238862291535787));
#9891=CARTESIAN_POINT('Ctrl Pts',(-0.0138331900592842,0.154934841990167,
0.238938380281671));
#9892=CARTESIAN_POINT('Ctrl Pts',(-0.0144306309811333,0.15488033858614,
0.238981351633487));
#9893=CARTESIAN_POINT('Ctrl Pts',(-0.0160171942645502,0.154726339850241,
0.239095820528831));
#9894=CARTESIAN_POINT('Ctrl Pts',(-0.0170056891878823,0.154620817503584,
0.239167505849375));
#9895=CARTESIAN_POINT('Ctrl Pts',(-0.0244280280647339,0.153756443872188,
0.239708614235448));
#9896=CARTESIAN_POINT('Ctrl Pts',(-0.0308089082765891,0.152605902959035,
0.240190287540344));
#9897=CARTESIAN_POINT('Ctrl Pts',(-0.0462225854363646,0.148820497931415,
0.241395185496132));
#9898=CARTESIAN_POINT('Ctrl Pts',(-0.0551222709238866,0.145758361620418,
0.242127760292114));
#9899=CARTESIAN_POINT('Ctrl Pts',(-0.0636886300394901,0.141913920753719,
0.24285329779702));
#9900=CARTESIAN_POINT('Origin',(0.,0.,-0.129405622560373));
#9901=CARTESIAN_POINT('',(-0.0636886254453755,0.141913922815482,0.326750756222096));
#9902=CARTESIAN_POINT('',(-0.0636886270244494,0.14191392210682,0.31288131537517));
#9903=CARTESIAN_POINT('',(-0.0636886258329924,0.141913922641526,-0.129405622560373));
#9904=CARTESIAN_POINT('',(-0.155549941229055,0.000135217002094367,0.269470366437021));
#9905=CARTESIAN_POINT('Ctrl Pts',(-0.0636886254453755,0.141913922815482,
0.326750756222096));
#9906=CARTESIAN_POINT('Ctrl Pts',(-0.0582901109833659,0.144336686972171,
0.326320925124822));
#9907=CARTESIAN_POINT('Ctrl Pts',(-0.0527581233471341,0.146449271766227,
0.325880672208058));
#9908=CARTESIAN_POINT('Ctrl Pts',(-0.0357824592924485,0.151845092873984,
0.324529867261289));
#9909=CARTESIAN_POINT('Ctrl Pts',(-0.0240708969387131,0.154135863142175,
0.323594999854329));
#9910=CARTESIAN_POINT('Ctrl Pts',(-0.0106728027741258,0.155191115319544,
0.322567035016699));
#9911=CARTESIAN_POINT('Ctrl Pts',(-0.00913032694338526,0.155289498749078,
0.322449370544501));
#9912=CARTESIAN_POINT('Ctrl Pts',(-0.00444993155897336,0.155518046297418,
0.322094838601657));
#9913=CARTESIAN_POINT('Ctrl Pts',(-0.00130905213082067,0.155576201956878,
0.321860318200235));
#9914=CARTESIAN_POINT('Ctrl Pts',(0.00237521922574042,0.155532814160507,
0.321590762491016));
#9915=CARTESIAN_POINT('Ctrl Pts',(0.00291870551660551,0.155523564544498,
0.321551140620584));
#9916=CARTESIAN_POINT('Ctrl Pts',(0.00379656517409258,0.155504020805235,
0.321487382551291));
#9917=CARTESIAN_POINT('Ctrl Pts',(0.00413096688544281,0.155495496758018,
0.32146315171864));
#9918=CARTESIAN_POINT('Ctrl Pts',(0.00472382364613329,0.155478470720674,
0.32142029625768));
#9919=CARTESIAN_POINT('Ctrl Pts',(0.00498228712648372,0.155470402927405,
0.321401647758151));
#9920=CARTESIAN_POINT('Ctrl Pts',(0.00553542999574471,0.155451756047836,
0.321361813063243));
#9921=CARTESIAN_POINT('Ctrl Pts',(0.00583009908345493,0.155440983631135,
0.321340637813952));
#9922=CARTESIAN_POINT('Ctrl Pts',(0.00663734268955308,0.155409173964979,
0.321282748383538));
#9923=CARTESIAN_POINT('Ctrl Pts',(0.00714985289851023,0.155386438577707,
0.321246127591292));
#9924=CARTESIAN_POINT('Ctrl Pts',(0.00986033728558172,0.155252760312061,
0.321053109776168));
#9925=CARTESIAN_POINT('Ctrl Pts',(0.0120560285610156,0.155097709046656,
0.320899035283374));
#9926=CARTESIAN_POINT('Ctrl Pts',(0.0282010883755749,0.153612634846923,
0.319778034047897));
#9927=CARTESIAN_POINT('Ctrl Pts',(0.0419186180543963,0.150449599533689,
0.318886327432832));
#9928=CARTESIAN_POINT('Ctrl Pts',(0.0613993227837462,0.143081521775237,
0.31749584890497));
#9929=CARTESIAN_POINT('Ctrl Pts',(0.0676043431192616,0.140256307234454,
0.317033233784034));
#9930=CARTESIAN_POINT('Ctrl Pts',(0.0744869323724657,0.13655952731255,0.316485905688618));
#9931=CARTESIAN_POINT('Ctrl Pts',(0.0753655114682721,0.136076622503357,
0.316415379815532));
#9932=CARTESIAN_POINT('Ctrl Pts',(0.0767645123763301,0.135289966905287,
0.316301987193396));
#9933=CARTESIAN_POINT('Ctrl Pts',(0.077287954531985,0.134991620374683,0.31625931341458));
#9934=CARTESIAN_POINT('Ctrl Pts',(0.0782127668251281,0.134457362564195,
0.316183470913544));
#9935=CARTESIAN_POINT('Ctrl Pts',(0.0786148384531749,0.134222674718234,
0.316150346580373));
#9936=CARTESIAN_POINT('Ctrl Pts',(0.0794488544196931,0.133730829411704,
0.316081318580144));
#9937=CARTESIAN_POINT('Ctrl Pts',(0.079880617183301,0.133473376338569,0.316045404472165));
#9938=CARTESIAN_POINT('Ctrl Pts',(0.0809953201807312,0.132801351213353,
0.315952213834214));
#9939=CARTESIAN_POINT('Ctrl Pts',(0.081676320486284,0.132383607002119,0.315894821977248));
#9940=CARTESIAN_POINT('Ctrl Pts',(0.0845877515648008,0.130566639701334,
0.315647448158808));
#9941=CARTESIAN_POINT('Ctrl Pts',(0.0867855525243568,0.129116232193679,
0.315455590180177));
#9942=CARTESIAN_POINT('Ctrl Pts',(0.0924897279614938,0.125140394179507,
0.314943519388029));
#9943=CARTESIAN_POINT('Ctrl Pts',(0.0959292991634937,0.122523594916081,
0.314620039179894));
#9944=CARTESIAN_POINT('Ctrl Pts',(0.108808669876982,0.111850018503915,0.313350719745203));
#9945=CARTESIAN_POINT('Ctrl Pts',(0.117379397400703,0.102819188601871,0.312373701995559));
#9946=CARTESIAN_POINT('Ctrl Pts',(0.125275761156514,0.0922087801849701,
0.311366054176543));
#9947=CARTESIAN_POINT('Ctrl Pts',(0.125760324472868,0.0915467984804432,
0.311303730131871));
#9948=CARTESIAN_POINT('Ctrl Pts',(0.128130719767829,0.0882541649237341,
0.310996514011709));
#9949=CARTESIAN_POINT('Ctrl Pts',(0.129939535236669,0.0855686863609178,
0.310754628481084));
#9950=CARTESIAN_POINT('Ctrl Pts',(0.131955386486013,0.0823643077774252,
0.310477636656397));
#9951=CARTESIAN_POINT('Ctrl Pts',(0.132244940280963,0.0818985898076804,
0.310437659282426));
#9952=CARTESIAN_POINT('Ctrl Pts',(0.132706027828015,0.0811481555372005,
0.310373702093419));
#9953=CARTESIAN_POINT('Ctrl Pts',(0.132879118949211,0.080864409488134,0.310349624232085));
#9954=CARTESIAN_POINT('Ctrl Pts',(0.133185461264069,0.080358586834402,0.310306890920478));
#9955=CARTESIAN_POINT('Ctrl Pts',(0.133319068612005,0.0801367301469652,
0.310288212448523));
#9956=CARTESIAN_POINT('Ctrl Pts',(0.133602538456296,0.0796633537755949,
0.310248496338573));
#9957=CARTESIAN_POINT('Ctrl Pts',(0.133752244808418,0.0794117449078804,
0.310227468866258));
#9958=CARTESIAN_POINT('Ctrl Pts',(0.13415750845334,0.0787262281996331,0.310170398344127));
#9959=CARTESIAN_POINT('Ctrl Pts',(0.134411673587953,0.0782914944490271,
0.310134444316195));
#9960=CARTESIAN_POINT('Ctrl Pts',(0.135703212854175,0.076057568342193,0.309950867426656));
#9961=CARTESIAN_POINT('Ctrl Pts',(0.136706654583689,0.07423885378224,0.309805305807871));
#9962=CARTESIAN_POINT('Ctrl Pts',(0.139552947965225,0.0688264719914708,
0.309381805733331));
#9963=CARTESIAN_POINT('Ctrl Pts',(0.141292739763657,0.0651803320972412,
0.309108787817847));
#9964=CARTESIAN_POINT('Ctrl Pts',(0.147014222448333,0.0518806514822679,
0.30814171923541));
#9965=CARTESIAN_POINT('Ctrl Pts',(0.150163855150907,0.0419000137475358,
0.30746699786141));
#9966=CARTESIAN_POINT('Ctrl Pts',(0.153611925935303,0.0253240905266897,
0.306334681780179));
#9967=CARTESIAN_POINT('Ctrl Pts',(0.154534618203243,0.0188935870117826,
0.305893080609385));
#9968=CARTESIAN_POINT('Ctrl Pts',(0.155132422106355,0.0114334299925759,
0.305368703045123));
#9969=CARTESIAN_POINT('Ctrl Pts',(0.155202354672146,0.0104412993850196,
0.305298730441605));
#9970=CARTESIAN_POINT('Ctrl Pts',(0.155299222545004,0.00884952964703879,
0.305186058417093));
#9971=CARTESIAN_POINT('Ctrl Pts',(0.15533221059567,0.00825027461614965,
0.305143548053034));
#9972=CARTESIAN_POINT('Ctrl Pts',(0.155384610726287,0.00718621328626032,
0.305067893831824));
#9973=CARTESIAN_POINT('Ctrl Pts',(0.155405407285597,0.00672147972893468,
0.305034793618392));
#9974=CARTESIAN_POINT('Ctrl Pts',(0.155444381178197,0.00575331483119456,
0.304965713044568));
#9975=CARTESIAN_POINT('Ctrl Pts',(0.155462198202698,0.0052498752740376,
0.30492972182303));
#9976=CARTESIAN_POINT('Ctrl Pts',(0.15550209362601,0.0039430129819499,0.304836107462004));
#9977=CARTESIAN_POINT('Ctrl Pts',(0.15552039086842,0.00313949877787785,
0.304778367008649));
#9978=CARTESIAN_POINT('Ctrl Pts',(0.155572667994231,-0.000341307548242315,
0.30452741782614));
#9979=CARTESIAN_POINT('Ctrl Pts',(0.15554374271425,-0.00301893436405565,
0.3043322650992));
#9980=CARTESIAN_POINT('Ctrl Pts',(0.155283834256495,-0.0101139993587367,
0.303809163172111));
#9981=CARTESIAN_POINT('Ctrl Pts',(0.154933531392658,-0.0145243350513768,
0.303477768604749));
#9982=CARTESIAN_POINT('Ctrl Pts',(0.152891807675056,-0.0311915515881011,
0.302202409464882));
#9983=CARTESIAN_POINT('Ctrl Pts',(0.149928786109605,-0.0432450630509603,
0.301228198694679));
#9984=CARTESIAN_POINT('Ctrl Pts',(0.144199783413796,-0.0584580099248424,
0.299990749377524));
#9985=CARTESIAN_POINT('Ctrl Pts',(0.14269360377312,-0.0620440031988351,
0.299698877066495));
#9986=CARTESIAN_POINT('Ctrl Pts',(0.140788092596793,-0.0661431384855975,
0.299367909198624));
#9987=CARTESIAN_POINT('Ctrl Pts',(0.140518231836121,-0.0667145287338506,
0.299321837031124));
#9988=CARTESIAN_POINT('Ctrl Pts',(0.140104534957726,-0.0675768234715042,
0.29925242069617));
#9989=CARTESIAN_POINT('Ctrl Pts',(0.139963262698345,-0.0678689390390178,
0.299228924410958));
#9990=CARTESIAN_POINT('Ctrl Pts',(0.139708153052337,-0.068392257463147,
0.299186869298371));
#9991=CARTESIAN_POINT('Ctrl Pts',(0.139594654845669,-0.0686236202205007,
0.299168289979218));
#9992=CARTESIAN_POINT('Ctrl Pts',(0.139347008278992,-0.0691252836335875,
0.299128034175251));
#9993=CARTESIAN_POINT('Ctrl Pts',(0.139212648582225,-0.0693954755922074,
0.299106371128295));
#9994=CARTESIAN_POINT('Ctrl Pts',(0.138833678231784,-0.0701520397109793,
0.299045759318072));
#9995=CARTESIAN_POINT('Ctrl Pts',(0.138587295899455,-0.0706375277448612,
0.299006919120298));
#9996=CARTESIAN_POINT('Ctrl Pts',(0.137113893931152,-0.0735034316300548,
0.29877790310948));
#9997=CARTESIAN_POINT('Ctrl Pts',(0.135828019537181,-0.0758533177111465,
0.298591199690355));
#9998=CARTESIAN_POINT('Ctrl Pts',(0.127120598043966,-0.0908335695765035,
0.297400263076346));
#9999=CARTESIAN_POINT('Ctrl Pts',(0.118006561187256,-0.102395998037373,
0.29647133687095));
#10000=CARTESIAN_POINT('Ctrl Pts',(0.105952252301966,-0.113903356353573,
0.295351500190367));
#10001=CARTESIAN_POINT('Ctrl Pts',(0.104469455841599,-0.115264854424969,
0.295215438622432));
#10002=CARTESIAN_POINT('Ctrl Pts',(0.100038150820563,-0.119177902442594,
0.294812886440002));
#10003=CARTESIAN_POINT('Ctrl Pts',(0.097019839541405,-0.121647648552644,
0.294543759461496));
#10004=CARTESIAN_POINT('Ctrl Pts',(0.0931596446242968,-0.124571161105423,
0.29420375564164));
#10005=CARTESIAN_POINT('Ctrl Pts',(0.0924019799560585,-0.125134198346578,
0.294137215917408));
#10006=CARTESIAN_POINT('Ctrl Pts',(0.0912025773697343,-0.126008668068039,
0.29403216089233));
#10007=CARTESIAN_POINT('Ctrl Pts',(0.0907642513720203,-0.126324760861218,
0.293993825977405));
#10008=CARTESIAN_POINT('Ctrl Pts',(0.0899874343255327,-0.126878821568116,
0.293925984398484));
#10009=CARTESIAN_POINT('Ctrl Pts',(0.0896496222738355,-0.12711773644577,
0.293896514407064));
#10010=CARTESIAN_POINT('Ctrl Pts',(0.0888733773329952,-0.127662096257359,
0.293828867189764));
#10011=CARTESIAN_POINT('Ctrl Pts',(0.0884343178420111,-0.127966634065507,
0.293790655899963));
#10012=CARTESIAN_POINT('Ctrl Pts',(0.0872167660204803,-0.128801886361493,
0.293684827713051));
#10013=CARTESIAN_POINT('Ctrl Pts',(0.0864350188683064,-0.129327791468073,
0.293617030608923));
#10014=CARTESIAN_POINT('Ctrl Pts',(0.0846927362010747,-0.13047702489966,
0.293466241470117));
#10015=CARTESIAN_POINT('Ctrl Pts',(0.0837300063831723,-0.131096908784045,
0.293383125858262));
#10016=CARTESIAN_POINT('Ctrl Pts',(0.0807394573813568,-0.132976088845127,
0.293125528260265));
#10017=CARTESIAN_POINT('Ctrl Pts',(0.0786895134417772,-0.13419932752562,
0.292949766076832));
#10018=CARTESIAN_POINT('Ctrl Pts',(0.063552779746995,-0.14276561937207,
0.291657361230243));
#10019=CARTESIAN_POINT('Ctrl Pts',(0.0494933861140353,-0.148226928899269,
0.290474937900805));
#10020=CARTESIAN_POINT('Ctrl Pts',(0.0304589108108244,-0.152605992650428,
0.288981512458593));
#10021=CARTESIAN_POINT('Ctrl Pts',(0.0260002458625941,-0.153428586160075,
0.288639849816666));
#10022=CARTESIAN_POINT('Ctrl Pts',(0.0208543036868468,-0.154147140419328,
0.288259233628864));
#10023=CARTESIAN_POINT('Ctrl Pts',(0.0201964709833297,-0.154234709077025,
0.288210833279952));
#10024=CARTESIAN_POINT('Ctrl Pts',(0.0192139972853612,-0.154359099255711,
0.288138948437671));
#10025=CARTESIAN_POINT('Ctrl Pts',(0.0188897797816933,-0.154399110877777,
0.288115291432368));
#10026=CARTESIAN_POINT('Ctrl Pts',(0.01830941677064,-0.154468877932902,
0.288073063649479));
#10027=CARTESIAN_POINT('Ctrl Pts',(0.0180533222193519,-0.154499017966925,
0.288054471637995));
#10028=CARTESIAN_POINT('Ctrl Pts',(0.0174989975029473,-0.154562859895225,
0.288014319166698));
#10029=CARTESIAN_POINT('Ctrl Pts',(0.0172007451990448,-0.154596335471925,
0.287992771565049));
#10030=CARTESIAN_POINT('Ctrl Pts',(0.016368637830235,-0.154687292612542,
0.287932807138131));
#10031=CARTESIAN_POINT('Ctrl Pts',(0.0158345721877104,-0.154742874299795,
0.287894495176426));
#10032=CARTESIAN_POINT('Ctrl Pts',(0.012797494639218,-0.155043063221851,
0.287677562492922));
#10033=CARTESIAN_POINT('Ctrl Pts',(0.0102889443697388,-0.155229722983398,
0.287501992906389));
#10034=CARTESIAN_POINT('Ctrl Pts',(-0.00698094676142714,-0.156094218921507,
0.286311219262086));
#10035=CARTESIAN_POINT('Ctrl Pts',(-0.0217701013512237,-0.154726578431675,
0.285374843717495));
#10036=CARTESIAN_POINT('Ctrl Pts',(-0.0379214800930314,-0.150867815742666,
0.284259310255825));
#10037=CARTESIAN_POINT('Ctrl Pts',(-0.0396897590620582,-0.150412297191286,
0.28413599582269));
#10038=CARTESIAN_POINT('Ctrl Pts',(-0.0454076550927831,-0.148831486265594,
0.283732711240773));
#10039=CARTESIAN_POINT('Ctrl Pts',(-0.0493205268322766,-0.147580984552771,
0.283449587823713));
#10040=CARTESIAN_POINT('Ctrl Pts',(-0.0540009166304922,-0.145878265405383,
0.283099965806389));
#10041=CARTESIAN_POINT('Ctrl Pts',(-0.0548202064040207,-0.145572360799852,
0.28303835237914));
#10042=CARTESIAN_POINT('Ctrl Pts',(-0.0561693576057605,-0.145055613195911,
0.282936185745965));
#10043=CARTESIAN_POINT('Ctrl Pts',(-0.0567007247238053,-0.144848733006444,
0.282895764924838));
#10044=CARTESIAN_POINT('Ctrl Pts',(-0.0576592421891808,-0.144469465484676,
0.282822515128432));
#10045=CARTESIAN_POINT('Ctrl Pts',(-0.0580867892668555,-0.144298092750948,
0.282789720534529));
#10046=CARTESIAN_POINT('Ctrl Pts',(-0.0589150986463811,-0.143961805547251,
0.282725946621811));
#10047=CARTESIAN_POINT('Ctrl Pts',(-0.0593159457971507,-0.143797110096527,
0.282694974945782));
#10048=CARTESIAN_POINT('Ctrl Pts',(-0.0604009629802681,-0.143346002008202,
0.28261084038669));
#10049=CARTESIAN_POINT('Ctrl Pts',(-0.0610837736383424,-0.143056370649525,
0.282557568958235));
#10050=CARTESIAN_POINT('Ctrl Pts',(-0.0639388245435889,-0.141821161829619,
0.282333435379573));
#10051=CARTESIAN_POINT('Ctrl Pts',(-0.0660912798635748,-0.140830951154788,
0.282161063258689));
#10052=CARTESIAN_POINT('Ctrl Pts',(-0.0715947836888051,-0.13814517552773,
0.281711175681017));
#10053=CARTESIAN_POINT('Ctrl Pts',(-0.0749083747560809,-0.136376807863524,
0.281431275603599));
#10054=CARTESIAN_POINT('Ctrl Pts',(-0.0845601198995792,-0.13076802635846,
0.280588694625293));
#10055=CARTESIAN_POINT('Ctrl Pts',(-0.0906910240442798,-0.126593084772745,
0.280016480914248));
#10056=CARTESIAN_POINT('Ctrl Pts',(-0.103643547390748,-0.116347596842595,
0.278735801803397));
#10057=CARTESIAN_POINT('Ctrl Pts',(-0.110277293779692,-0.110080440989303,
0.278028330146676));
#10058=CARTESIAN_POINT('Ctrl Pts',(-0.117096675653929,-0.102398838755052,
0.2772689420312));
#10059=CARTESIAN_POINT('Ctrl Pts',(-0.117858631760769,-0.101520917864376,
0.277183601606336));
#10060=CARTESIAN_POINT('Ctrl Pts',(-0.118884376945866,-0.100311945242677,
0.277068133461041));
#10061=CARTESIAN_POINT('Ctrl Pts',(-0.119156736679291,-0.0999882670891371,
0.277037416609493));
#10062=CARTESIAN_POINT('Ctrl Pts',(-0.119586356768663,-0.0994734488844824,
0.276988878023448));
#10063=CARTESIAN_POINT('Ctrl Pts',(-0.119744484389673,-0.099283040942448,
0.276970994096709));
#10064=CARTESIAN_POINT('Ctrl Pts',(-0.12006917201687,-0.0988901671757694,
0.276934235513077));
#10065=CARTESIAN_POINT('Ctrl Pts',(-0.120235674636361,-0.0986876576821558,
0.276915365392171));
#10066=CARTESIAN_POINT('Ctrl Pts',(-0.120629525014883,-0.0982061592484336,
0.276870679546228));
#10067=CARTESIAN_POINT('Ctrl Pts',(-0.120856419930169,-0.0979267981114251,
0.276844896448671));
#10068=CARTESIAN_POINT('Ctrl Pts',(-0.121334544872652,-0.0973339207221548,
0.276790474052623));
#10069=CARTESIAN_POINT('Ctrl Pts',(-0.121585534597569,-0.0970202127838668,
0.276761851491534));
#10070=CARTESIAN_POINT('Ctrl Pts',(-0.123637434388573,-0.0944351088812501,
0.276527378092782));
#10071=CARTESIAN_POINT('Ctrl Pts',(-0.125375899765741,-0.0921145571175439,
0.276325680582519));
#10072=CARTESIAN_POINT('Ctrl Pts',(-0.133332039786485,-0.0808515455563323,
0.275380348264986));
#10073=CARTESIAN_POINT('Ctrl Pts',(-0.138664588988016,-0.0713203237475915,
0.274676414146517));
#10074=CARTESIAN_POINT('Ctrl Pts',(-0.144190224994525,-0.0584359147975346,
0.273749490832387));
#10075=CARTESIAN_POINT('Ctrl Pts',(-0.145335548306044,-0.0555261590693752,
0.273541809798545));
#10076=CARTESIAN_POINT('Ctrl Pts',(-0.147116060408715,-0.0505692593613106,
0.273188656103198));
#10077=CARTESIAN_POINT('Ctrl Pts',(-0.147798046706393,-0.0485399015835882,
0.273044255500863));
#10078=CARTESIAN_POINT('Ctrl Pts',(-0.14966751215074,-0.0425718069201622,
0.272619128352821));
#10079=CARTESIAN_POINT('Ctrl Pts',(-0.150740815246993,-0.0385995395850642,
0.27233554217521));
#10080=CARTESIAN_POINT('Ctrl Pts',(-0.151849957232022,-0.0337366061969515,
0.271985408570263));
#10081=CARTESIAN_POINT('Ctrl Pts',(-0.152037324006107,-0.032881912390198,
0.27192376349765));
#10082=CARTESIAN_POINT('Ctrl Pts',(-0.152334896757062,-0.0314675554134114,
0.271821555198225));
#10083=CARTESIAN_POINT('Ctrl Pts',(-0.152449254762276,-0.0309087774003956,
0.271781124546243));
#10084=CARTESIAN_POINT('Ctrl Pts',(-0.152650408622758,-0.0298976156953686,
0.271707864204032));
#10085=CARTESIAN_POINT('Ctrl Pts',(-0.152738273503795,-0.0294454491505347,
0.271675068940467));
#10086=CARTESIAN_POINT('Ctrl Pts',(-0.152904899511301,-0.0285671489025245,
0.271611295578362));
#10087=CARTESIAN_POINT('Ctrl Pts',(-0.15298389089345,-0.0281410627210089,
0.271580325129715));
#10088=CARTESIAN_POINT('Ctrl Pts',(-0.153153087502518,-0.0272066322474014,
0.271512331805116));
#10089=CARTESIAN_POINT('Ctrl Pts',(-0.15324254409131,-0.0266981594553495,
0.271475285530647));
#10090=CARTESIAN_POINT('Ctrl Pts',(-0.153456080376488,-0.0254479748661856,
0.271384078522261));
#10091=CARTESIAN_POINT('Ctrl Pts',(-0.153577314645084,-0.0247057972702772,
0.27132982849307));
#10092=CARTESIAN_POINT('Ctrl Pts',(-0.154066536286533,-0.0215680138064688,
0.271100008084215));
#10093=CARTESIAN_POINT('Ctrl Pts',(-0.154383869571322,-0.0191649788829334,
0.270922860778074));
#10094=CARTESIAN_POINT('Ctrl Pts',(-0.155252803672957,-0.0111452131060672,
0.270327540589336));
#10095=CARTESIAN_POINT('Ctrl Pts',(-0.155554845593828,-0.00550663010602916,
0.269902092796786));
#10096=CARTESIAN_POINT('Ctrl Pts',(-0.155549941229055,0.000135217002094367,
0.269470366437021));
#10097=CARTESIAN_POINT('Ctrl Pts',(-0.155549941365104,0.000135060403868008,
0.269470378420255));
#10098=CARTESIAN_POINT('Ctrl Pts',(-0.155538361405763,0.0134717745324127,
0.26844982442386));
#10099=CARTESIAN_POINT('Ctrl Pts',(-0.153811734320124,0.0267516801702719,
0.267394858539501));
#10100=CARTESIAN_POINT('Ctrl Pts',(-0.150111277084165,0.0407896868427397,
0.266312817712502));
#10101=CARTESIAN_POINT('Ctrl Pts',(-0.149797613421265,0.0419269517450572,
0.266225448687747));
#10102=CARTESIAN_POINT('Ctrl Pts',(-0.149236792556411,0.0438736619999813,
0.266076519031741));
#10103=CARTESIAN_POINT('Ctrl Pts',(-0.148995916974571,0.0446848439766073,
0.26601464858016));
#10104=CARTESIAN_POINT('Ctrl Pts',(-0.148642949659393,0.0458389144450729,
0.265926932409377));
#10105=CARTESIAN_POINT('Ctrl Pts',(-0.148536272114212,0.0461834216411417,
0.265900787037438));
#10106=CARTESIAN_POINT('Ctrl Pts',(-0.148349939715738,0.0467778439441754,
0.265855746577269));
#10107=CARTESIAN_POINT('Ctrl Pts',(-0.148270849562501,0.0470279328930674,
0.265836818850273));
#10108=CARTESIAN_POINT('Ctrl Pts',(-0.148115965218899,0.0475134138773714,
0.265800119717081));
#10109=CARTESIAN_POINT('Ctrl Pts',(-0.148040242376818,0.0477488250155281,
0.26578234413627));
#10110=CARTESIAN_POINT('Ctrl Pts',(-0.147833805744105,0.0483853943933405,
0.265734329048688));
#10111=CARTESIAN_POINT('Ctrl Pts',(-0.14770201935289,0.0487862070844197,
0.265704151940773));
#10112=CARTESIAN_POINT('Ctrl Pts',(-0.147203281391342,0.0502825137170163,
0.265591684826262));
#10113=CARTESIAN_POINT('Ctrl Pts',(-0.146825747271535,0.0513744818662478,
0.265509989668008));
#10114=CARTESIAN_POINT('Ctrl Pts',(-0.142730112011315,0.0628065013125632,
0.264657703250813));
#10115=CARTESIAN_POINT('Ctrl Pts',(-0.137937851128568,0.0727308189373068,
0.263942295714118));
#10116=CARTESIAN_POINT('Ctrl Pts',(-0.12975729239478,0.0859023757296986,
0.262921291152447));
#10117=CARTESIAN_POINT('Ctrl Pts',(-0.12721036291946,0.0896308770702425,
0.262623406814871));
#10118=CARTESIAN_POINT('Ctrl Pts',(-0.121858548842607,0.0967770005487323,
0.26202649707633));
#10119=CARTESIAN_POINT('Ctrl Pts',(-0.119063032751312,0.10019622165393,
0.261727916813682));
#10120=CARTESIAN_POINT('Ctrl Pts',(-0.114352767742845,0.105481519166797,
0.261240360201995));
#10121=CARTESIAN_POINT('Ctrl Pts',(-0.112528713944862,0.107425292334628,
0.261054932654558));
#10122=CARTESIAN_POINT('Ctrl Pts',(-0.110103093240845,0.109880524439778,
0.260812031158641));
#10123=CARTESIAN_POINT('Ctrl Pts',(-0.109546243220104,0.110435688742401,
0.260756510024244));
#10124=CARTESIAN_POINT('Ctrl Pts',(-0.108674959710832,0.111291260711172,
0.260669996614128));
#10125=CARTESIAN_POINT('Ctrl Pts',(-0.108363429192316,0.111594618084951,
0.260639133535982));
#10126=CARTESIAN_POINT('Ctrl Pts',(-0.107752979622864,0.112184085736192,
0.260578790309104));
#10127=CARTESIAN_POINT('Ctrl Pts',(-0.107454182589295,0.112470317631217,
0.260549315785306));
#10128=CARTESIAN_POINT('Ctrl Pts',(-0.106762901911694,0.113127259065976,
0.260481264210018));
#10129=CARTESIAN_POINT('Ctrl Pts',(-0.106369625196915,0.113497122387658,
0.260442651310369));
#10130=CARTESIAN_POINT('Ctrl Pts',(-0.105285153294287,0.114506443705127,
0.260336448360013));
#10131=CARTESIAN_POINT('Ctrl Pts',(-0.104590074552427,0.115141675282488,
0.260268680218121));
#10132=CARTESIAN_POINT('Ctrl Pts',(-0.101008839438464,0.118355376651227,
0.259920994573663));
#10133=CARTESIAN_POINT('Ctrl Pts',(-0.0980331892901918,0.12083157574309,
0.259636886249868));
#10134=CARTESIAN_POINT('Ctrl Pts',(-0.086678510720647,0.129584735278999,
0.25856874917064));
#10135=CARTESIAN_POINT('Ctrl Pts',(-0.0777657023239636,0.135121428718178,
0.257758592970445));
#10136=CARTESIAN_POINT('Ctrl Pts',(-0.0668190495798515,0.140477699583313,
0.256813759178683));
#10137=CARTESIAN_POINT('Ctrl Pts',(-0.0652596210018785,0.141208885972023,
0.256680339621468));
#10138=CARTESIAN_POINT('Ctrl Pts',(-0.0636886236493968,0.141913923621488,
0.256547255026181));
#10139=CARTESIAN_POINT('Ctrl Pts',(-0.0636886300394901,0.141913920753719,
0.24285329779702));
#10140=CARTESIAN_POINT('Ctrl Pts',(-0.0646310252844373,0.141490989290846,
0.242933115031557));
#10141=CARTESIAN_POINT('Ctrl Pts',(-0.0655693880425395,0.141058589799998,
0.243012827267554));
#10142=CARTESIAN_POINT('Ctrl Pts',(-0.0701705969310746,0.138882485006915,
0.243404678902055));
#10143=CARTESIAN_POINT('Ctrl Pts',(-0.0737686816808534,0.137005270628566,
0.243714243232908));
#10144=CARTESIAN_POINT('Ctrl Pts',(-0.0790971242092449,0.133954417778686,
0.244173589806775));
#10145=CARTESIAN_POINT('Ctrl Pts',(-0.0808838855652834,0.132883179207204,
0.244327773649405));
#10146=CARTESIAN_POINT('Ctrl Pts',(-0.0830756240255447,0.131508544011537,
0.244516604484947));
#10147=CARTESIAN_POINT('Ctrl Pts',(-0.0835012477505949,0.13123870655549,
0.244553260016158));
#10148=CARTESIAN_POINT('Ctrl Pts',(-0.084172084477396,0.130808823958321,
0.244611001763488));
#10149=CARTESIAN_POINT('Ctrl Pts',(-0.0844181647311111,0.130650150011145,
0.244632176075007));
#10150=CARTESIAN_POINT('Ctrl Pts',(-0.0848809667469775,0.13034987916913,
0.24467198340744));
#10151=CARTESIAN_POINT('Ctrl Pts',(-0.0850977803515731,0.13020843788296,
0.24469062580215));
#10152=CARTESIAN_POINT('Ctrl Pts',(-0.08559190055342,0.129884330543777,
0.244733098503388));
#10153=CARTESIAN_POINT('Ctrl Pts',(-0.085868975841331,0.129701317474722,
0.244756905315376));
#10154=CARTESIAN_POINT('Ctrl Pts',(-0.0866013419250812,0.129214201380808,
0.244819812346093));
#10155=CARTESIAN_POINT('Ctrl Pts',(-0.0870556223805546,0.128908575732652,
0.24485881330213));
#10156=CARTESIAN_POINT('Ctrl Pts',(-0.0901716165641117,0.12678824798451,
0.245126262904502));
#10157=CARTESIAN_POINT('Ctrl Pts',(-0.0927782537850686,0.124893473607168,
0.245349667757981));
#10158=CARTESIAN_POINT('Ctrl Pts',(-0.0959900452419526,0.122402709515645,
0.245627154765004));
#10159=CARTESIAN_POINT('Ctrl Pts',(-0.0966515095238083,0.121881080732186,
0.245684425565424));
#10160=CARTESIAN_POINT('Ctrl Pts',(-0.0980100135738502,0.120791753799071,
0.245802378344208));
#10161=CARTESIAN_POINT('Ctrl Pts',(-0.0987064355934165,0.120223334560066,
0.245863029049646));
#10162=CARTESIAN_POINT('Ctrl Pts',(-0.110933337841073,0.110065878648549,
0.246931902287378));
#10163=CARTESIAN_POINT('Ctrl Pts',(-0.121022191170155,0.0988654033982793,
0.247886286394423));
#10164=CARTESIAN_POINT('Ctrl Pts',(-0.131205465187675,0.0836185598499964,
0.249141409538127));
#10165=CARTESIAN_POINT('Ctrl Pts',(-0.132968919682436,0.0807849070926952,
0.249372643878607));
#10166=CARTESIAN_POINT('Ctrl Pts',(-0.135073785434927,0.077146782413369,
0.249668171050736));
#10167=CARTESIAN_POINT('Ctrl Pts',(-0.135501495390457,0.076393050999492,
0.249729324185004));
#10168=CARTESIAN_POINT('Ctrl Pts',(-0.136174555111127,0.075183515096626,
0.249827362145157));
#10169=CARTESIAN_POINT('Ctrl Pts',(-0.136423971337927,0.0747299835046003,
0.249864101335422));
#10170=CARTESIAN_POINT('Ctrl Pts',(-0.136891557240927,0.0738695957861169,
0.249933762654057));
#10171=CARTESIAN_POINT('Ctrl Pts',(-0.137110188769411,0.0734629958048693,
0.249966667923186));
#10172=CARTESIAN_POINT('Ctrl Pts',(-0.137600944887211,0.0725404899020796,
0.250041293699401));
#10173=CARTESIAN_POINT('Ctrl Pts',(-0.137871982856152,0.0720240170724891,
0.250083052018111));
#10174=CARTESIAN_POINT('Ctrl Pts',(-0.138663139207676,0.070495608776675,
0.250206573047868));
#10175=CARTESIAN_POINT('Ctrl Pts',(-0.139175056893584,0.0694794965617869,
0.250288621284287));
#10176=CARTESIAN_POINT('Ctrl Pts',(-0.144387811887925,0.0588438251891433,
0.251146868886069));
#10177=CARTESIAN_POINT('Ctrl Pts',(-0.148093635503412,0.0487710897163048,
0.251958081617822));
#10178=CARTESIAN_POINT('Ctrl Pts',(-0.152625356991953,0.0309821951729422,
0.253377140340226));
#10179=CARTESIAN_POINT('Ctrl Pts',(-0.153964934328477,0.0234350101372198,
0.253974383355005));
#10180=CARTESIAN_POINT('Ctrl Pts',(-0.15504708924477,0.0128497394444634,
0.254787005803065));
#10181=CARTESIAN_POINT('Ctrl Pts',(-0.155265173507138,0.00987137877698549,
0.25501284781695));
#10182=CARTESIAN_POINT('Ctrl Pts',(-0.1554471956716,0.00576508064528757,
0.255318874111009));
#10183=CARTESIAN_POINT('Ctrl Pts',(-0.155484809544134,0.00464122617924813,
0.25540207951625));
#10184=CARTESIAN_POINT('Ctrl Pts',(-0.155528663351504,0.0027021669107826,
0.255544581490408));
#10185=CARTESIAN_POINT('Ctrl Pts',(-0.155540687778674,0.00188715468499464,
0.255604154823418));
#10186=CARTESIAN_POINT('Ctrl Pts',(-0.155548753196391,0.000716937102396059,
0.25568919446813));
#10187=CARTESIAN_POINT('Ctrl Pts',(-0.155549984658848,0.000361799947529685,
0.25571493649624));
#10188=CARTESIAN_POINT('Ctrl Pts',(-0.155550011041026,-0.000254663437624176,
0.255759502982025));
#10189=CARTESIAN_POINT('Ctrl Pts',(-0.155549363710134,-0.000515986568123264,
0.25577835824537));
#10190=CARTESIAN_POINT('Ctrl Pts',(-0.155546638232264,-0.00106138237633014,
0.255817632196304));
#10191=CARTESIAN_POINT('Ctrl Pts',(-0.155544440473662,-0.00134545129377664,
0.255838044120524));
#10192=CARTESIAN_POINT('Ctrl Pts',(-0.155536595733541,-0.0020942519099721,
0.255891737721539));
#10193=CARTESIAN_POINT('Ctrl Pts',(-0.155529644058057,-0.00255897196269481,
0.255924947411003));
#10194=CARTESIAN_POINT('Ctrl Pts',(-0.155488728703524,-0.00466343375498688,
0.256074849985892));
#10195=CARTESIAN_POINT('Ctrl Pts',(-0.155430914162649,-0.00630268759477646,
0.256190279496122));
#10196=CARTESIAN_POINT('Ctrl Pts',(-0.155201019275601,-0.0108001549157698,
0.256504064543988));
#10197=CARTESIAN_POINT('Ctrl Pts',(-0.154975932195845,-0.0136551260960159,
0.256700027510645));
#10198=CARTESIAN_POINT('Ctrl Pts',(-0.15288775239119,-0.0332269647460581,
0.258031182991192));
#10199=CARTESIAN_POINT('Ctrl Pts',(-0.148402991951509,-0.0495511847403122,
0.259092852227158));
#10200=CARTESIAN_POINT('Ctrl Pts',(-0.140835635852098,-0.0660522538505316,
0.260346101737872));
#10201=CARTESIAN_POINT('Ctrl Pts',(-0.140264899314354,-0.0672557388049182,
0.260438531145712));
#10202=CARTESIAN_POINT('Ctrl Pts',(-0.139053280586148,-0.0697281011010006,
0.260630662994696));
#10203=CARTESIAN_POINT('Ctrl Pts',(-0.13841032142666,-0.0709958140481729,
0.260730427351576));
#10204=CARTESIAN_POINT('Ctrl Pts',(-0.13748681737535,-0.0727564347766701,
0.260870821827192));
#10205=CARTESIAN_POINT('Ctrl Pts',(-0.137220798580539,-0.0732569189562833,
0.260910941735121));
#10206=CARTESIAN_POINT('Ctrl Pts',(-0.13672873428624,-0.074170597539528,
0.260984576785553));
#10207=CARTESIAN_POINT('Ctrl Pts',(-0.136503535144281,-0.0745842423242739,
0.261018061667909));
#10208=CARTESIAN_POINT('Ctrl Pts',(-0.136043867976956,-0.0754195015726712,
0.261085981348318));
#10209=CARTESIAN_POINT('Ctrl Pts',(-0.135809310302092,-0.0758410604963707,
0.261120419062224));
#10210=CARTESIAN_POINT('Ctrl Pts',(-0.13522700051705,-0.0768762532084486,
0.261205380375507));
#10211=CARTESIAN_POINT('Ctrl Pts',(-0.134877031455413,-0.0774886206587898,
0.261255983084047));
#10212=CARTESIAN_POINT('Ctrl Pts',(-0.133574035952822,-0.0797329989666328,
0.261442733736896));
#10213=CARTESIAN_POINT('Ctrl Pts',(-0.132595489764074,-0.0813499214125757,
0.26157979973297));
#10214=CARTESIAN_POINT('Ctrl Pts',(-0.126189131654329,-0.0915128278749574,
0.262457941517948));
#10215=CARTESIAN_POINT('Ctrl Pts',(-0.119968364155803,-0.0995279482857881,
0.263228849318606));
#10216=CARTESIAN_POINT('Ctrl Pts',(-0.105583413615441,-0.11473844762226,
0.264848980466173));
#10217=CARTESIAN_POINT('Ctrl Pts',(-0.0973523903873451,-0.121800336528475,
0.2656954993498));
#10218=CARTESIAN_POINT('Ctrl Pts',(-0.0875174985688326,-0.128599330470599,
0.266579087403249));
#10219=CARTESIAN_POINT('Ctrl Pts',(-0.0865732676975356,-0.129236875070932,
0.266662706865862));
#10220=CARTESIAN_POINT('Ctrl Pts',(-0.0852719532568076,-0.130094859111347,
0.266776212351666));
#10221=CARTESIAN_POINT('Ctrl Pts',(-0.0849208879832633,-0.130324292342802,
0.266806662810959));
#10222=CARTESIAN_POINT('Ctrl Pts',(-0.0843618096442823,-0.130686450912175,
0.266854879919869));
#10223=CARTESIAN_POINT('Ctrl Pts',(-0.0841544048335969,-0.130820103684079,
0.266872707371933));
#10224=CARTESIAN_POINT('Ctrl Pts',(-0.0837256941361658,-0.13109492570158,
0.266909432174851));
#10225=CARTESIAN_POINT('Ctrl Pts',(-0.0835043488151082,-0.131236028336217,
0.266928324706472));
#10226=CARTESIAN_POINT('Ctrl Pts',(-0.0829767495209032,-0.131570485726683,
0.266973196221415));
#10227=CARTESIAN_POINT('Ctrl Pts',(-0.0826701727770193,-0.131763334109334,
0.266999141789122));
#10228=CARTESIAN_POINT('Ctrl Pts',(-0.0816371804463011,-0.132408100834492,
0.267086143429506));
#10229=CARTESIAN_POINT('Ctrl Pts',(-0.0809076931497814,-0.132855107825965,
0.267146886832381));
#10230=CARTESIAN_POINT('Ctrl Pts',(-0.0791491681472426,-0.133912820203145,
0.267291749900795));
#10231=CARTESIAN_POINT('Ctrl Pts',(-0.0781166826918304,-0.13451772497603,
0.267375532259073));
#10232=CARTESIAN_POINT('Ctrl Pts',(-0.0742375753964356,-0.136730659220493,
0.267685996099241));
#10233=CARTESIAN_POINT('Ctrl Pts',(-0.0713472830942073,-0.138260837545,
0.267908761299697));
#10234=CARTESIAN_POINT('Ctrl Pts',(-0.0635493598096736,-0.142079489259363,
0.268493146901523));
#10235=CARTESIAN_POINT('Ctrl Pts',(-0.058566809500545,-0.144204845116762,
0.268849738536345));
#10236=CARTESIAN_POINT('Ctrl Pts',(-0.0425734801544572,-0.150060937094764,
0.2699708356569));
#10237=CARTESIAN_POINT('Ctrl Pts',(-0.0312520119154191,-0.152820319826965,
0.270733762018313));
#10238=CARTESIAN_POINT('Ctrl Pts',(-0.0179990143981319,-0.154514989613307,
0.271662290042638));
#10239=CARTESIAN_POINT('Ctrl Pts',(-0.0162648526853695,-0.154707144865804,
0.271784388974812));
#10240=CARTESIAN_POINT('Ctrl Pts',(-0.013826894949649,-0.154935842165196,
0.271957042354235));
#10241=CARTESIAN_POINT('Ctrl Pts',(-0.0131254769140946,-0.154996838799361,
0.272006831718319));
#10242=CARTESIAN_POINT('Ctrl Pts',(-0.0119911094886615,-0.15508773036931,
0.272087550688457));
#10243=CARTESIAN_POINT('Ctrl Pts',(-0.0115584006573708,-0.155120579502367,
0.272118387559271));
#10244=CARTESIAN_POINT('Ctrl Pts',(-0.0106570961333128,-0.1551852099674,
0.272182717976255));
#10245=CARTESIAN_POINT('Ctrl Pts',(-0.0101884833019987,-0.155216680449379,
0.272216220911841));
#10246=CARTESIAN_POINT('Ctrl Pts',(-0.00908190995427605,-0.155285961481448,
0.272295469506566));
#10247=CARTESIAN_POINT('Ctrl Pts',(-0.00844384900640427,-0.155321963395448,
0.272341271206601));
#10248=CARTESIAN_POINT('Ctrl Pts',(-0.00633310829019463,-0.155428015249109,
0.27249314860609));
#10249=CARTESIAN_POINT('Ctrl Pts',(-0.00485969507336507,-0.15548105759351,
0.272599752115084));
#10250=CARTESIAN_POINT('Ctrl Pts',(0.00290524697204107,-0.155650114129601,
0.273164815382534));
#10251=CARTESIAN_POINT('Ctrl Pts',(0.00919791101476006,-0.155405202570579,
0.273634358054969));
#10252=CARTESIAN_POINT('Ctrl Pts',(0.0233073754734391,-0.153996105058492,
0.274713118147876));
#10253=CARTESIAN_POINT('Ctrl Pts',(0.0310855464860249,-0.152616205180488,
0.275326287983536));
#10254=CARTESIAN_POINT('Ctrl Pts',(0.0401852769142114,-0.15027714336649,
0.276054126084955));
#10255=CARTESIAN_POINT('Ctrl Pts',(0.0416401932374928,-0.149880521437169,
0.27617079471762));
#10256=CARTESIAN_POINT('Ctrl Pts',(0.0492948719477864,-0.147673728709153,
0.276785618193729));
#10257=CARTESIAN_POINT('Ctrl Pts',(0.0553840608470555,-0.145499632773997,
0.277278437823852));
#10258=CARTESIAN_POINT('Ctrl Pts',(0.0619644296493473,-0.14267691452889,
0.277803342523287));
#10259=CARTESIAN_POINT('Ctrl Pts',(0.062605874614149,-0.142396618621266,
0.277854423407324));
#10260=CARTESIAN_POINT('Ctrl Pts',(0.063550366001855,-0.14197628284294,
0.277929486769382));
#10261=CARTESIAN_POINT('Ctrl Pts',(0.0638548766492982,-0.141839587713198,
0.277953664505873));
#10262=CARTESIAN_POINT('Ctrl Pts',(0.0643943788385472,-0.141595315120732,
0.277996455990822));
#10263=CARTESIAN_POINT('Ctrl Pts',(0.0646295441600475,-0.141488131359905,
0.278015093388228));
#10264=CARTESIAN_POINT('Ctrl Pts',(0.0651327072876176,-0.141257283185047,
0.278054937176998));
#10265=CARTESIAN_POINT('Ctrl Pts',(0.0654006199441148,-0.141133442267647,
0.27807613248833));
#10266=CARTESIAN_POINT('Ctrl Pts',(0.0661346353465462,-0.140791609391587,
0.278134152559328));
#10267=CARTESIAN_POINT('Ctrl Pts',(0.0666000172412687,-0.140572063337675,
0.27817088318408));
#10268=CARTESIAN_POINT('Ctrl Pts',(0.06907051370596,-0.139391572456316,
0.278365619318536));
#10269=CARTESIAN_POINT('Ctrl Pts',(0.0710560733276606,-0.13838996408166,
0.278521252640042));
#10270=CARTESIAN_POINT('Ctrl Pts',(0.085442687186578,-0.130741365023255,
0.279647470213097));
#10271=CARTESIAN_POINT('Ctrl Pts',(0.0969137479924993,-0.12248098898627,
0.280542528707925));
#10272=CARTESIAN_POINT('Ctrl Pts',(0.112000299278424,-0.108152963710786,
0.281932174259887));
#10273=CARTESIAN_POINT('Ctrl Pts',(0.116575335321449,-0.10320514803952,
0.28238963041825));
#10274=CARTESIAN_POINT('Ctrl Pts',(0.121445238991837,-0.0972000881196913,
0.282931300033196));
#10275=CARTESIAN_POINT('Ctrl Pts',(0.122067812613842,-0.0964170744483435,
0.283001673473434));
#10276=CARTESIAN_POINT('Ctrl Pts',(0.123052722857573,-0.0951535181142867,
0.283114860599021));
#10277=CARTESIAN_POINT('Ctrl Pts',(0.123419905908483,-0.0946767733887699,
0.28315748236073));
#10278=CARTESIAN_POINT('Ctrl Pts',(0.124066097656561,-0.0938276208576194,
0.283233256203632));
#10279=CARTESIAN_POINT('Ctrl Pts',(0.12434622068369,-0.0934560667725696,
0.283266364099166));
#10280=CARTESIAN_POINT('Ctrl Pts',(0.124925538895744,-0.0926804457119648,
0.283335381670927));
#10281=CARTESIAN_POINT('Ctrl Pts',(0.125224450115931,-0.0922761744329278,
0.283371301878818));
#10282=CARTESIAN_POINT('Ctrl Pts',(0.12599375043568,-0.0912250896556484,
0.28346455983454));
#10283=CARTESIAN_POINT('Ctrl Pts',(0.126461115214211,-0.0905760919115208,
0.283522013291596));
#10284=CARTESIAN_POINT('Ctrl Pts',(0.128450954116115,-0.0877675143207924,
0.283770122406445));
#10285=CARTESIAN_POINT('Ctrl Pts',(0.129923185590691,-0.0855730590658979,
0.283962668267544));
#10286=CARTESIAN_POINT('Ctrl Pts',(0.133665161212532,-0.079676097035106,
0.2844770645729));
#10287=CARTESIAN_POINT('Ctrl Pts',(0.135836842557997,-0.0759144359912381,
0.284802220036776));
#10288=CARTESIAN_POINT('Ctrl Pts',(0.143623831697038,-0.0610196899979001,
0.286077862006308));
#10289=CARTESIAN_POINT('Ctrl Pts',(0.148049881740416,-0.0493193241638953,
0.287059743420964));
#10290=CARTESIAN_POINT('Ctrl Pts',(0.151968596788088,-0.0334165830217562,
0.288306761327306));
#10291=CARTESIAN_POINT('Ctrl Pts',(0.152761406010202,-0.0295817817380417,
0.288600668104189));
#10292=CARTESIAN_POINT('Ctrl Pts',(0.153513382011395,-0.0250967019825401,
0.288933640833726));
#10293=CARTESIAN_POINT('Ctrl Pts',(0.153614207458862,-0.0244719882861227,
0.28897977828202));
#10294=CARTESIAN_POINT('Ctrl Pts',(0.153760984325288,-0.0235258914771595,
0.289049268936782));
#10295=CARTESIAN_POINT('Ctrl Pts',(0.153809744929723,-0.0232049615462851,
0.289072774787922));
#10296=CARTESIAN_POINT('Ctrl Pts',(0.153895403157591,-0.0226290468669152,
0.289114834625351));
#10297=CARTESIAN_POINT('Ctrl Pts',(0.153932672073063,-0.0223741222631823,
0.289133409170077));
#10298=CARTESIAN_POINT('Ctrl Pts',(0.154012177092988,-0.021820694096564,
0.289173640102508));
#10299=CARTESIAN_POINT('Ctrl Pts',(0.154054178723935,-0.021522160804094,
0.289195283125781));
#10300=CARTESIAN_POINT('Ctrl Pts',(0.154169453977875,-0.0206851936174956,
0.289255802205561));
#10301=CARTESIAN_POINT('Ctrl Pts',(0.154240775493627,-0.0201464878695059,
0.289294570187238));
#10302=CARTESIAN_POINT('Ctrl Pts',(0.154644917814789,-0.0169659090896126,
0.289522432224591));
#10303=CARTESIAN_POINT('Ctrl Pts',(0.154912707033697,-0.0143160109146303,
0.289708094139946));
#10304=CARTESIAN_POINT('Ctrl Pts',(0.156210854054824,0.00295267182807369,
0.290898586001891));
#10305=CARTESIAN_POINT('Ctrl Pts',(0.155239073871537,0.0176489329047987,
0.291827839142038));
#10306=CARTESIAN_POINT('Ctrl Pts',(0.151819417137384,0.0339196315765692,
0.292944983517349));
#10307=CARTESIAN_POINT('Ctrl Pts',(0.151378059572506,0.0358379610517775,
0.293078003662129));
#10308=CARTESIAN_POINT('Ctrl Pts',(0.149942329211882,0.041577499447648,
0.293480712748644));
#10309=CARTESIAN_POINT('Ctrl Pts',(0.148838827467336,0.0453694769943925,
0.293753162661909));
#10310=CARTESIAN_POINT('Ctrl Pts',(0.14731974376163,0.0499343678096255,
0.294090949216627));
#10311=CARTESIAN_POINT('Ctrl Pts',(0.147040306983594,0.0507513158369499,
0.294151787702763));
#10312=CARTESIAN_POINT('Ctrl Pts',(0.146566229569858,0.0521005180172448,
0.294252926876222));
#10313=CARTESIAN_POINT('Ctrl Pts',(0.146375452887546,0.052634118255503,
0.294293099763111));
#10314=CARTESIAN_POINT('Ctrl Pts',(0.146024461501181,0.053599169345844,
0.294366074939678));
#10315=CARTESIAN_POINT('Ctrl Pts',(0.145865238830342,0.0540309763366914,
0.294398843952769));
#10316=CARTESIAN_POINT('Ctrl Pts',(0.145518967244312,0.0549573677624412,
0.294469400454367));
#10317=CARTESIAN_POINT('Ctrl Pts',(0.145331308507367,0.055451716420817,
0.294507207948635));
#10318=CARTESIAN_POINT('Ctrl Pts',(0.144811234732413,0.056800969658985,
0.294610832821411));
#10319=CARTESIAN_POINT('Ctrl Pts',(0.144473777195233,0.0576538940134264,
0.294676818303378));
#10320=CARTESIAN_POINT('Ctrl Pts',(0.142627136278012,0.0622032445389931,
0.295031400098233));
#10321=CARTESIAN_POINT('Ctrl Pts',(0.140983731906166,0.0658431891837452,
0.295324490298526));
#10322=CARTESIAN_POINT('Ctrl Pts',(0.132627942421066,0.0825994351494228,
0.296720070694461));
#10323=CARTESIAN_POINT('Ctrl Pts',(0.124214216050099,0.0947814562636385,
0.297881489930009));
#10324=CARTESIAN_POINT('Ctrl Pts',(0.111232668608358,0.108822867128473,
0.299342370443203));
#10325=CARTESIAN_POINT('Ctrl Pts',(0.108112950676369,0.111922838344334,
0.2996735046566));
#10326=CARTESIAN_POINT('Ctrl Pts',(0.104378960751211,0.115331129579707,
0.300043810890028));
#10327=CARTESIAN_POINT('Ctrl Pts',(0.103889337413758,0.115772373695358,
0.300091877948775));
#10328=CARTESIAN_POINT('Ctrl Pts',(0.1031535815779,0.116427003698748,0.300163361286699));
#10329=CARTESIAN_POINT('Ctrl Pts',(0.102909568127296,0.11664274249072,0.300186947363945));
#10330=CARTESIAN_POINT('Ctrl Pts',(0.102471268558987,0.117027808811723,
0.300229093287804));
#10331=CARTESIAN_POINT('Ctrl Pts',(0.102277238527927,0.117197420611471,
0.300247674063303));
#10332=CARTESIAN_POINT('Ctrl Pts',(0.10185593445929,0.117563861394978,0.300287852937023));
#10333=CARTESIAN_POINT('Ctrl Pts',(0.101628511655836,0.117760513388253,
0.300309437961563));
#10334=CARTESIAN_POINT('Ctrl Pts',(0.100991303662769,0.118308284951478,
0.300369631660898));
#10335=CARTESIAN_POINT('Ctrl Pts',(0.100580253925784,0.118657937985371,
0.300408134124878));
#10336=CARTESIAN_POINT('Ctrl Pts',(0.0981781804688915,0.12067977322723,
0.300631294968168));
#10337=CARTESIAN_POINT('Ctrl Pts',(0.0961471496060811,0.122304090499185,
0.300812684276459));
#10338=CARTESIAN_POINT('Ctrl Pts',(0.08236634025872,0.13276969477891,0.302003169420193));
#10339=CARTESIAN_POINT('Ctrl Pts',(0.069453676464604,0.139958212658715,
0.302935319667781));
#10340=CARTESIAN_POINT('Ctrl Pts',(0.0539557821117858,0.145904611552168,
0.304050541410017));
#10341=CARTESIAN_POINT('Ctrl Pts',(0.0521771960635938,0.146550066207702,
0.304178356842817));
#10342=CARTESIAN_POINT('Ctrl Pts',(0.0465718731327349,0.148469281190261,
0.304581362194133));
#10343=CARTESIAN_POINT('Ctrl Pts',(0.0427073732836244,0.149626676319463,
0.304859524558478));
#10344=CARTESIAN_POINT('Ctrl Pts',(0.03796073761188,0.150849396932931,0.305203637499376));
#10345=CARTESIAN_POINT('Ctrl Pts',(0.0371171469334411,0.151059178814054,
0.30526488485908));
#10346=CARTESIAN_POINT('Ctrl Pts',(0.0357190294658757,0.151394440539131,
0.305366562605688));
#10347=CARTESIAN_POINT('Ctrl Pts',(0.0351654858523942,0.151523972629209,
0.305406862764935));
#10348=CARTESIAN_POINT('Ctrl Pts',(0.0341624375822613,0.151752898768408,
0.305479973631794));
#10349=CARTESIAN_POINT('Ctrl Pts',(0.0337131759131925,0.151853337756109,
0.305512750476149));
#10350=CARTESIAN_POINT('Ctrl Pts',(0.03326228799292,0.151952040785781,0.305545678324688));
#10351=CARTESIAN_POINT('Ctrl Pts',(0.033261096582728,0.151952301580466,
0.305545765332291));
#10352=CARTESIAN_POINT('Ctrl Pts',(0.0332587207255954,0.151952821616339,
0.305545938839424));
#10353=CARTESIAN_POINT('Ctrl Pts',(0.0332575360529371,0.151953080907093,
0.305546025355438));
#10354=CARTESIAN_POINT('Ctrl Pts',(0.033255173324262,0.151953598011456,
0.305546197904702));
#10355=CARTESIAN_POINT('Ctrl Pts',(0.0332539952612068,0.151953855826765,
0.305546283938464));
#10356=CARTESIAN_POINT('Ctrl Pts',(0.0332516457020982,0.151954369991586,
0.305546455526842));
#10357=CARTESIAN_POINT('Ctrl Pts',(0.0332504741961427,0.151954626343423,
0.305546541082179));
#10358=CARTESIAN_POINT('Ctrl Pts',(0.0332481376978107,0.151955137593465,
0.305546711717601));
#10359=CARTESIAN_POINT('Ctrl Pts',(0.0332469726959516,0.151955392493903,
0.305546796798376));
#10360=CARTESIAN_POINT('Ctrl Pts',(0.0332446491540944,0.151955900852935,
0.305546966488444));
#10361=CARTESIAN_POINT('Ctrl Pts',(0.0332434906051759,0.151956154313635,
0.305547051098386));
#10362=CARTESIAN_POINT('Ctrl Pts',(0.0332411799101148,0.151956659806583,
0.305547219851097));
#10363=CARTESIAN_POINT('Ctrl Pts',(0.0332400277596687,0.151956911839925,
0.305547303994177));
#10364=CARTESIAN_POINT('Ctrl Pts',(0.0332377298150578,0.151957414488784,
0.305547471816552));
#10365=CARTESIAN_POINT('Ctrl Pts',(0.0332365840137241,0.151957665106021,
0.305547555496368));
#10366=CARTESIAN_POINT('Ctrl Pts',(0.0332342987097748,0.151958164935713,
0.305547722396412));
#10367=CARTESIAN_POINT('Ctrl Pts',(0.033233159203392,0.151958414149141,
0.305547805616913));
#10368=CARTESIAN_POINT('Ctrl Pts',(0.0327233048205491,0.152069914806779,
0.305585041426369));
#10369=CARTESIAN_POINT('Ctrl Pts',(0.0322140402765985,0.152178609747234,
0.305622275459916));
#10370=CARTESIAN_POINT('Ctrl Pts',(0.0308364365117833,0.152465413837663,
0.305723113685092));
#10371=CARTESIAN_POINT('Ctrl Pts',(0.0299671163995292,0.152638658627842,
0.305786871857615));
#10372=CARTESIAN_POINT('Ctrl Pts',(0.028033802189224,0.153006792148099,
0.305928963410166));
#10373=CARTESIAN_POINT('Ctrl Pts',(0.0269691689366109,0.153198029770798,
0.306007409271551));
#10374=CARTESIAN_POINT('Ctrl Pts',(0.0237278501052427,0.153745426894165,
0.306246882292746));
#10375=CARTESIAN_POINT('Ctrl Pts',(0.0215455896880002,0.154066394179012,
0.306408991000768));
#10376=CARTESIAN_POINT('Ctrl Pts',(0.0044431140174602,0.156211377083595,
0.307686718837038));
#10377=CARTESIAN_POINT('Ctrl Pts',(-0.0106621158301532,0.155909861711717,
0.308869548094476));
#10378=CARTESIAN_POINT('Ctrl Pts',(-0.026345427090253,0.153305194294345,
0.310087247990286));
#10379=CARTESIAN_POINT('Ctrl Pts',(-0.0272051420288109,0.153154968647471,
0.310153928453098));
#10380=CARTESIAN_POINT('Ctrl Pts',(-0.0288359658101667,0.152855834886191,
0.310280234987703));
#10381=CARTESIAN_POINT('Ctrl Pts',(-0.0296073003428357,0.152708306881315,
0.310339896785407));
#10382=CARTESIAN_POINT('Ctrl Pts',(-0.0335717377101413,0.151918888434002,
0.310646042062632));
#10383=CARTESIAN_POINT('Ctrl Pts',(-0.0367455246038526,0.151182606979643,
0.310889473506111));
#10384=CARTESIAN_POINT('Ctrl Pts',(-0.0404250154250893,0.150206265884471,
0.311168015035298));
#10385=CARTESIAN_POINT('Ctrl Pts',(-0.0409551614627046,0.150062583467118,
0.311208057133632));
#10386=CARTESIAN_POINT('Ctrl Pts',(-0.0418050735753087,0.149827397122019,
0.311272093664716));
#10387=CARTESIAN_POINT('Ctrl Pts',(-0.0421253201090561,0.149737672335052,
0.311296186562792));
#10388=CARTESIAN_POINT('Ctrl Pts',(-0.0426943871336672,0.149576264339099,
0.311338931666725));
#10389=CARTESIAN_POINT('Ctrl Pts',(-0.0429433188117957,0.149504986270929,
0.311357606982288));
#10390=CARTESIAN_POINT('Ctrl Pts',(-0.0434730621661568,0.149351869471086,
0.31139729944714));
#10391=CARTESIAN_POINT('Ctrl Pts',(-0.0437538207588134,0.149269860392073,
0.311418306509449));
#10392=CARTESIAN_POINT('Ctrl Pts',(-0.0445163297165142,0.149044796729112,
0.311475283258547));
#10393=CARTESIAN_POINT('Ctrl Pts',(-0.0449976265962869,0.148900196987338,
0.311511164377631));
#10394=CARTESIAN_POINT('Ctrl Pts',(-0.0474112023001512,0.14816229631183,
0.311690722839279));
#10395=CARTESIAN_POINT('Ctrl Pts',(-0.0493326039622012,0.147533668668207,
0.311832453904321));
#10396=CARTESIAN_POINT('Ctrl Pts',(-0.0549178007752948,0.145585024772356,
0.312242392109044));
#10397=CARTESIAN_POINT('Ctrl Pts',(-0.0585451262568406,0.14416461936081,
0.312506024919305));
#10398=CARTESIAN_POINT('Ctrl Pts',(-0.0626412936682278,0.142380474849873,
0.312804839115273));
#10399=CARTESIAN_POINT('Ctrl Pts',(-0.0631656457855339,0.142148627458991,
0.312843111303748));
#10400=CARTESIAN_POINT('Ctrl Pts',(-0.0636886270244494,0.14191392210682,
0.31288131537517));
#10401=CARTESIAN_POINT('Origin',(0.,0.,-0.129405622560373));
#10402=CARTESIAN_POINT('',(-0.0636886207929056,0.141913924903434,0.396608754846595));
#10403=CARTESIAN_POINT('',(-0.0636886258329921,0.141913922641526,0.382796071549385));
#10404=CARTESIAN_POINT('',(-0.0636886258329924,0.141913922641526,-0.129405622560373));
#10405=CARTESIAN_POINT('Ctrl Pts',(-0.0636886207929056,0.141913924903434,
0.396608754846595));
#10406=CARTESIAN_POINT('Ctrl Pts',(-0.0591354711488871,0.143957303108135,
0.396280149747421));
#10407=CARTESIAN_POINT('Ctrl Pts',(-0.0544854027433177,0.145780922739278,
0.395950672078547));
#10408=CARTESIAN_POINT('Ctrl Pts',(-0.0458237033067888,0.148705081971013,
0.395338079499676));
#10409=CARTESIAN_POINT('Ctrl Pts',(-0.0418418461088594,0.149874176190154,
0.395056901137322));
#10410=CARTESIAN_POINT('Ctrl Pts',(-0.0353378727723009,0.151504376525937,
0.394594616688936));
#10411=CARTESIAN_POINT('Ctrl Pts',(-0.0328426610223724,0.152064787711378,
0.394416579065734));
#10412=CARTESIAN_POINT('Ctrl Pts',(-0.0295595151424556,0.152717590803652,
0.394180923169887));
#10413=CARTESIAN_POINT('Ctrl Pts',(-0.0287829885131883,0.152865846437844,
0.394125085341324));
#10414=CARTESIAN_POINT('Ctrl Pts',(-0.0275127108832061,0.153098347777723,
0.394033564052576));
#10415=CARTESIAN_POINT('Ctrl Pts',(-0.0270196162337983,0.153186140627323,
0.393997993485945));
#10416=CARTESIAN_POINT('Ctrl Pts',(-0.0260667273767181,0.153351053398406,
0.393929165705241));
#10417=CARTESIAN_POINT('Ctrl Pts',(-0.0256069929010297,0.153428490706252,
0.39389591894561));
#10418=CARTESIAN_POINT('Ctrl Pts',(-0.0245481922785319,0.153601942869539,
0.393819254137818));
#10419=CARTESIAN_POINT('Ctrl Pts',(-0.0239489019942723,0.153696521338003,
0.393775791177357));
#10420=CARTESIAN_POINT('Ctrl Pts',(-0.0223436573269114,0.153940240538981,
0.39365917685131));
#10421=CARTESIAN_POINT('Ctrl Pts',(-0.0213367831270878,0.154083023965586,
0.393585826435465));
#10422=CARTESIAN_POINT('Ctrl Pts',(-0.0129940613902414,0.155182753992489,
0.392976266209449));
#10423=CARTESIAN_POINT('Ctrl Pts',(-0.00560113016398566,0.155624958516443,
0.392423930633981));
#10424=CARTESIAN_POINT('Ctrl Pts',(0.0117238713532809,0.155425111399385,
0.391101724465564));
#10425=CARTESIAN_POINT('Ctrl Pts',(0.0216195989182905,0.154359927374671,
0.390324268914821));
#10426=CARTESIAN_POINT('Ctrl Pts',(0.0349944030782908,0.151608292096276,
0.389275222631333));
#10427=CARTESIAN_POINT('Ctrl Pts',(0.038615707523504,0.1507266198929,0.388991622031633));
#10428=CARTESIAN_POINT('Ctrl Pts',(0.0434601339677926,0.149361064610111,
0.388615587028682));
#10429=CARTESIAN_POINT('Ctrl Pts',(0.0447136869116124,0.148990594827376,
0.388518595072565));
#10430=CARTESIAN_POINT('Ctrl Pts',(0.0465613753970196,0.14841911541535,
0.3883762392744));
#10431=CARTESIAN_POINT('Ctrl Pts',(0.0471591677446034,0.148230254778108,
0.388330276870934));
#10432=CARTESIAN_POINT('Ctrl Pts',(0.0482397725726555,0.147881660224996,
0.388247384344753));
#10433=CARTESIAN_POINT('Ctrl Pts',(0.0487229709107621,0.147723164107304,
0.388210388325363));
#10434=CARTESIAN_POINT('Ctrl Pts',(0.0494822059590996,0.147469993352559,
0.38815237704341));
#10435=CARTESIAN_POINT('Ctrl Pts',(0.0497587624318069,0.14737690867659,
0.388131271075488));
#10436=CARTESIAN_POINT('Ctrl Pts',(0.0502718638027505,0.147202597661875,
0.388092161343756));
#10437=CARTESIAN_POINT('Ctrl Pts',(0.0505084722090288,0.14712157994426,
0.388074146029746));
#10438=CARTESIAN_POINT('Ctrl Pts',(0.0510528421066504,0.146933712749406,
0.388032741750722));
#10439=CARTESIAN_POINT('Ctrl Pts',(0.0513604636238838,0.146826466997955,
0.388009376481895));
#10440=CARTESIAN_POINT('Ctrl Pts',(0.0522894613393386,0.146499314649221,
0.387938905543215));
#10441=CARTESIAN_POINT('Ctrl Pts',(0.0529097898187304,0.146276420323115,
0.387891972268997));
#10442=CARTESIAN_POINT('Ctrl Pts',(0.0576761658799279,0.144529493735014,
0.387532164477043));
#10443=CARTESIAN_POINT('Ctrl Pts',(0.0617574983698718,0.142833242585835,
0.387228790084258));
#10444=CARTESIAN_POINT('Ctrl Pts',(0.0791557975828898,0.134716788601274,
0.385933130595585));
#10445=CARTESIAN_POINT('Ctrl Pts',(0.0915912323790402,0.126591264585131,
0.38499336037026));
#10446=CARTESIAN_POINT('Ctrl Pts',(0.105644319033502,0.114238842820077,
0.383718880371709));
#10447=CARTESIAN_POINT('Ctrl Pts',(0.108495410459469,0.111534643764521,
0.383447582577348));
#10448=CARTESIAN_POINT('Ctrl Pts',(0.111879032373547,0.108072744340735,
0.383107465105336));
#10449=CARTESIAN_POINT('Ctrl Pts',(0.112511380428234,0.107414268907066,
0.383043079009707));
#10450=CARTESIAN_POINT('Ctrl Pts',(0.113500187767364,0.106366294398961,
0.382941064096871));
#10451=CARTESIAN_POINT('Ctrl Pts',(0.113860530570887,0.105980473545882,
0.382903602412488));
#10452=CARTESIAN_POINT('Ctrl Pts',(0.114531483318713,0.105254709461171,
0.382833307733877));
#10453=CARTESIAN_POINT('Ctrl Pts',(0.114842562251683,0.104915205866627,
0.382800495180288));
#10454=CARTESIAN_POINT('Ctrl Pts',(0.115534144312808,0.104153669596703,
0.382727047060551));
#10455=CARTESIAN_POINT('Ctrl Pts',(0.11591384986254,0.103730924929615,0.382686378554194));
#10456=CARTESIAN_POINT('Ctrl Pts',(0.116867775723354,0.1026570949005,0.382583330106278));
#10457=CARTESIAN_POINT('Ctrl Pts',(0.117438871039729,0.102003272732052,
0.382520821486495));
#10458=CARTESIAN_POINT('Ctrl Pts',(0.120619165552353,0.0983001796953169,
0.382168051212617));
#10459=CARTESIAN_POINT('Ctrl Pts',(0.123114830981151,0.0951558791407954,
0.38187322304819));
#10460=CARTESIAN_POINT('Ctrl Pts',(0.126614192964098,0.0903786144783409,
0.381431511679175));
#10461=CARTESIAN_POINT('Ctrl Pts',(0.127713938225963,0.0888177756493666,
0.381288134440068));
#10462=CARTESIAN_POINT('Ctrl Pts',(0.137038856553683,0.0750517793050917,
0.38003187667353));
#10463=CARTESIAN_POINT('Ctrl Pts',(0.143520768099879,0.0617586354025572,
0.378864732072268));
#10464=CARTESIAN_POINT('Ctrl Pts',(0.148834886832389,0.0452847731455561,
0.377562543551511));
#10465=CARTESIAN_POINT('Ctrl Pts',(0.14956957840972,0.042795765935048,0.377369697281248));
#10466=CARTESIAN_POINT('Ctrl Pts',(0.150381423032445,0.0397683426615026,
0.377140725561483));
#10467=CARTESIAN_POINT('Ctrl Pts',(0.150518430487696,0.0392465995726382,
0.377101463617054));
#10468=CARTESIAN_POINT('Ctrl Pts',(0.150727573656063,0.0384329472951513,
0.377040555362658));
#10469=CARTESIAN_POINT('Ctrl Pts',(0.150801580000325,0.0381415307981588,
0.377018804356258));
#10470=CARTESIAN_POINT('Ctrl Pts',(0.150937473850377,0.037599839789361,
0.376978493872609));
#10471=CARTESIAN_POINT('Ctrl Pts',(0.150999583502159,0.0373496284927104,
0.376959922169652));
#10472=CARTESIAN_POINT('Ctrl Pts',(0.151138808317416,0.036782731709718,
0.376917952452996));
#10473=CARTESIAN_POINT('Ctrl Pts',(0.151215550232206,0.036465958164934,
0.376894576075642));
#10474=CARTESIAN_POINT('Ctrl Pts',(0.151444657814457,0.0355070923864214,
0.376824038504343));
#10475=CARTESIAN_POINT('Ctrl Pts',(0.151593936325631,0.0348642582177862,
0.376777050186271));
#10476=CARTESIAN_POINT('Ctrl Pts',(0.152710636894445,0.0299126276891752,
0.376417279520102));
#10477=CARTESIAN_POINT('Ctrl Pts',(0.153498377268147,0.0255648431689894,
0.376113990227377));
#10478=CARTESIAN_POINT('Ctrl Pts',(0.156113409732975,0.00654659047186478,
0.374818410627166));
#10479=CARTESIAN_POINT('Ctrl Pts',(0.156029742918761,-0.00830798203150761,
0.373878638037471));
#10480=CARTESIAN_POINT('Ctrl Pts',(0.153271835687203,-0.026813789611275,
0.37260415857605));
#10481=CARTESIAN_POINT('Ctrl Pts',(0.152545846269266,-0.030675645257038,
0.372332864431312));
#10482=CARTESIAN_POINT('Ctrl Pts',(0.151472018559481,-0.0353958124737809,
0.371992751005912));
#10483=CARTESIAN_POINT('Ctrl Pts',(0.151261673780469,-0.0362841829013968,
0.371928365178482));
#10484=CARTESIAN_POINT('Ctrl Pts',(0.150917370453587,-0.0376832655415541,
0.371826350594796));
#10485=CARTESIAN_POINT('Ctrl Pts',(0.150788608228567,-0.0381952460718942,
0.371788888969522));
#10486=CARTESIAN_POINT('Ctrl Pts',(0.150542661134858,-0.0391525441504082,
0.371718594343923));
#10487=CARTESIAN_POINT('Ctrl Pts',(0.15042609996145,-0.0395980173371105,
0.371685781783945));
#10488=CARTESIAN_POINT('Ctrl Pts',(0.150161283275421,-0.0405920484693481,
0.371612333574844));
#10489=CARTESIAN_POINT('Ctrl Pts',(0.150011997028421,-0.0411403223803712,
0.371571664985144));
#10490=CARTESIAN_POINT('Ctrl Pts',(0.149627052085371,-0.0425241275821229,
0.371468616185309));
#10491=CARTESIAN_POINT('Ctrl Pts',(0.149387399268055,-0.0433585173351884,
0.371406107295415));
#10492=CARTESIAN_POINT('Ctrl Pts',(0.148000631683482,-0.048038753995225,
0.371053332793077));
#10493=CARTESIAN_POINT('Ctrl Pts',(0.146712102408559,-0.0518407406068074,
0.370758500542132));
#10494=CARTESIAN_POINT('Ctrl Pts',(0.144595845262558,-0.0573715012970494,
0.370316788560117));
#10495=CARTESIAN_POINT('Ctrl Pts',(0.143880807506569,-0.059141866161648,
0.370173414957269));
#10496=CARTESIAN_POINT('Ctrl Pts',(0.137371268870141,-0.0744416097236432,
0.36891715825066));
#10497=CARTESIAN_POINT('Ctrl Pts',(0.129717303886049,-0.0870962799570504,
0.36775001080692));
#10498=CARTESIAN_POINT('Ctrl Pts',(0.118757648883784,-0.100494551256526,
0.366447823457123));
#10499=CARTESIAN_POINT('Ctrl Pts',(0.117064812744389,-0.102461533113913,
0.366254980351734));
#10500=CARTESIAN_POINT('Ctrl Pts',(0.114961440124734,-0.104785307906241,
0.366026011882111));
#10501=CARTESIAN_POINT('Ctrl Pts',(0.114597368278322,-0.10518334789989,
0.365986750124842));
#10502=CARTESIAN_POINT('Ctrl Pts',(0.114027151715282,-0.105800290970308,
0.365925842097099));
#10503=CARTESIAN_POINT('Ctrl Pts',(0.11382243533742,-0.106020498563939,
0.365904091131427));
#10504=CARTESIAN_POINT('Ctrl Pts',(0.113440997979261,-0.106428421683388,
0.36586378068468));
#10505=CARTESIAN_POINT('Ctrl Pts',(0.113264450574062,-0.106616289574125,
0.3658452089781));
#10506=CARTESIAN_POINT('Ctrl Pts',(0.112863640692477,-0.107040680779638,
0.365803239204184));
#10507=CARTESIAN_POINT('Ctrl Pts',(0.112639101822718,-0.107276938239204,
0.36577986277344));
#10508=CARTESIAN_POINT('Ctrl Pts',(0.111957697656428,-0.107989406567054,
0.365709324881809));
#10509=CARTESIAN_POINT('Ctrl Pts',(0.111498534867578,-0.108463425905312,
0.365662336299106));
#10510=CARTESIAN_POINT('Ctrl Pts',(0.107943644453324,-0.112086906195201,
0.365302557353279));
#10511=CARTESIAN_POINT('Ctrl Pts',(0.104717715343248,-0.115106533812928,
0.364999260539068));
#10512=CARTESIAN_POINT('Ctrl Pts',(0.0901563580736357,-0.127616971474278,
0.363703661381624));
#10513=CARTESIAN_POINT('Ctrl Pts',(0.0776299566863628,-0.135601986811538,
0.362763876658843));
#10514=CARTESIAN_POINT('Ctrl Pts',(0.0605858387280864,-0.143319883110265,
0.361489399953024));
#10515=CARTESIAN_POINT('Ctrl Pts',(0.0569476690540846,-0.144803975211418,
0.361218124536059));
#10516=CARTESIAN_POINT('Ctrl Pts',(0.0523997468572953,-0.146461266007262,
0.360878031875576));
#10517=CARTESIAN_POINT('Ctrl Pts',(0.0515392906741986,-0.146766267801874,
0.360813647424466));
#10518=CARTESIAN_POINT('Ctrl Pts',(0.0501770952732396,-0.147235662500156,
0.360711634529874));
#10519=CARTESIAN_POINT('Ctrl Pts',(0.0496771081464612,-0.147405108851847,
0.360674173207941));
#10520=CARTESIAN_POINT('Ctrl Pts',(0.0487394178499021,-0.147717580819097,
0.360603878854384));
#10521=CARTESIAN_POINT('Ctrl Pts',(0.0483019221113363,-0.147861214817721,
0.360571066261615));
#10522=CARTESIAN_POINT('Ctrl Pts',(0.0473231264180402,-0.148177755100382,
0.360497617593915));
#10523=CARTESIAN_POINT('Ctrl Pts',(0.046781506150068,-0.148349641277132,
0.360456948576507));
#10524=CARTESIAN_POINT('Ctrl Pts',(0.0454100613849526,-0.148776619468472,
0.36035389797066));
#10525=CARTESIAN_POINT('Ctrl Pts',(0.0445790300259477,-0.149027736346607,
0.360291387694576));
#10526=CARTESIAN_POINT('Ctrl Pts',(0.0398943925850023,-0.150400626825541,
0.359938591491321));
#10527=CARTESIAN_POINT('Ctrl Pts',(0.0360009469321137,-0.151379778847063,
0.359643738267843));
#10528=CARTESIAN_POINT('Ctrl Pts',(0.0302063665586847,-0.152600858744321,
0.359202023139442));
#10529=CARTESIAN_POINT('Ctrl Pts',(0.028331402036626,-0.152960052963473,
0.359058668197927));
#10530=CARTESIAN_POINT('Ctrl Pts',(0.0119466540993918,-0.155787359212479,
0.357802416928715));
#10531=CARTESIAN_POINT('Ctrl Pts',(-0.00283654316817243,-0.156218756873579,
0.356635254894959));
#10532=CARTESIAN_POINT('Ctrl Pts',(-0.0200368803470148,-0.154275909703786,
0.355333073554957));
#10533=CARTESIAN_POINT('Ctrl Pts',(-0.0226073099168896,-0.153920253953389,
0.355140246693816));
#10534=CARTESIAN_POINT('Ctrl Pts',(-0.0257001295377401,-0.15341315718086,
0.354911294906176));
#10535=CARTESIAN_POINT('Ctrl Pts',(-0.026231977268921,-0.153323112563649,
0.354872034109604));
#10536=CARTESIAN_POINT('Ctrl Pts',(-0.0270595319050074,-0.153178571050486,
0.354811127245268));
#10537=CARTESIAN_POINT('Ctrl Pts',(-0.0273555602952314,-0.153125981535161,
0.354789376488655));
#10538=CARTESIAN_POINT('Ctrl Pts',(-0.027905139099566,-0.153026704128821,
0.354749066231342));
#10539=CARTESIAN_POINT('Ctrl Pts',(-0.0281587234021228,-0.152980244681817,
0.354730494506161));
#10540=CARTESIAN_POINT('Ctrl Pts',(-0.0287326505477795,-0.152873619461138,
0.354688524438306));
#10541=CARTESIAN_POINT('Ctrl Pts',(-0.0290529198960198,-0.152813077272343,
0.354665147733501));
#10542=CARTESIAN_POINT('Ctrl Pts',(-0.0300210675994438,-0.152626909556827,
0.354594608197535));
#10543=CARTESIAN_POINT('Ctrl Pts',(-0.0306683504579261,-0.152498165045919,
0.354547618256416));
#10544=CARTESIAN_POINT('Ctrl Pts',(-0.0356411192274561,-0.151476138995254,
0.354187796801346));
#10545=CARTESIAN_POINT('Ctrl Pts',(-0.0399281132623178,-0.150403008460899,
0.353884461370454));
#10546=CARTESIAN_POINT('Ctrl Pts',(-0.058337109069451,-0.144951963177837,
0.352588761758896));
#10547=CARTESIAN_POINT('Ctrl Pts',(-0.0718396701616462,-0.138756622887168,
0.3516489147026));
#10548=CARTESIAN_POINT('Ctrl Pts',(-0.087566179370972,-0.128621093876159,
0.350374452128954));
#10549=CARTESIAN_POINT('Ctrl Pts',(-0.0907847952954962,-0.12636984611009,
0.35010327289934));
#10550=CARTESIAN_POINT('Ctrl Pts',(-0.0946422495902132,-0.12344829005988,
0.349763286890065));
#10551=CARTESIAN_POINT('Ctrl Pts',(-0.0953650344051116,-0.122890788408527,
0.349698909509598));
#10552=CARTESIAN_POINT('Ctrl Pts',(-0.096498005842365,-0.122000885434624,
0.349596905292492));
#10553=CARTESIAN_POINT('Ctrl Pts',(-0.0969114873115889,-0.121672695346751,
0.349559445528945));
#10554=CARTESIAN_POINT('Ctrl Pts',(-0.0976824958721955,-0.121054304085085,
0.349489152572844));
#10555=CARTESIAN_POINT('Ctrl Pts',(-0.0980404214898577,-0.120764606913884,
0.349456339811474));
#10556=CARTESIAN_POINT('Ctrl Pts',(-0.0988371794682913,-0.120113851781497,
0.3493828887871));
#10557=CARTESIAN_POINT('Ctrl Pts',(-0.0992753282308914,-0.119751971273283,
0.349342217571856));
#10558=CARTESIAN_POINT('Ctrl Pts',(-0.100377872324346,-0.118831136883617,
0.34923915768544));
#10559=CARTESIAN_POINT('Ctrl Pts',(-0.101039581340861,-0.118269012387253,
0.349176640286103));
#10560=CARTESIAN_POINT('Ctrl Pts',(-0.10473459587014,-0.115076440155669,
0.348823732547575));
#10561=CARTESIAN_POINT('Ctrl Pts',(-0.107669601004868,-0.1123350977175,
0.348528771530388));
#10562=CARTESIAN_POINT('Ctrl Pts',(-0.111837779702478,-0.108128408754094,
0.348087040218821));
#10563=CARTESIAN_POINT('Ctrl Pts',(-0.113155403896522,-0.106748750776543,
0.347943781180044));
#10564=CARTESIAN_POINT('Ctrl Pts',(-0.124415590152557,-0.0945156644537806,
0.346687557766949));
#10565=CARTESIAN_POINT('Ctrl Pts',(-0.132794930127446,-0.0823278724373318,
0.345520320657869));
#10566=CARTESIAN_POINT('Ctrl Pts',(-0.14048939314704,-0.0668225828946814,
0.344218170218855));
#10567=CARTESIAN_POINT('Ctrl Pts',(-0.141583953763048,-0.0644710272572081,
0.344025426923031));
#10568=CARTESIAN_POINT('Ctrl Pts',(-0.142834574585835,-0.0615985201508543,
0.343796560954731));
#10569=CARTESIAN_POINT('Ctrl Pts',(-0.143047299183293,-0.0611028935602491,
0.343757305101806));
#10570=CARTESIAN_POINT('Ctrl Pts',(-0.143374584429493,-0.0603292750398509,
0.343696404224281));
#10571=CARTESIAN_POINT('Ctrl Pts',(-0.143490921431259,-0.0600520470771563,
0.343674654543487));
#10572=CARTESIAN_POINT('Ctrl Pts',(-0.143705525649564,-0.0595364666674289,
0.343634345260886));
#10573=CARTESIAN_POINT('Ctrl Pts',(-0.143804003096175,-0.0592982095920591,
0.343615773439877));
#10574=CARTESIAN_POINT('Ctrl Pts',(-0.144025650315872,-0.05875815516773,
0.343573801858931));
#10575=CARTESIAN_POINT('Ctrl Pts',(-0.144148463861312,-0.0584562154037349,
0.343550423743441));
#10576=CARTESIAN_POINT('Ctrl Pts',(-0.144517090990275,-0.0575417115089637,
0.343479875743202));
#10577=CARTESIAN_POINT('Ctrl Pts',(-0.144759960019966,-0.0569279559462022,
0.34343287880955));
#10578=CARTESIAN_POINT('Ctrl Pts',(-0.146598967263648,-0.0521927139463801,
0.343072838336293));
#10579=CARTESIAN_POINT('Ctrl Pts',(-0.148022884216022,-0.0480059524947524,
0.342769303942075));
#10580=CARTESIAN_POINT('Ctrl Pts',(-0.153426818966979,-0.0295745516656521,
0.341473085969551));
#10581=CARTESIAN_POINT('Ctrl Pts',(-0.15554270412961,-0.0148646774897879,
0.34053291696168));
#10582=CARTESIAN_POINT('Ctrl Pts',(-0.155551875192911,0.00377240964231844,
0.339263323416171));
#10583=CARTESIAN_POINT('Ctrl Pts',(-0.155410911248689,0.00761980084480383,
0.338997568250853));
#10584=CARTESIAN_POINT('Ctrl Pts',(-0.15505820770871,0.0123950842303167,
0.338661337111921));
#10585=CARTESIAN_POINT('Ctrl Pts',(-0.154980483131377,0.013331754203132,
0.338595081553473));
#10586=CARTESIAN_POINT('Ctrl Pts',(-0.154844793031477,0.0148048509162445,
0.338490377958999));
#10587=CARTESIAN_POINT('Ctrl Pts',(-0.154792515958477,0.0153417902974159,
0.338452108308192));
#10588=CARTESIAN_POINT('Ctrl Pts',(-0.154695208360985,0.0162900653490015,
0.338384329994491));
#10589=CARTESIAN_POINT('Ctrl Pts',(-0.154651327425278,0.016701516052533,
0.338354857695168));
#10590=CARTESIAN_POINT('Ctrl Pts',(-0.154546920691025,0.0176447809281248,
0.338287142703986));
#10591=CARTESIAN_POINT('Ctrl Pts',(-0.154485290872378,0.0181764650009163,
0.338248865662852));
#10592=CARTESIAN_POINT('Ctrl Pts',(-0.154307104528458,0.0196472781321917,
0.338142671966467));
#10593=CARTESIAN_POINT('Ctrl Pts',(-0.154184721716883,0.0205856639802072,
0.338074573047169));
#10594=CARTESIAN_POINT('Ctrl Pts',(-0.153440237542671,0.0259144459705404,
0.337685828332761));
#10595=CARTESIAN_POINT('Ctrl Pts',(-0.152639249564241,0.0302773369576339,
0.337359596198671));
#10596=CARTESIAN_POINT('Ctrl Pts',(-0.14948715934694,0.0440931945675072,
0.336299659137388));
#10597=CARTESIAN_POINT('Ctrl Pts',(-0.146434817648429,0.0533611876740401,
0.335546078973155));
#10598=CARTESIAN_POINT('Ctrl Pts',(-0.139000414404946,0.0703754381062482,
0.334106366647411));
#10599=CARTESIAN_POINT('Ctrl Pts',(-0.134780408387858,0.0781543454835109,
0.333423529591988));
#10600=CARTESIAN_POINT('Ctrl Pts',(-0.129542511915241,0.0861104924450523,
0.332725362760499));
#10601=CARTESIAN_POINT('Ctrl Pts',(-0.129158969563395,0.0866847156743254,
0.332674980489749));
#10602=CARTESIAN_POINT('Ctrl Pts',(-0.128585372740147,0.0875312209319739,
0.33260074047546));
#10603=CARTESIAN_POINT('Ctrl Pts',(-0.12839825715358,0.0878054684292402,
0.33257669354251));
#10604=CARTESIAN_POINT('Ctrl Pts',(-0.128063985103896,0.0882920435464803,
0.332534041000714));
#10605=CARTESIAN_POINT('Ctrl Pts',(-0.127917176729224,0.0885046051669697,
0.332515412364162));
#10606=CARTESIAN_POINT('Ctrl Pts',(-0.127600752928645,0.0889603183435611,
0.332475483909656));
#10607=CARTESIAN_POINT('Ctrl Pts',(-0.127430972153441,0.089203350429118,
0.332454195625835));
#10608=CARTESIAN_POINT('Ctrl Pts',(-0.126961342157553,0.0898715235608675,
0.332395678200694));
#10609=CARTESIAN_POINT('Ctrl Pts',(-0.126660049537383,0.0902956533920446,
0.33235854585871));
#10610=CARTESIAN_POINT('Ctrl Pts',(-0.125014424034513,0.0925877571447012,
0.332157891703847));
#10611=CARTESIAN_POINT('Ctrl Pts',(-0.123630797913218,0.0944273600073881,
0.331996915939853));
#10612=CARTESIAN_POINT('Ctrl Pts',(-0.113344052392295,0.107490180992172,
0.330848798709652));
#10613=CARTESIAN_POINT('Ctrl Pts',(-0.102968214487035,0.117467748648099,
0.329938812661447));
#10614=CARTESIAN_POINT('Ctrl Pts',(-0.0889586129320677,0.127636435131847,
0.328780496157874));
#10615=CARTESIAN_POINT('Ctrl Pts',(-0.0864956177248851,0.129318215944089,
0.328579379734413));
#10616=CARTESIAN_POINT('Ctrl Pts',(-0.0808705594660266,0.132926498929271,
0.328123569780184));
#10617=CARTESIAN_POINT('Ctrl Pts',(-0.0776851114311599,0.134812911772795,
0.327867795298827));
#10618=CARTESIAN_POINT('Ctrl Pts',(-0.0736212035253429,0.137027665775012,
0.327542742600306));
#10619=CARTESIAN_POINT('Ctrl Pts',(-0.0728028370025879,0.137464212266892,
0.327477349763916));
#10620=CARTESIAN_POINT('Ctrl Pts',(-0.0715049029263191,0.138141736426061,
0.327373713428127));
#10621=CARTESIAN_POINT('Ctrl Pts',(-0.0710278985778237,0.138387600946786,
0.327335642300027));
#10622=CARTESIAN_POINT('Ctrl Pts',(-0.0701437110260563,0.138837566073509,
0.327265097861832));
#10623=CARTESIAN_POINT('Ctrl Pts',(-0.0697368838007441,0.139042356781615,
0.327232649157847));
#10624=CARTESIAN_POINT('Ctrl Pts',(-0.0688320734181299,0.139492854751347,
0.327160499505217));
#10625=CARTESIAN_POINT('Ctrl Pts',(-0.0683336641663858,0.139737687058772,
0.327120768594766));
#10626=CARTESIAN_POINT('Ctrl Pts',(-0.0668984475443242,0.140433190254196,
0.327006387841378));
#10627=CARTESIAN_POINT('Ctrl Pts',(-0.0659584350150779,0.140877137824565,
0.326931506862302));
#10628=CARTESIAN_POINT('Ctrl Pts',(-0.0645731589023019,0.141514469913206,
0.326821186335112));
#10629=CARTESIAN_POINT('Ctrl Pts',(-0.0641313410607403,0.141715239356901,
0.326786005352217));
#10630=CARTESIAN_POINT('Ctrl Pts',(-0.0636886254453755,0.141913922815482,
0.326750756222096));
#10631=CARTESIAN_POINT('',(-0.155549941519498,0.000134882470554111,0.325594377439629));
#10632=CARTESIAN_POINT('Ctrl Pts',(-0.0636886270244492,0.14191392210682,
0.31288131537517));
#10633=CARTESIAN_POINT('Ctrl Pts',(-0.0738457763258268,0.137355561067371,
0.313623300801195));
#10634=CARTESIAN_POINT('Ctrl Pts',(-0.0834857012421142,0.1317192952549,
0.314342086516591));
#10635=CARTESIAN_POINT('Ctrl Pts',(-0.0968652474729675,0.121832535428259,
0.315461554910601));
#10636=CARTESIAN_POINT('Ctrl Pts',(-0.101111003997252,0.118332566954402,
0.315837738301656));
#10637=CARTESIAN_POINT('Ctrl Pts',(-0.105865281244906,0.113970413452104,
0.316290101255649));
#10638=CARTESIAN_POINT('Ctrl Pts',(-0.106562377892366,0.113318897195196,
0.316357260196019));
#10639=CARTESIAN_POINT('Ctrl Pts',(-0.107683980767327,0.112251129959869,
0.316466704596343));
#10640=CARTESIAN_POINT('Ctrl Pts',(-0.108112179851629,0.111838778789471,
0.316508822519532));
#10641=CARTESIAN_POINT('Ctrl Pts',(-0.108869604911422,0.111100971770551,
0.316583928744778));
#10642=CARTESIAN_POINT('Ctrl Pts',(-0.109199763457013,0.110776479698431,
0.316616874810544));
#10643=CARTESIAN_POINT('Ctrl Pts',(-0.109834725548014,0.1101468183604,0.316680642564838));
#10644=CARTESIAN_POINT('Ctrl Pts',(-0.110139718372898,0.109841845218271,
0.316711455435337));
#10645=CARTESIAN_POINT('Ctrl Pts',(-0.110949479491181,0.109025372840118,
0.316793757617018));
#10646=CARTESIAN_POINT('Ctrl Pts',(-0.111451972970211,0.108511642744849,
0.316845345886176));
#10647=CARTESIAN_POINT('Ctrl Pts',(-0.113402359182437,0.106489803286914,
0.317047631907775));
#10648=CARTESIAN_POINT('Ctrl Pts',(-0.114823286229012,0.104956111877036,
0.317199480043754));
#10649=CARTESIAN_POINT('Ctrl Pts',(-0.118328635821682,0.101016180364589,
0.317585822048543));
#10650=CARTESIAN_POINT('Ctrl Pts',(-0.120370815262059,0.0985738248010755,
0.317821949653995));
#10651=CARTESIAN_POINT('Ctrl Pts',(-0.126103629237698,0.0912736544734109,
0.318518332383104));
#10652=CARTESIAN_POINT('Ctrl Pts',(-0.129584964943485,0.0862596582650869,
0.318985314453582));
#10653=CARTESIAN_POINT('Ctrl Pts',(-0.138706886644305,0.0713185072492202,
0.320338306441304));
#10654=CARTESIAN_POINT('Ctrl Pts',(-0.143562443411091,0.0609573245357439,
0.321233351895657));
#10655=CARTESIAN_POINT('Ctrl Pts',(-0.147600249513271,0.0491040492620575,
0.322158377065807));
#10656=CARTESIAN_POINT('Ctrl Pts',(-0.147947841727943,0.048046619336895,
0.322240048576568));
#10657=CARTESIAN_POINT('Ctrl Pts',(-0.148409540769718,0.046589518786747,
0.322351341330326));
#10658=CARTESIAN_POINT('Ctrl Pts',(-0.148533430148211,0.0461930210253136,
0.322381499554538));
#10659=CARTESIAN_POINT('Ctrl Pts',(-0.148728143983151,0.0455609721252862,
0.322429368423441));
#10660=CARTESIAN_POINT('Ctrl Pts',(-0.148799999445464,0.0453257450133406,
0.322447138344701));
#10661=CARTESIAN_POINT('Ctrl Pts',(-0.148947533565676,0.0448386430564463,
0.322483840851225));
#10662=CARTESIAN_POINT('Ctrl Pts',(-0.149023131458458,0.0445867464390801,
0.322502768284357));
#10663=CARTESIAN_POINT('Ctrl Pts',(-0.149202137990535,0.0439847448979742,
0.322547879271261));
#10664=CARTESIAN_POINT('Ctrl Pts',(-0.14930495462334,0.0436344622627188,
0.322574028439805));
#10665=CARTESIAN_POINT('Ctrl Pts',(-0.149520379158446,0.042890862529187,
0.322629335570863));
#10666=CARTESIAN_POINT('Ctrl Pts',(-0.149632670740083,0.0424974555624741,
0.322658475653757));
#10667=CARTESIAN_POINT('Ctrl Pts',(-0.149937403644339,0.0414136589348379,
0.322738434101334));
#10668=CARTESIAN_POINT('Ctrl Pts',(-0.150126630744275,0.0407223642402907,
0.322789079273793));
#10669=CARTESIAN_POINT('Ctrl Pts',(-0.153777084537168,0.0270149747521514,
0.323786727562734));
#10670=CARTESIAN_POINT('Ctrl Pts',(-0.155538566952624,0.0136034147113705,
0.324649336154599));
#10671=CARTESIAN_POINT('Ctrl Pts',(-0.155549944528231,0.000131366907260993,
0.325541276351331));
#10672=CARTESIAN_POINT('Ctrl Pts',(-0.155549941519498,0.000134882470554111,
0.325594377439629));
#10673=CARTESIAN_POINT('Ctrl Pts',(-0.15555880784338,-0.0100899907526335,
0.326325391658143));
#10674=CARTESIAN_POINT('Ctrl Pts',(-0.154555154411991,-0.0203335588299377,
0.327056405876658));
#10675=CARTESIAN_POINT('Ctrl Pts',(-0.152554318723264,-0.0303806243991271,
0.327787420095172));
#10676=CARTESIAN_POINT('Ctrl Pts',(-0.150554603080401,-0.0404220657312509,
0.328518025099948));
#10677=CARTESIAN_POINT('Ctrl Pts',(-0.147559001477363,-0.0502663007971989,
0.329248630104723));
#10678=CARTESIAN_POINT('Ctrl Pts',(-0.143633978489968,-0.0597083136853105,
0.329979235109499));
#10679=CARTESIAN_POINT('Ctrl Pts',(-0.139699463917864,-0.0691731594754049,
0.330711606880817));
#10680=CARTESIAN_POINT('Ctrl Pts',(-0.134831446328035,-0.0782329877699992,
0.331443978652135));
#10681=CARTESIAN_POINT('Ctrl Pts',(-0.129143803565775,-0.0867045587069356,
0.332176350423453));
#10682=CARTESIAN_POINT('Ctrl Pts',(-0.125869021867529,-0.091582246462531,
0.332598029100064));
#10683=CARTESIAN_POINT('Ctrl Pts',(-0.122323365373555,-0.0962654239148562,
0.333019707776675));
#10684=CARTESIAN_POINT('Ctrl Pts',(-0.118534587709285,-0.100724148130375,
0.333441386453285));
#10685=CARTESIAN_POINT('Ctrl Pts',(-0.111909869255113,-0.108520275327589,
0.334178696150029));
#10686=CARTESIAN_POINT('Ctrl Pts',(-0.104487883553983,-0.11568924989458,
0.334916005846774));
#10687=CARTESIAN_POINT('Ctrl Pts',(-0.0964115024798472,-0.122068114958733,
0.335653315543518));
#10688=CARTESIAN_POINT('Ctrl Pts',(-0.0882848547000145,-0.128486681533985,
0.336395214192813));
#10689=CARTESIAN_POINT('Ctrl Pts',(-0.0794962614522086,-0.134104547200687,
0.337137112842109));
#10690=CARTESIAN_POINT('Ctrl Pts',(-0.0702284668008892,-0.138793965829918,
0.337879011491404));
#10691=CARTESIAN_POINT('Ctrl Pts',(-0.0610391862679532,-0.143443657039276,
0.33861462498651));
#10692=CARTESIAN_POINT('Ctrl Pts',(-0.0513796418104073,-0.147180168478902,
0.339350238481616));
#10693=CARTESIAN_POINT('Ctrl Pts',(-0.0414531982586966,-0.149924763978888,
0.340085851976721));
#10694=CARTESIAN_POINT('Ctrl Pts',(-0.0313995359392024,-0.152704534620479,
0.340830893203111));
#10695=CARTESIAN_POINT('Ctrl Pts',(-0.0210730073372121,-0.154466474556329,
0.341575934429501));
#10696=CARTESIAN_POINT('Ctrl Pts',(-0.0106975876470872,-0.155181713222057,
0.342320975655891));
#10697=CARTESIAN_POINT('Ctrl Pts',(-0.000322167956962707,-0.155896951887786,
0.343066016882281));
#10698=CARTESIAN_POINT('Ctrl Pts',(0.0101011639815613,-0.15556555558113,
0.343811058108671));
#10699=CARTESIAN_POINT('Ctrl Pts',(0.0203502550655604,-0.154213065655173,
0.344556099335061));
#10700=CARTESIAN_POINT('Ctrl Pts',(0.0304929880736154,-0.152874610947079,
0.345293409031827));
#10701=CARTESIAN_POINT('Ctrl Pts',(0.0405411244634621,-0.150526202297159,
0.346030718728593));
#10702=CARTESIAN_POINT('Ctrl Pts',(0.0502802718650486,-0.14719951345428,
0.346768028425358));
#10703=CARTESIAN_POINT('Ctrl Pts',(0.0600800348875177,-0.143852119584423,
0.347509927074648));
#10704=CARTESIAN_POINT('Ctrl Pts',(0.0695660042342812,-0.139514358471281,
0.348251825723938));
#10705=CARTESIAN_POINT('Ctrl Pts',(0.0785317499687253,-0.134270498423331,
0.348993724373228));
#10706=CARTESIAN_POINT('Ctrl Pts',(0.0874215404575554,-0.129071062864954,
0.349729337868355));
#10707=CARTESIAN_POINT('Ctrl Pts',(0.0957990883436117,-0.122981316705354,
0.350464951363482));
#10708=CARTESIAN_POINT('Ctrl Pts',(0.103487959801753,-0.116129430705876,
0.351200564858609));
#10709=CARTESIAN_POINT('Ctrl Pts',(0.111275372972575,-0.109189729923024,
0.35194560608498));
#10710=CARTESIAN_POINT('Ctrl Pts',(0.118355571950899,-0.101468822740119,
0.352690647311352));
#10711=CARTESIAN_POINT('Ctrl Pts',(0.124582843579175,-0.0931392376269359,
0.353435688537723));
#10712=CARTESIAN_POINT('Ctrl Pts',(0.130810115207451,-0.0848096525137527,
0.354180729764095));
#10713=CARTESIAN_POINT('Ctrl Pts',(0.136183984389138,-0.075872247844273,
0.354925770990466));
#10714=CARTESIAN_POINT('Ctrl Pts',(0.140605443003462,-0.0665275273687531,
0.355670812216837));
#10715=CARTESIAN_POINT('Ctrl Pts',(0.144981018736611,-0.057279780027348,
0.35640812191363));
#10716=CARTESIAN_POINT('Ctrl Pts',(0.14845673252472,-0.0475638404553147,
0.357145431610422));
#10717=CARTESIAN_POINT('Ctrl Pts',(0.150942937142596,-0.0375770172680896,
0.357882741307214));
#10718=CARTESIAN_POINT('Ctrl Pts',(0.15344461568537,-0.0275280369475157,
0.358624639956497));
#10719=CARTESIAN_POINT('Ctrl Pts',(0.154944024042579,-0.0172056554152167,
0.359366538605781));
#10720=CARTESIAN_POINT('Ctrl Pts',(0.155400022831297,-0.00682901193674878,
0.360108437255064));
#10721=CARTESIAN_POINT('Ctrl Pts',(0.155852158528107,0.0034597235725403,
0.360844050750219));
#10722=CARTESIAN_POINT('Ctrl Pts',(0.155278477933672,0.0138008650692228,
0.361579664245374));
#10723=CARTESIAN_POINT('Ctrl Pts',(0.153690994693365,0.0239766688713038,
0.362315277740529));
#10724=CARTESIAN_POINT('Ctrl Pts',(0.152083166033404,0.0342828872777153,
0.363060318966876));
#10725=CARTESIAN_POINT('Ctrl Pts',(0.14943546241944,0.0444185318484303,
0.363805360193224));
#10726=CARTESIAN_POINT('Ctrl Pts',(0.14581382593986,0.0541676163845165,
0.364550401419571));
#10727=CARTESIAN_POINT('Ctrl Pts',(0.14219218946028,0.0639167009206027,
0.365295442645918));
#10728=CARTESIAN_POINT('Ctrl Pts',(0.137597083689187,0.0732783607708785,
0.366040483872266));
#10729=CARTESIAN_POINT('Ctrl Pts',(0.132143282539398,0.0820606810824336,
0.366785525098613));
#10730=CARTESIAN_POINT('Ctrl Pts',(0.126746077217331,0.090751864465138,
0.367522834795384));
#10731=CARTESIAN_POINT('Ctrl Pts',(0.120467523852922,0.0989408714713713,
0.368260144492155));
#10732=CARTESIAN_POINT('Ctrl Pts',(0.113424787979095,0.10644538492531,0.368997454188926));
#10733=CARTESIAN_POINT('Ctrl Pts',(0.106338218719297,0.113996605829399,
0.369739352838215));
#10734=CARTESIAN_POINT('Ctrl Pts',(0.0984784316869404,0.120853976588515,
0.370481251487504));
#10735=CARTESIAN_POINT('Ctrl Pts',(0.0900072391288423,0.126864098169669,
0.371223150136792));
#10736=CARTESIAN_POINT('Ctrl Pts',(0.0816078121025456,0.132823303711729,
0.371958763631925));
#10737=CARTESIAN_POINT('Ctrl Pts',(0.0726080793179316,0.137949035530561,
0.372694377127058));
#10738=CARTESIAN_POINT('Ctrl Pts',(0.0631975039910557,0.142133310625274,
0.373429990622192));
#10739=CARTESIAN_POINT('Ctrl Pts',(0.0536663213404706,0.146371212007785,
0.374175031848558));
#10740=CARTESIAN_POINT('Ctrl Pts',(0.0437145572080062,0.149642911252742,
0.374920073074924));
#10741=CARTESIAN_POINT('Ctrl Pts',(0.0335594421983349,0.151886689144693,
0.375665114301291));
#10742=CARTESIAN_POINT('Ctrl Pts',(0.0234043271886633,0.154130467036644,
0.376410155527657));
#10743=CARTESIAN_POINT('Ctrl Pts',(0.0130468391673053,0.15534624419272,
0.377155196754023));
#10744=CARTESIAN_POINT('Ctrl Pts',(0.00271046422415448,0.155526383239917,
0.37790023798039));
#10745=CARTESIAN_POINT('Ctrl Pts',(-0.00751912685898194,0.155704661292045,
0.37863758227447));
#10746=CARTESIAN_POINT('Ctrl Pts',(-0.0178047266851457,0.154870016604413,
0.37937492656855));
#10747=CARTESIAN_POINT('Ctrl Pts',(-0.0279295856847137,0.153022026987883,
0.380112270862631));
#10748=CARTESIAN_POINT('Ctrl Pts',(-0.0380325437573131,0.151178034729303,
0.380848020218595));
#10749=CARTESIAN_POINT('Ctrl Pts',(-0.0479745335382852,0.148325135029611,
0.38158376957456));
#10750=CARTESIAN_POINT('Ctrl Pts',(-0.0575442136137484,0.144514587428312,
0.382319518930524));
#10751=CARTESIAN_POINT('Ctrl Pts',(-0.0596103411904147,0.143691876802757,
0.382478369803478));
#10752=CARTESIAN_POINT('Ctrl Pts',(-0.0616591580438317,0.142824714283798,
0.382637220676431));
#10753=CARTESIAN_POINT('Ctrl Pts',(-0.0636886258329921,0.141913922641526,
0.382796071549385));
#10754=CARTESIAN_POINT('Origin',(0.,0.,-0.129405622560373));
#10755=CARTESIAN_POINT('',(-0.0637865765496296,0.142129738084048,0.466608809190139));
#10756=CARTESIAN_POINT('',(-0.0636704081198525,0.141871577573868,0.452783997775559));
#10757=CARTESIAN_POINT('',(-0.0636886258329924,0.141913922641526,-0.129405622560373));
#10758=CARTESIAN_POINT('',(-0.155747148273957,-8.48283479504535E-5,0.40940562256037));
#10759=CARTESIAN_POINT('Ctrl Pts',(-0.155747148273957,-8.48283479504535E-5,
0.40940562256037));
#10760=CARTESIAN_POINT('Ctrl Pts',(-0.155779482799656,-0.00500404714443213,
0.409759213094268));
#10761=CARTESIAN_POINT('Ctrl Pts',(-0.153336323268121,-0.0614340654297066,
0.413817707922091));
#10762=CARTESIAN_POINT('Ctrl Pts',(-0.0845632241029054,-0.163255983359439,
0.42158110704384));
#10763=CARTESIAN_POINT('Ctrl Pts',(0.0913113927969153,-0.159579712115361,
0.432695819925616));
#10764=CARTESIAN_POINT('Ctrl Pts',(0.183594933073833,-0.00981608490943425,
0.443810532807392));
#10765=CARTESIAN_POINT('Ctrl Pts',(0.107806367033371,0.148933683901261,
0.454925245689169));
#10766=CARTESIAN_POINT('Ctrl Pts',(-0.0114902447342972,0.16425485410465,
0.462524671150084));
#10767=CARTESIAN_POINT('Ctrl Pts',(-0.0613862033991981,0.143219630774059,
0.466419192317074));
#10768=CARTESIAN_POINT('Ctrl Pts',(-0.0637865765496296,0.142129738084048,
0.466608809190139));
#10769=CARTESIAN_POINT('Ctrl Pts',(-0.15554997258092,-9.23584055120413E-5,
0.409292448061377));
#10770=CARTESIAN_POINT('Ctrl Pts',(-0.155557537435976,0.0126483660585973,
0.408427759124959));
#10771=CARTESIAN_POINT('Ctrl Pts',(-0.153999806552126,0.0253430736269646,
0.407612305561652));
#10772=CARTESIAN_POINT('Ctrl Pts',(-0.149882798880593,0.0418201330599853,
0.406475148577664));
#10773=CARTESIAN_POINT('Ctrl Pts',(-0.148687414650298,0.0458892688006899,
0.406188013833792));
#10774=CARTESIAN_POINT('Ctrl Pts',(-0.14649406783911,0.0523644696222185,
0.405716850546238));
#10775=CARTESIAN_POINT('Ctrl Pts',(-0.145599273192537,0.0548032833110541,
0.405536046470926));
#10776=CARTESIAN_POINT('Ctrl Pts',(-0.144351432928983,0.0579577294100021,
0.405297249788426));
#10777=CARTESIAN_POINT('Ctrl Pts',(-0.144053322372908,0.0586947600576042,
0.40524109849527));
#10778=CARTESIAN_POINT('Ctrl Pts',(-0.143557846676748,0.059893230008936,
0.405149192967831));
#10779=CARTESIAN_POINT('Ctrl Pts',(-0.143363872462857,0.0603560635318725,
0.405113553465428));
#10780=CARTESIAN_POINT('Ctrl Pts',(-0.142985521260094,0.0612467160773643,
0.405044683000883));
#10781=CARTESIAN_POINT('Ctrl Pts',(-0.142801455094546,0.0616746620135198,
0.405011462892062));
#10782=CARTESIAN_POINT('Ctrl Pts',(-0.142374158583935,0.062655939886744,
0.404934989247679));
#10783=CARTESIAN_POINT('Ctrl Pts',(-0.142129621211477,0.0632086907851109,
0.40489169152825));
#10784=CARTESIAN_POINT('Ctrl Pts',(-0.141468225648485,0.0646804606617182,
0.404775807944452));
#10785=CARTESIAN_POINT('Ctrl Pts',(-0.141045641411174,0.0655968582265392,
0.404703026930829));
#10786=CARTESIAN_POINT('Ctrl Pts',(-0.137591525234734,0.0728995883620714,
0.404117909179039));
#10787=CARTESIAN_POINT('Ctrl Pts',(-0.134137241223736,0.0790755959048336,
0.403590896643744));
#10788=CARTESIAN_POINT('Ctrl Pts',(-0.124704628610565,0.0935334474189555,
0.402275888788921));
#10789=CARTESIAN_POINT('Ctrl Pts',(-0.118307773153663,0.101503675713296,
0.401477575043163));
#10790=CARTESIAN_POINT('Ctrl Pts',(-0.108533763554301,0.111492238453883,
0.400403532777939));
#10791=CARTESIAN_POINT('Ctrl Pts',(-0.105791642054227,0.114097458434855,
0.400115603687116));
#10792=CARTESIAN_POINT('Ctrl Pts',(-0.101967647376471,0.117474012903218,
0.399734386913506));
#10793=CARTESIAN_POINT('Ctrl Pts',(-0.100967075944991,0.118335094879871,
0.399636417229969));
#10794=CARTESIAN_POINT('Ctrl Pts',(-0.0994718924935058,0.119589061732261,
0.399492765935777));
#10795=CARTESIAN_POINT('Ctrl Pts',(-0.0989856845943892,0.119991813732151,
0.399446473643626));
#10796=CARTESIAN_POINT('Ctrl Pts',(-0.0981049607053237,0.120712368013654,
0.399363393766964));
#10797=CARTESIAN_POINT('Ctrl Pts',(-0.0977113220410934,0.121031221883824,
0.399326536594244));
#10798=CARTESIAN_POINT('Ctrl Pts',(-0.0970869351904872,0.121531953930878,
0.399268516574676));
#10799=CARTESIAN_POINT('Ctrl Pts',(-0.0968572221164068,0.121715107274073,
0.399247264743596));
#10800=CARTESIAN_POINT('Ctrl Pts',(-0.0966263276692074,0.121898134940101,
0.399225998682503));
#10801=CARTESIAN_POINT('Ctrl Pts',(-0.0966256664104302,0.121898659104406,
0.399225937779395));
#10802=CARTESIAN_POINT('Ctrl Pts',(-0.0966243412313925,0.121899709525155,
0.399225815729616));
#10803=CARTESIAN_POINT('Ctrl Pts',(-0.096623677311036,0.121900235781603,
0.399225754582941));
#10804=CARTESIAN_POINT('Ctrl Pts',(-0.0966223467903276,0.1219012904011,
0.399225632044343));
#10805=CARTESIAN_POINT('Ctrl Pts',(-0.0966216801867385,0.121901818766642,
0.399225570652127));
#10806=CARTESIAN_POINT('Ctrl Pts',(-0.0966203442745582,0.121902877623932,
0.399225447620162));
#10807=CARTESIAN_POINT('Ctrl Pts',(-0.096619674968368,0.121903408113704,
0.39922538598064));
#10808=CARTESIAN_POINT('Ctrl Pts',(-0.0966183336272404,0.121904471238058,
0.399225262451894));
#10809=CARTESIAN_POINT('Ctrl Pts',(-0.0966176615937382,0.121905003871429,
0.39922520056281));
#10810=CARTESIAN_POINT('Ctrl Pts',(-0.0966163147788525,0.121906071297926,
0.399225076533197));
#10811=CARTESIAN_POINT('Ctrl Pts',(-0.0966156399939986,0.121906606093728,
0.399225014392356));
#10812=CARTESIAN_POINT('Ctrl Pts',(-0.0966142876526094,0.121907677863727,
0.399224889857058));
#10813=CARTESIAN_POINT('Ctrl Pts',(-0.0966136100963429,0.121908214837636,
0.399224827462632));
#10814=CARTESIAN_POINT('Ctrl Pts',(-0.0966122521868786,0.121909290983635,
0.399224702417861));
#10815=CARTESIAN_POINT('Ctrl Pts',(-0.0966115718352112,0.121909830154436,
0.399224639767663));
#10816=CARTESIAN_POINT('Ctrl Pts',(-0.0966101471332454,0.121910959194794,
0.39922450857568));
#10817=CARTESIAN_POINT('Ctrl Pts',(-0.09660940278153,0.121911549063647,
0.399224440033928));
#10818=CARTESIAN_POINT('Ctrl Pts',(-0.0966079004402631,0.121912739586392,
0.399224301696613));
#10819=CARTESIAN_POINT('Ctrl Pts',(-0.0966071424489415,0.121913340241277,
0.399224231900924));
#10820=CARTESIAN_POINT('Ctrl Pts',(-0.0966056125263574,0.121914552574241,
0.399224091028028));
#10821=CARTESIAN_POINT('Ctrl Pts',(-0.0966048405972114,0.121915164250217,
0.399224019951054));
#10822=CARTESIAN_POINT('Ctrl Pts',(-0.0966032824931897,0.121916398866383,
0.399223876487547));
#10823=CARTESIAN_POINT('Ctrl Pts',(-0.0966024963151156,0.121917021808664,
0.399223804100759));
#10824=CARTESIAN_POINT('Ctrl Pts',(-0.096600909394848,0.121918279208378,
0.399223657988428));
#10825=CARTESIAN_POINT('Ctrl Pts',(-0.096600108654989,0.1219189136635,0.399223584263141));
#10826=CARTESIAN_POINT('Ctrl Pts',(-0.0965984922879632,0.121920194343575,
0.39922343544418));
#10827=CARTESIAN_POINT('Ctrl Pts',(-0.0965976766573522,0.121920840570776,
0.399223360350232));
#10828=CARTESIAN_POINT('Ctrl Pts',(-0.0965960301729118,0.121922145059696,
0.399223208763152));
#10829=CARTESIAN_POINT('Ctrl Pts',(-0.0965951993210838,0.121922803319329,
0.399223132270249));
#10830=CARTESIAN_POINT('Ctrl Pts',(-0.0965935220492247,0.12192413214492,
0.399222977853633));
#10831=CARTESIAN_POINT('Ctrl Pts',(-0.0965926756306571,0.121924802709198,
0.399222899930101));
#10832=CARTESIAN_POINT('Ctrl Pts',(-0.0965909668741902,0.121926156420677,
0.399222742620042));
#10833=CARTESIAN_POINT('Ctrl Pts',(-0.0965901045349775,0.121926839568376,
0.399222663233442));
#10834=CARTESIAN_POINT('Ctrl Pts',(-0.0965883635749518,0.121928218732045,
0.399222502964044));
#10835=CARTESIAN_POINT('Ctrl Pts',(-0.0965874849529363,0.121928914748401,
0.399222422081185));
#10836=CARTESIAN_POINT('Ctrl Pts',(-0.0965857110534585,0.12193031994382,
0.399222258785007));
#10837=CARTESIAN_POINT('Ctrl Pts',(-0.0965848157753737,0.121931029122786,
0.399222176371682));
#10838=CARTESIAN_POINT('Ctrl Pts',(-0.0963904279118336,0.122085006604115,
0.399204282632976));
#10839=CARTESIAN_POINT('Ctrl Pts',(-0.096196573136442,0.122237812270272,
0.399186505003034));
#10840=CARTESIAN_POINT('Ctrl Pts',(-0.0957419364928956,0.122594427433828,
0.39914496751221));
#10841=CARTESIAN_POINT('Ctrl Pts',(-0.095480867346312,0.122797866502447,
0.399121234049922));
#10842=CARTESIAN_POINT('Ctrl Pts',(-0.0946772604466527,0.123419967880696,
0.399048536354677));
#10843=CARTESIAN_POINT('Ctrl Pts',(-0.0941325936993364,0.123835887234364,
0.398999760930253));
#10844=CARTESIAN_POINT('Ctrl Pts',(-0.0863119302969718,0.129726501274908,
0.398306195051271));
#10845=CARTESIAN_POINT('Ctrl Pts',(-0.078570331258783,0.13455659010774,
0.397702516207297));
#10846=CARTESIAN_POINT('Ctrl Pts',(-0.0682213415125348,0.139813789530708,
0.396937441118992));
#10847=CARTESIAN_POINT('Ctrl Pts',(-0.0659671172503672,0.140891373402896,
0.396773196082423));
#10848=CARTESIAN_POINT('Ctrl Pts',(-0.0636886207929056,0.141913924903434,
0.396608754846595));
#10849=CARTESIAN_POINT('',(-0.155542147809967,-7.47474344319557E-5,0.395594379955244));
#10850=CARTESIAN_POINT('Ctrl Pts',(-0.0636886258329921,0.141913922641526,
0.382796071549385));
#10851=CARTESIAN_POINT('Ctrl Pts',(-0.0730861195942185,0.137696482570911,
0.383531633895099));
#10852=CARTESIAN_POINT('Ctrl Pts',(-0.082066691787089,0.132539942042728,
0.384267196240812));
#10853=CARTESIAN_POINT('Ctrl Pts',(-0.0904421818323631,0.126554392438199,
0.385002758586526));
#10854=CARTESIAN_POINT('Ctrl Pts',(-0.0988383308873284,0.120554078858474,
0.385740135272601));
#10855=CARTESIAN_POINT('Ctrl Pts',(-0.106625672314012,0.113721234620129,
0.386477511958675));
#10856=CARTESIAN_POINT('Ctrl Pts',(-0.113647151506982,0.106207944403181,
0.38721488864475));
#10857=CARTESIAN_POINT('Ctrl Pts',(-0.119360694143706,0.100094203577801,
0.387814909383888));
#10858=CARTESIAN_POINT('Ctrl Pts',(-0.124567633470123,0.0935308734025379,
0.388414930123027));
#10859=CARTESIAN_POINT('Ctrl Pts',(-0.129203650408045,0.0866153521105563,
0.389014950862166));
#10860=CARTESIAN_POINT('Ctrl Pts',(-0.134996062412211,0.0779748425776694,
0.3897646390921));
#10861=CARTESIAN_POINT('Ctrl Pts',(-0.13993845508717,0.0687205532039445,
0.390514327322034));
#10862=CARTESIAN_POINT('Ctrl Pts',(-0.143909921737381,0.0590401297893296,
0.391264015551968));
#10863=CARTESIAN_POINT('Ctrl Pts',(-0.147872374669165,0.0493816772531327,
0.392012002274825));
#10864=CARTESIAN_POINT('Ctrl Pts',(-0.150867858811146,0.0392997867614514,
0.392759988997682));
#10865=CARTESIAN_POINT('Ctrl Pts',(-0.152821662629263,0.029005894766889,
0.393507975720539));
#10866=CARTESIAN_POINT('Ctrl Pts',(-0.1546382811691,0.0194347828307725,
0.394203442960236));
#10867=CARTESIAN_POINT('Ctrl Pts',(-0.155554668148968,0.00968118809725694,
0.394898910199932));
#10868=CARTESIAN_POINT('Ctrl Pts',(-0.15554998205569,-7.47159587813949E-5,
0.395594377439629));
#10869=CARTESIAN_POINT('Ctrl Pts',(-0.155329803440314,-7.56005704470291E-5,
0.395594448140074));
#10870=CARTESIAN_POINT('Ctrl Pts',(-0.155421485368252,-0.021252058778351,
0.397106186674697));
#10871=CARTESIAN_POINT('Ctrl Pts',(-0.141514608041042,-0.0942113101233241,
0.402322829503245));
#10872=CARTESIAN_POINT('Ctrl Pts',(-0.030390408656302,-0.18132809188354,
0.411244376625719));
#10873=CARTESIAN_POINT('Ctrl Pts',(0.135872146613563,-0.123863689671489,
0.422359089507495));
#10874=CARTESIAN_POINT('Ctrl Pts',(0.177750452880091,0.0469918114711103,
0.433473802389271));
#10875=CARTESIAN_POINT('Ctrl Pts',(0.0674866542632175,0.163636701374273,
0.443615438478625));
#10876=CARTESIAN_POINT('Ctrl Pts',(-0.0287035209048353,0.157155007295605,
0.450052170274054));
#10877=CARTESIAN_POINT('Ctrl Pts',(-0.0636704081198332,0.141871577573876,
0.452783997775557));
#10878=CARTESIAN_POINT('Origin',(0.,0.,-0.129405622560373));
#10879=CARTESIAN_POINT('',(-0.0636886258329926,0.141913922641526,0.536610014060325));
#10880=CARTESIAN_POINT('',(-0.0636886260274623,0.141913922554251,0.522938154987668));
#10881=CARTESIAN_POINT('',(-0.0636886258329924,0.141913922641526,-0.129405622560373));
#10882=CARTESIAN_POINT('',(-0.155549938719811,0.000138073397279943,0.479405624672607));
#10883=CARTESIAN_POINT('Ctrl Pts',(-0.155549938719811,0.000138073397279943,
0.479405624672607));
#10884=CARTESIAN_POINT('Ctrl Pts',(-0.1555590802874,-0.0101605815668361,
0.480144271311098));
#10885=CARTESIAN_POINT('Ctrl Pts',(-0.154540807560027,-0.0204920682189847,
0.480882917949589));
#10886=CARTESIAN_POINT('Ctrl Pts',(-0.152503881605263,-0.0306328026032212,
0.48162156458808));
#10887=CARTESIAN_POINT('Ctrl Pts',(-0.150503926990696,-0.0405894770122334,
0.482346804378819));
#10888=CARTESIAN_POINT('Ctrl Pts',(-0.147522245248312,-0.050361310081166,
0.483072044169558));
#10889=CARTESIAN_POINT('Ctrl Pts',(-0.143619085953899,-0.0597441264876015,
0.483797283960298));
#10890=CARTESIAN_POINT('Ctrl Pts',(-0.139607695430838,-0.0693871202711947,
0.484542634022664));
#10891=CARTESIAN_POINT('Ctrl Pts',(-0.134623217858585,-0.0786181617347638,
0.485287984085031));
#10892=CARTESIAN_POINT('Ctrl Pts',(-0.128783351950023,-0.0872390437849736,
0.486033334147398));
#10893=CARTESIAN_POINT('Ctrl Pts',(-0.12294348604146,-0.0958599258351837,
0.486778684209764));
#10894=CARTESIAN_POINT('Ctrl Pts',(-0.11624896051622,-0.103869838725253,
0.487524034272131));
#10895=CARTESIAN_POINT('Ctrl Pts',(-0.108861606859135,-0.111107844241741,
0.488269384334498));
#10896=CARTESIAN_POINT('Ctrl Pts',(-0.101553943306264,-0.118267770727406,
0.489006694031275));
#10897=CARTESIAN_POINT('Ctrl Pts',(-0.093509487166098,-0.124730494109114,
0.489744003728051));
#10898=CARTESIAN_POINT('Ctrl Pts',(-0.0848853671140475,-0.130346756576117,
0.490481313424828));
#10899=CARTESIAN_POINT('Ctrl Pts',(-0.0762075712761837,-0.135997974180504,
0.491223212074115));
#10900=CARTESIAN_POINT('Ctrl Pts',(-0.0669435581198422,-0.140791495449943,
0.491965110723402));
#10901=CARTESIAN_POINT('Ctrl Pts',(-0.0572869535805678,-0.144616760610442,
0.492707009372689));
#10902=CARTESIAN_POINT('Ctrl Pts',(-0.0477121570458454,-0.148409619213502,
0.493442622867828));
#10903=CARTESIAN_POINT('Ctrl Pts',(-0.0377522780015032,-0.151250239972536,
0.494178236362967));
#10904=CARTESIAN_POINT('Ctrl Pts',(-0.0276170107185682,-0.153078748423713,
0.494913849858106));
#10905=CARTESIAN_POINT('Ctrl Pts',(-0.0173518483529004,-0.154930691309317,
0.495658891084467));
#10906=CARTESIAN_POINT('Ctrl Pts',(-0.00690771718440615,-0.155744171137756,
0.496403932310828));
#10907=CARTESIAN_POINT('Ctrl Pts',(0.00348970852022084,-0.155510849893002,
0.49714897353719));
#10908=CARTESIAN_POINT('Ctrl Pts',(0.0138871342248475,-0.155277528648248,
0.497894014763551));
#10909=CARTESIAN_POINT('Ctrl Pts',(0.0242368857416045,-0.153997561560528,
0.498639055989912));
#10910=CARTESIAN_POINT('Ctrl Pts',(0.0343200622446376,-0.151716630029553,
0.499384097216273));
#10911=CARTESIAN_POINT('Ctrl Pts',(0.0442986024206074,-0.149459368449967,
0.50012140691305));
#10912=CARTESIAN_POINT('Ctrl Pts',(0.0540908956050945,-0.146204977218319,
0.500858716609827));
#10913=CARTESIAN_POINT('Ctrl Pts',(0.0634863282952233,-0.142004537320436,
0.501596026306604));
#10914=CARTESIAN_POINT('Ctrl Pts',(0.0729402373550734,-0.137777954243781,
0.502337924955891));
#10915=CARTESIAN_POINT('Ctrl Pts',(0.0819913996524141,-0.132593723636582,
0.503079823605178));
#10916=CARTESIAN_POINT('Ctrl Pts',(0.090441924285109,-0.126554576494122,
0.503821722254466));
#10917=CARTESIAN_POINT('Ctrl Pts',(0.0988208584788675,-0.120566591286989,
0.504557335749605));
#10918=CARTESIAN_POINT('Ctrl Pts',(0.106608541702961,-0.113738684808734,
0.505292949244743));
#10919=CARTESIAN_POINT('Ctrl Pts',(0.113640955466632,-0.106214574050038,
0.506028562739883));
#10920=CARTESIAN_POINT('Ctrl Pts',(0.120763497683961,-0.0985940331763595,
0.506773603966244));
#10921=CARTESIAN_POINT('Ctrl Pts',(0.127110572156788,-0.0902599902839601,
0.507518645192605));
#10922=CARTESIAN_POINT('Ctrl Pts',(0.132552795837115,-0.081397535686065,
0.508263686418966));
#10923=CARTESIAN_POINT('Ctrl Pts',(0.137995019517441,-0.0725350810881702,
0.509008727645328));
#10924=CARTESIAN_POINT('Ctrl Pts',(0.142531997515425,-0.0631451128853464,
0.509753768871688));
#10925=CARTESIAN_POINT('Ctrl Pts',(0.146083407030714,-0.0534363236974505,
0.51049881009805));
#10926=CARTESIAN_POINT('Ctrl Pts',(0.149597962440805,-0.043828285700466,
0.511236119794826));
#10927=CARTESIAN_POINT('Ctrl Pts',(0.152173731215626,-0.0338360145212888,
0.511973429491603));
#10928=CARTESIAN_POINT('Ctrl Pts',(0.153739421299251,-0.0236641678191169,
0.51271073918838));
#10929=CARTESIAN_POINT('Ctrl Pts',(0.155314856104085,-0.0134290124127974,
0.513452637837667));
#10930=CARTESIAN_POINT('Ctrl Pts',(0.155867274863009,-0.00301293736332606,
0.514194536486954));
#10931=CARTESIAN_POINT('Ctrl Pts',(0.15537568106821,0.00736208072422352,
0.514936435136241));
#10932=CARTESIAN_POINT('Ctrl Pts',(0.15488825191609,0.0176492046121652,
0.51567204863138));
#10933=CARTESIAN_POINT('Ctrl Pts',(0.15337449941722,0.0278950266995725,
0.516407662126519));
#10934=CARTESIAN_POINT('Ctrl Pts',(0.150866231699999,0.0378838043580931,
0.517143275621658));
#10935=CARTESIAN_POINT('Ctrl Pts',(0.14832581765318,0.0480005996666759,
0.51788831684802));
#10936=CARTESIAN_POINT('Ctrl Pts',(0.144765401788514,0.0578527600473534,
0.518633358074381));
#10937=CARTESIAN_POINT('Ctrl Pts',(0.14027033607596,0.0672312079107413,
0.519378399300742));
#10938=CARTESIAN_POINT('Ctrl Pts',(0.135775270363406,0.0766096557741292,
0.520123440527103));
#10939=CARTESIAN_POINT('Ctrl Pts',(0.130346095249456,0.0855135723160958,
0.520868481753464));
#10940=CARTESIAN_POINT('Ctrl Pts',(0.124114597521458,0.0937623014973852,
0.521613522979826));
#10941=CARTESIAN_POINT('Ctrl Pts',(0.117947766025789,0.101925430994467,
0.522350832676602));
#10942=CARTESIAN_POINT('Ctrl Pts',(0.110949021114648,0.109508150675974,
0.523088142373379));
#10943=CARTESIAN_POINT('Ctrl Pts',(0.103251656540129,0.116339580202609,
0.523825452070156));
#10944=CARTESIAN_POINT('Ctrl Pts',(0.0955063842266478,0.123213527962508,
0.524567350719443));
#10945=CARTESIAN_POINT('Ctrl Pts',(0.0870543473186811,0.129326044467828,
0.525309249368731));
#10946=CARTESIAN_POINT('Ctrl Pts',(0.0780706649700945,0.134539116137751,
0.526051148018018));
#10947=CARTESIAN_POINT('Ctrl Pts',(0.0691630898208316,0.139708024148578,
0.526786761513157));
#10948=CARTESIAN_POINT('Ctrl Pts',(0.0597336673533617,0.143992217048598,
0.527522375008296));
#10949=CARTESIAN_POINT('Ctrl Pts',(0.0499809135424709,0.147301428307603,
0.528257988503435));
#10950=CARTESIAN_POINT('Ctrl Pts',(0.0401031669980127,0.150653050906958,
0.529003029729796));
#10951=CARTESIAN_POINT('Ctrl Pts',(0.0298946459200571,0.15300416185647,
0.529748070956157));
#10952=CARTESIAN_POINT('Ctrl Pts',(0.0195773017775878,0.154313096511959,
0.530493112182519));
#10953=CARTESIAN_POINT('Ctrl Pts',(0.0092599576351189,0.155622031167448,
0.53123815340888));
#10954=CARTESIAN_POINT('Ctrl Pts',(-0.00116522854114558,0.155888799596017,
0.531983194635241));
#10955=CARTESIAN_POINT('Ctrl Pts',(-0.0114750046802433,0.155126164032984,
0.532728235861602));
#10956=CARTESIAN_POINT('Ctrl Pts',(-0.0216784195161703,0.154371396236549,
0.53346559083419));
#10957=CARTESIAN_POINT('Ctrl Pts',(-0.031845294325765,0.152602787151973,
0.534202945806778));
#10958=CARTESIAN_POINT('Ctrl Pts',(-0.0417597337363428,0.149839671443412,
0.534940300779366));
#10959=CARTESIAN_POINT('Ctrl Pts',(-0.0492433618270808,0.147754013396778,
0.535496871873019));
#10960=CARTESIAN_POINT('Ctrl Pts',(-0.0565829658107906,0.145102825562585,
0.536053442966672));
#10961=CARTESIAN_POINT('Ctrl Pts',(-0.0636886258329926,0.141913922641526,
0.536610014060325));
#10962=CARTESIAN_POINT('Ctrl Pts',(-0.0637865765496296,0.142129738084048,
0.466608809190139));
#10963=CARTESIAN_POINT('Ctrl Pts',(-0.108286843876662,0.121924331247818,
0.470124096610999));
#10964=CARTESIAN_POINT('Ctrl Pts',(-0.150204862388095,0.0699946174511132,
0.474389701067743));
#10965=CARTESIAN_POINT('Ctrl Pts',(-0.155693983092541,0.0106028137662625,
0.478655305524487));
#10966=CARTESIAN_POINT('Ctrl Pts',(-0.155597581791774,0.000138145146615299,
0.47940562256037));
#10967=CARTESIAN_POINT('',(-0.155730189438309,-9.40385839890952E-5,0.465594279708133));
#10968=CARTESIAN_POINT('Ctrl Pts',(-0.0636704081198332,0.141871577573876,
0.452783997775557));
#10969=CARTESIAN_POINT('Ctrl Pts',(-0.0761256112515922,0.136427620822346,
0.453757074567979));
#10970=CARTESIAN_POINT('Ctrl Pts',(-0.127520786042802,0.105560469046302,
0.458027168545505));
#10971=CARTESIAN_POINT('Ctrl Pts',(-0.155398933057417,0.0457878287565685,
0.462297262523029));
#10972=CARTESIAN_POINT('Ctrl Pts',(-0.155730189438309,-9.40385839890952E-5,
0.465594279708133));
#10973=CARTESIAN_POINT('Ctrl Pts',(-0.155549975452665,-8.73880735471365E-5,
0.465697707969148));
#10974=CARTESIAN_POINT('Ctrl Pts',(-0.155548164875887,-0.00331019825709863,
0.465944108543144));
#10975=CARTESIAN_POINT('Ctrl Pts',(-0.155446195038996,-0.00653246011159423,
0.466188084566158));
#10976=CARTESIAN_POINT('Ctrl Pts',(-0.155155744776936,-0.0111573908270398,
0.466532880105807));
#10977=CARTESIAN_POINT('Ctrl Pts',(-0.155048174695573,-0.0125640916787875,
0.466637030835553));
#10978=CARTESIAN_POINT('Ctrl Pts',(-0.154883554325798,-0.0143897677691079,
0.466771103469191));
#10979=CARTESIAN_POINT('Ctrl Pts',(-0.154843918718361,-0.0148101878428167,
0.466801902094296));
#10980=CARTESIAN_POINT('Ctrl Pts',(-0.154774299441659,-0.0155177995442651,
0.466853605932392));
#10981=CARTESIAN_POINT('Ctrl Pts',(-0.154745227618446,-0.0158050752386271,
0.466874559530526));
#10982=CARTESIAN_POINT('Ctrl Pts',(-0.15469031679173,-0.0163330024566513,
0.4669129957944));
#10983=CARTESIAN_POINT('Ctrl Pts',(-0.154664715795774,-0.0165736769722737,
0.466930491496732));
#10984=CARTESIAN_POINT('Ctrl Pts',(-0.154610555425915,-0.0170717818417858,
0.466966644029411));
#10985=CARTESIAN_POINT('Ctrl Pts',(-0.154581915234115,-0.0173291969883696,
0.466985295485207));
#10986=CARTESIAN_POINT('Ctrl Pts',(-0.154514967182694,-0.017917544348447,
0.467027854072288));
#10987=CARTESIAN_POINT('Ctrl Pts',(-0.154476239093041,-0.0182484256919927,
0.467051737361886));
#10988=CARTESIAN_POINT('Ctrl Pts',(-0.15437061608041,-0.0191263998087611,
0.467114980254563));
#10989=CARTESIAN_POINT('Ctrl Pts',(-0.154301875072465,-0.0196732725305804,
0.467154238895342));
#10990=CARTESIAN_POINT('Ctrl Pts',(-0.153801795329305,-0.0234877262749171,
0.467427205988928));
#10991=CARTESIAN_POINT('Ctrl Pts',(-0.153269564534123,-0.026741545112331,
0.467655632166634));
#10992=CARTESIAN_POINT('Ctrl Pts',(-0.152246948752375,-0.0319485348496029,
0.468017626718562));
#10993=CARTESIAN_POINT('Ctrl Pts',(-0.151821408491984,-0.0339131660570124,
0.468153384709735));
#10994=CARTESIAN_POINT('Ctrl Pts',(-0.148682919453986,-0.0471567511957541,
0.469066254280379));
#10995=CARTESIAN_POINT('Ctrl Pts',(-0.144753683561463,-0.0581099049338928,
0.46981278092554));
#10996=CARTESIAN_POINT('Ctrl Pts',(-0.13786812908316,-0.0721416220458392,
0.470861248283143));
#10997=CARTESIAN_POINT('Ctrl Pts',(-0.135953539177746,-0.0756879497399387,
0.471134588221908));
#10998=CARTESIAN_POINT('Ctrl Pts',(-0.132629730486719,-0.0813106596315096,
0.471585145436031));
#10999=CARTESIAN_POINT('Ctrl Pts',(-0.131304118296203,-0.0834343817743867,
0.471759492773676));
#11000=CARTESIAN_POINT('Ctrl Pts',(-0.129496671811696,-0.0861802160342242,
0.471990942536704));
#11001=CARTESIAN_POINT('Ctrl Pts',(-0.129060496691806,-0.0868320551364464,
0.472046343993481));
#11002=CARTESIAN_POINT('Ctrl Pts',(-0.128338573174079,-0.0878934725014694,
0.472137323055854));
#11003=CARTESIAN_POINT('Ctrl Pts',(-0.128055744863998,-0.0883050285626444,
0.472172790276873));
#11004=CARTESIAN_POINT('Ctrl Pts',(-0.127504846408535,-0.0890984529819978,
0.472241540611045));
#11005=CARTESIAN_POINT('Ctrl Pts',(-0.127237029916742,-0.0894804916766432,
0.472274813813889));
#11006=CARTESIAN_POINT('Ctrl Pts',(-0.12661531116442,-0.0903589350395661,
0.472351716572051));
#11007=CARTESIAN_POINT('Ctrl Pts',(-0.126260203267138,-0.0908544727247875,
0.47239539201171));
#11008=CARTESIAN_POINT('Ctrl Pts',(-0.125298872028597,-0.0921794480044028,
0.472512972880781));
#11009=CARTESIAN_POINT('Ctrl Pts',(-0.124687338396307,-0.0930049757566399,
0.472587082654436));
#11010=CARTESIAN_POINT('Ctrl Pts',(-0.119292433485654,-0.10013887270268,
0.47323508061539));
#11011=CARTESIAN_POINT('Ctrl Pts',(-0.114042947506785,-0.106078486715775,
0.473827534466485));
#11012=CARTESIAN_POINT('Ctrl Pts',(-0.101551535814027,-0.118208685514831,
0.475159817809064));
#11013=CARTESIAN_POINT('Ctrl Pts',(-0.0941466666919652,-0.124186952003432,
0.475903099373365));
#11014=CARTESIAN_POINT('Ctrl Pts',(-0.0832040702968274,-0.131477070797758,
0.476912729319627));
#11015=CARTESIAN_POINT('Ctrl Pts',(-0.0800944336132139,-0.133394240125578,
0.477190543098319));
#11016=CARTESIAN_POINT('Ctrl Pts',(-0.0757991533018811,-0.135837968557607,
0.477559629399006));
#11017=CARTESIAN_POINT('Ctrl Pts',(-0.0746704080736929,-0.136461700741375,
0.477655295354975));
#11018=CARTESIAN_POINT('Ctrl Pts',(-0.0729869354279448,-0.137364825033823,
0.47779588855457));
#11019=CARTESIAN_POINT('Ctrl Pts',(-0.0724381147288619,-0.137655030666191,
0.477841398138763));
#11020=CARTESIAN_POINT('Ctrl Pts',(-0.0714412843417732,-0.13817452241102,
0.477923452672274));
#11021=CARTESIAN_POINT('Ctrl Pts',(-0.0709938748025159,-0.138404933117785,
0.477960062473078));
#11022=CARTESIAN_POINT('Ctrl Pts',(-0.0702858420787814,-0.138765225051959,
0.478017644218082));
#11023=CARTESIAN_POINT('Ctrl Pts',(-0.0700259643329782,-0.138896550005705,
0.478038704287792));
#11024=CARTESIAN_POINT('Ctrl Pts',(-0.0695350018513293,-0.139142921669729,
0.47807834795028));
#11025=CARTESIAN_POINT('Ctrl Pts',(-0.0693040021660714,-0.139258121553617,
0.478096940620944));
#11026=CARTESIAN_POINT('Ctrl Pts',(-0.0687764063239815,-0.139519596451617,
0.478139270607487));
#11027=CARTESIAN_POINT('Ctrl Pts',(-0.0684796301671491,-0.139665500817273,
0.478162984694788));
#11028=CARTESIAN_POINT('Ctrl Pts',(-0.0675673988751837,-0.140110375309755,
0.478235587443016));
#11029=CARTESIAN_POINT('Ctrl Pts',(-0.0669504231951391,-0.140406237540617,
0.478284287954387));
#11030=CARTESIAN_POINT('Ctrl Pts',(-0.0580752564643582,-0.144590398040235,
0.478979364980513));
#11031=CARTESIAN_POINT('Ctrl Pts',(-0.0494908820139851,-0.147749213291722,
0.479584420753534));
#11032=CARTESIAN_POINT('Ctrl Pts',(-0.0338469873846071,-0.151987719206044,
0.480652654654553));
#11033=CARTESIAN_POINT('Ctrl Pts',(-0.0268982386528548,-0.15337002830477,
0.481115843765348));
#11034=CARTESIAN_POINT('Ctrl Pts',(-0.0155100653906487,-0.154837498087777,
0.481883591788931));
#11035=CARTESIAN_POINT('Ctrl Pts',(-0.0111188455925274,-0.155214622642025,
0.482181575334059));
#11036=CARTESIAN_POINT('Ctrl Pts',(-0.00405027554779986,-0.155520181340613,
0.482668845916792));
#11037=CARTESIAN_POINT('Ctrl Pts',(-0.00138036420720576,-0.155566785149004,
0.482854612961654));
#11038=CARTESIAN_POINT('Ctrl Pts',(0.00209202504326187,-0.15553800293797,
0.483099024303547));
#11039=CARTESIAN_POINT('Ctrl Pts',(0.00289468207103836,-0.15552513526461,
0.483155715347063));
#11040=CARTESIAN_POINT('Ctrl Pts',(0.00420048694823484,-0.155494089470242,
0.483248275232321));
#11041=CARTESIAN_POINT('Ctrl Pts',(0.00470371715538929,-0.155479680295672,
0.483284026118819));
#11042=CARTESIAN_POINT('Ctrl Pts',(0.00567170286170136,-0.155447259882393,
0.483352952999139));
#11043=CARTESIAN_POINT('Ctrl Pts',(0.00613646566108345,-0.155429606571105,
0.483386117444879));
#11044=CARTESIAN_POINT('Ctrl Pts',(0.00720090180359724,-0.155384393937088,
0.483462237883674));
#11045=CARTESIAN_POINT('Ctrl Pts',(0.00780050550932397,-0.15535544715613,
0.483505236780354));
#11046=CARTESIAN_POINT('Ctrl Pts',(0.00939387042019223,-0.155269277474624,
0.483619826887047));
#11047=CARTESIAN_POINT('Ctrl Pts',(0.0103872609876461,-0.155205985878364,
0.483691606506616));
#11048=CARTESIAN_POINT('Ctrl Pts',(0.0178920778310046,-0.154655462241151,
0.484236525968052));
#11049=CARTESIAN_POINT('Ctrl Pts',(0.0243666784582232,-0.153768269754051,
0.484722117126193));
#11050=CARTESIAN_POINT('Ctrl Pts',(0.0410630567821762,-0.150399409257983,
0.486015561510219));
#11051=CARTESIAN_POINT('Ctrl Pts',(0.0511231205686958,-0.147283911548327,
0.486837855955399));
#11052=CARTESIAN_POINT('Ctrl Pts',(0.0644392496848606,-0.14163012766054,
0.487950976873036));
#11053=CARTESIAN_POINT('Ctrl Pts',(0.068027086086083,-0.139942239918318,
0.48825322014786));
#11054=CARTESIAN_POINT('Ctrl Pts',(0.0727560866326421,-0.137492578644091,
0.488651505730209));
#11055=CARTESIAN_POINT('Ctrl Pts',(0.073957161220585,-0.136850268324908,
0.488752650540117));
#11056=CARTESIAN_POINT('Ctrl Pts',(0.0757149476048539,-0.135880337076171,
0.488900497519645));
#11057=CARTESIAN_POINT('Ctrl Pts',(0.0762782668814876,-0.135564911882608,
0.488947850524431));
#11058=CARTESIAN_POINT('Ctrl Pts',(0.0772918840699767,-0.134989028169367,
0.489032984083087));
#11059=CARTESIAN_POINT('Ctrl Pts',(0.0777428666557943,-0.134729802843178,
0.489070836139389));
#11060=CARTESIAN_POINT('Ctrl Pts',(0.0784472258989971,-0.134320222009398,
0.489129904028981));
#11061=CARTESIAN_POINT('Ctrl Pts',(0.0787014844571805,-0.134171403958061,
0.489151215858852));
#11062=CARTESIAN_POINT('Ctrl Pts',(0.0791773683102057,-0.133891049978019,
0.4891910824759));
#11063=CARTESIAN_POINT('Ctrl Pts',(0.0793990872681636,-0.133759686974749,
0.489209647567011));
#11064=CARTESIAN_POINT('Ctrl Pts',(0.0799002911315223,-0.133461050739314,
0.489251594870398));
#11065=CARTESIAN_POINT('Ctrl Pts',(0.08017957721249,-0.133293450666705,
0.489274955498335));
#11066=CARTESIAN_POINT('Ctrl Pts',(0.081022439578012,-0.132784039817386,
0.489345421054062));
#11067=CARTESIAN_POINT('Ctrl Pts',(0.0815843816311355,-0.132439516990278,
0.489392353571305));
#11068=CARTESIAN_POINT('Ctrl Pts',(0.0858776605068247,-0.129769641485927,
0.489750695234669));
#11069=CARTESIAN_POINT('Ctrl Pts',(0.089511521009019,-0.127290333644916,
0.490052695432413));
#11070=CARTESIAN_POINT('Ctrl Pts',(0.10484180971496,-0.115849092683232,
0.491343893714127));
#11071=CARTESIAN_POINT('Ctrl Pts',(0.115336420249136,-0.105405770913032,
0.492280662351702));
#11072=CARTESIAN_POINT('Ctrl Pts',(0.12660778001882,-0.0904554742995251,
0.493555391767838));
#11073=CARTESIAN_POINT('Ctrl Pts',(0.128886111333087,-0.0871784858382005,
0.493830845358089));
#11074=CARTESIAN_POINT('Ctrl Pts',(0.131529973887771,-0.0830452256196419,
0.49417555558678));
#11075=CARTESIAN_POINT('Ctrl Pts',(0.132017287071481,-0.0822683376463375,
0.494240230570442));
#11076=CARTESIAN_POINT('Ctrl Pts',(0.132774677104978,-0.0810368260556379,
0.494342592506802));
#11077=CARTESIAN_POINT('Ctrl Pts',(0.133049360016668,-0.0805850472736843,
0.494380110308273));
#11078=CARTESIAN_POINT('Ctrl Pts',(0.133558821153511,-0.0797374166033444,
0.494450443594424));
#11079=CARTESIAN_POINT('Ctrl Pts',(0.133794156892778,-0.079341904990258,
0.494483238316564));
#11080=CARTESIAN_POINT('Ctrl Pts',(0.134315362871283,-0.0784570391010249,
0.494556560300084));
#11081=CARTESIAN_POINT('Ctrl Pts',(0.134600319671333,-0.0779671572933243,
0.494597120056372));
#11082=CARTESIAN_POINT('Ctrl Pts',(0.135312722173778,-0.0767268890445578,
0.494699731659987));
#11083=CARTESIAN_POINT('Ctrl Pts',(0.13573660288336,-0.0759744882595893,
0.494761910347876));
#11084=CARTESIAN_POINT('Ctrl Pts',(0.138064530579706,-0.0717606759675843,
0.495109796803931));
#11085=CARTESIAN_POINT('Ctrl Pts',(0.139842271893258,-0.0682315394491492,
0.495399924999162));
#11086=CARTESIAN_POINT('Ctrl Pts',(0.142300711081877,-0.0628504271923861,
0.495840983464642));
#11087=CARTESIAN_POINT('Ctrl Pts',(0.143083764667252,-0.061046738526805,
0.495988596044243));
#11088=CARTESIAN_POINT('Ctrl Pts',(0.149414031658429,-0.0456741817785139,
0.497244582644813));
#11089=CARTESIAN_POINT('Ctrl Pts',(0.153050942097622,-0.0314008743230206,
0.498406742355253));
#11090=CARTESIAN_POINT('Ctrl Pts',(0.154924694426822,-0.0141853042412813,
0.499710367010844));
#11091=CARTESIAN_POINT('Ctrl Pts',(0.155144717481925,-0.0115326815911267,
0.499908258261993));
#11092=CARTESIAN_POINT('Ctrl Pts',(0.155327579760841,-0.00833310466792126,
0.500142395278582));
#11093=CARTESIAN_POINT('Ctrl Pts',(0.155355738177683,-0.0077905267289172,
0.500181942085597));
#11094=CARTESIAN_POINT('Ctrl Pts',(0.155395099642321,-0.00694668107853892,
0.500243190936549));
#11095=CARTESIAN_POINT('Ctrl Pts',(0.155408270309878,-0.00664551686200445,
0.50026499958461));
#11096=CARTESIAN_POINT('Ctrl Pts',(0.155431073642886,-0.00608688946849056,
0.500305355847305));
#11097=CARTESIAN_POINT('Ctrl Pts',(0.155440942071776,-0.00582944310631814,
0.500323915996993));
#11098=CARTESIAN_POINT('Ctrl Pts',(0.155461799888879,-0.00524753886955188,
0.500365781886261));
#11099=CARTESIAN_POINT('Ctrl Pts',(0.155472413197397,-0.00492307106106822,
0.500389066396508));
#11100=CARTESIAN_POINT('Ctrl Pts',(0.155500721623952,-0.00396593599087978,
0.50045758255323));
#11101=CARTESIAN_POINT('Ctrl Pts',(0.155515571620106,-0.00333318080103419,
0.500502659162807));
#11102=CARTESIAN_POINT('Ctrl Pts',(0.155594566512995,0.00121654713528559,
0.50082531643342));
#11103=CARTESIAN_POINT('Ctrl Pts',(0.155514588212892,0.00513503335253237,
0.501095442046556));
#11104=CARTESIAN_POINT('Ctrl Pts',(0.155224819022421,0.0101089143053874,
0.501433209105386));
#11105=CARTESIAN_POINT('Ctrl Pts',(0.155152039359066,0.0111704682524216,
0.501504999509196));
#11106=CARTESIAN_POINT('Ctrl Pts',(0.154158416206782,0.0237677088421316,
0.502354247233721));
#11107=CARTESIAN_POINT('Ctrl Pts',(0.151963932812225,0.0351668696930953,
0.503098801121396));
#11108=CARTESIAN_POINT('Ctrl Pts',(0.146632486672816,0.052300049104295,
0.504300374314306));
#11109=CARTESIAN_POINT('Ctrl Pts',(0.144368162367733,0.0582597473445544,
0.504734403320023));
#11110=CARTESIAN_POINT('Ctrl Pts',(0.141317601395188,0.0650093513068715,
0.505253859661951));
#11111=CARTESIAN_POINT('Ctrl Pts',(0.140880595348656,0.0659510271546518,
0.50532697711584));
#11112=CARTESIAN_POINT('Ctrl Pts',(0.140195597801441,0.067389203563851,
0.505439673701972));
#11113=CARTESIAN_POINT('Ctrl Pts',(0.139954314025153,0.067888882529719,
0.505479021149259));
#11114=CARTESIAN_POINT('Ctrl Pts',(0.139510188859246,0.0687961991023488,
0.505550824406271));
#11115=CARTESIAN_POINT('Ctrl Pts',(0.139308220465525,0.0692042593278585,
0.505583249573012));
#11116=CARTESIAN_POINT('Ctrl Pts',(0.138864296785653,0.0700913517546344,
0.505654031086156));
#11117=CARTESIAN_POINT('Ctrl Pts',(0.138621648894121,0.0705700287452655,
0.505692411327243));
#11118=CARTESIAN_POINT('Ctrl Pts',(0.137952627848658,0.0718730569520019,
0.505797404005634));
#11119=CARTESIAN_POINT('Ctrl Pts',(0.137521352297071,0.0726948515301451,
0.505864187992973));
#11120=CARTESIAN_POINT('Ctrl Pts',(0.135329385860168,0.0767823182649117,
0.506199256833229));
#11121=CARTESIAN_POINT('Ctrl Pts',(0.133459752358724,0.0799878567360161,
0.506471379390095));
#11122=CARTESIAN_POINT('Ctrl Pts',(0.129883640070248,0.0856442538859851,
0.506969282705803));
#11123=CARTESIAN_POINT('Ctrl Pts',(0.1282177271067,0.0881187304214564,0.507193581156044));
#11124=CARTESIAN_POINT('Ctrl Pts',(0.120411447203032,0.0990234409545753,
0.508211271586583));
#11125=CARTESIAN_POINT('Ctrl Pts',(0.113503947172465,0.106870849970884,
0.509027138066551));
#11126=CARTESIAN_POINT('Ctrl Pts',(0.102857147538016,0.116760679644628,
0.510146181466628));
#11127=CARTESIAN_POINT('Ctrl Pts',(0.0997402815676494,0.119434210948601,
0.510459519811949));
#11128=CARTESIAN_POINT('Ctrl Pts',(0.09487486750574,0.123284097739597,0.510923764924525));
#11129=CARTESIAN_POINT('Ctrl Pts',(0.0932023539512702,0.124553328511343,
0.511079175914049));
#11130=CARTESIAN_POINT('Ctrl Pts',(0.0910960020863834,0.12608559053669,
0.511269295003979));
#11131=CARTESIAN_POINT('Ctrl Pts',(0.0906860015093899,0.126380801099234,
0.511306043821766));
#11132=CARTESIAN_POINT('Ctrl Pts',(0.0900358894915702,0.12684410510161,
0.511363898933324));
#11133=CARTESIAN_POINT('Ctrl Pts',(0.0897967337674781,0.127013522918407,
0.511385093896668));
#11134=CARTESIAN_POINT('Ctrl Pts',(0.0893454814969487,0.127331278256141,
0.511424917969795));
#11135=CARTESIAN_POINT('Ctrl Pts',(0.0891334962161335,0.127479760511008,
0.511443556558521));
#11136=CARTESIAN_POINT('Ctrl Pts',(0.0886490671948899,0.127817273241531,
0.511485992441576));
#11137=CARTESIAN_POINT('Ctrl Pts',(0.0883763891443588,0.128005961973545,
0.511509766390563));
#11138=CARTESIAN_POINT('Ctrl Pts',(0.0876531826104626,0.128502996559307,
0.511572529269652));
#11139=CARTESIAN_POINT('Ctrl Pts',(0.0872016251804054,0.128809848753669,
0.511611419662326));
#11140=CARTESIAN_POINT('Ctrl Pts',(0.0841006168665344,0.130893333112102,
0.511876534584703));
#11141=CARTESIAN_POINT('Ctrl Pts',(0.0813984343165668,0.132590637159455,
0.51209781452478));
#11142=CARTESIAN_POINT('Ctrl Pts',(0.0778791106639981,0.134653021236762,
0.512376398738253));
#11143=CARTESIAN_POINT('Ctrl Pts',(0.0771086542724344,0.13509569757276,
0.512436814285568));
#11144=CARTESIAN_POINT('Ctrl Pts',(0.0655367818292574,0.141613227791855,
0.513336351889971));
#11145=CARTESIAN_POINT('Ctrl Pts',(0.0540505877705848,0.146382902925483,
0.514130696433513));
#11146=CARTESIAN_POINT('Ctrl Pts',(0.0379624645776529,0.150908252378661,
0.515248958307355));
#11147=CARTESIAN_POINT('Ctrl Pts',(0.0337590056200117,0.151903831450294,
0.515541228482873));
#11148=CARTESIAN_POINT('Ctrl Pts',(0.0269357746227456,0.153222692128533,
0.516020018771936));
#11149=CARTESIAN_POINT('Ctrl Pts',(0.0243395976488883,0.153656473652998,
0.516203176168421));
#11150=CARTESIAN_POINT('Ctrl Pts',(0.020942987189616,0.154135757097126,
0.516444630632217));
#11151=CARTESIAN_POINT('Ctrl Pts',(0.0201513455757505,0.15424125115262,
0.516501033693001));
#11152=CARTESIAN_POINT('Ctrl Pts',(0.0188603177378919,0.154403184715411,
0.51659324040369));
#11153=CARTESIAN_POINT('Ctrl Pts',(0.0183614009725772,0.154463309491148,
0.516628927805409));
#11154=CARTESIAN_POINT('Ctrl Pts',(0.0173998799815613,0.154574458689163,
0.516697813577958));
#11155=CARTESIAN_POINT('Ctrl Pts',(0.0169373202021491,0.154625826685374,
0.516731000761746));
#11156=CARTESIAN_POINT('Ctrl Pts',(0.015875617953295,0.154738909241769,
0.516807288675343));
#11157=CARTESIAN_POINT('Ctrl Pts',(0.0152763369178987,0.154799220896665,
0.516850432947526));
#11158=CARTESIAN_POINT('Ctrl Pts',(0.0136789591696513,0.154950614913672,
0.516965663510083));
#11159=CARTESIAN_POINT('Ctrl Pts',(0.01268032153837,0.155035532521845,0.517037941569458));
#11160=CARTESIAN_POINT('Ctrl Pts',(0.00489320014901267,0.155621958577393,
0.517603499032958));
#11161=CARTESIAN_POINT('Ctrl Pts',(-0.0019197227178117,0.155686950441743,
0.518110349161898));
#11162=CARTESIAN_POINT('Ctrl Pts',(-0.022709745869486,0.154520431489838,
0.519694167932434));
#11163=CARTESIAN_POINT('Ctrl Pts',(-0.0365335872077338,0.151847146766974,
0.520804791631584));
#11164=CARTESIAN_POINT('Ctrl Pts',(-0.0518989612148523,0.14665317734524,
0.522019864148303));
#11165=CARTESIAN_POINT('Ctrl Pts',(-0.0539710667562702,0.145903330712485,
0.522183113000258));
#11166=CARTESIAN_POINT('Ctrl Pts',(-0.0565053145224866,0.144924860436067,
0.522381436127547));
#11167=CARTESIAN_POINT('Ctrl Pts',(-0.0569830405300083,0.144737689817398,
0.522418762312211));
#11168=CARTESIAN_POINT('Ctrl Pts',(-0.0577338071554716,0.144439249961131,
0.522477318770632));
#11169=CARTESIAN_POINT('Ctrl Pts',(-0.0580074665675729,0.144329564692631,
0.522498641301715));
#11170=CARTESIAN_POINT('Ctrl Pts',(-0.0585204821753058,0.14412224840889,
0.522538570638093));
#11171=CARTESIAN_POINT('Ctrl Pts',(-0.0587599039628375,0.144024799976349,
0.52255718756815));
#11172=CARTESIAN_POINT('Ctrl Pts',(-0.0593084114202115,0.143799953387588,
0.522599798650671));
#11173=CARTESIAN_POINT('Ctrl Pts',(-0.0596173298069143,0.143672155450658,
0.522623768388046));
#11174=CARTESIAN_POINT('Ctrl Pts',(-0.0605742888472609,0.143272648488029,
0.522697939199957));
#11175=CARTESIAN_POINT('Ctrl Pts',(-0.0612209145136707,0.142997538265821,
0.522747940134679));
#11176=CARTESIAN_POINT('Ctrl Pts',(-0.0624750809416945,0.142453880004019,
0.522844734101855));
#11177=CARTESIAN_POINT('Ctrl Pts',(-0.0630827451941917,0.142185831871624,
0.522891546874463));
#11178=CARTESIAN_POINT('Ctrl Pts',(-0.0636886260274623,0.141913922554251,
0.522938154987668));
#11179=CARTESIAN_POINT('Origin',(0.,0.,-0.129405622560373));
#11180=CARTESIAN_POINT('',(-0.0636886258321223,0.141913922641917,0.606695238001095));
#11181=CARTESIAN_POINT('',(-0.063688625907641,0.141913922608025,0.592717731153444));
#11182=CARTESIAN_POINT('',(-0.0636886258329924,0.141913922641526,-0.129405622560373));
#11183=CARTESIAN_POINT('',(-0.155549999999463,-4.08543441352296E-7,0.54940562255668));
#11184=CARTESIAN_POINT('Ctrl Pts',(-0.0636886258321223,0.141913922641917,
0.606695238001095));
#11185=CARTESIAN_POINT('Ctrl Pts',(-0.0636228496240879,0.14194344191828,
0.606690392871029));
#11186=CARTESIAN_POINT('Ctrl Pts',(-0.0635570512475328,0.14197291620284,
0.606685546573706));
#11187=CARTESIAN_POINT('Ctrl Pts',(-0.0583496585560615,0.144301214160662,
0.60630203832958));
#11188=CARTESIAN_POINT('Ctrl Pts',(-0.0530876043388053,0.146318888920545,
0.605917040173728));
#11189=CARTESIAN_POINT('Ctrl Pts',(-0.0468144616707361,0.148341263218698,
0.605454986388314));
#11190=CARTESIAN_POINT('Ctrl Pts',(-0.0458980334977013,0.148627368417361,
0.605387417318009));
#11191=CARTESIAN_POINT('Ctrl Pts',(-0.0444081656620055,0.149077405893748,
0.605277428635648));
#11192=CARTESIAN_POINT('Ctrl Pts',(-0.0438363181890301,0.149246558805094,
0.605235179268839));
#11193=CARTESIAN_POINT('Ctrl Pts',(-0.0428185119163103,0.149541272472045,
0.605159916262343));
#11194=CARTESIAN_POINT('Ctrl Pts',(-0.0423729355252007,0.149668137764049,
0.605126945431326));
#11195=CARTESIAN_POINT('Ctrl Pts',(-0.0414351677004477,0.149930617351041,
0.605057504686982));
#11196=CARTESIAN_POINT('Ctrl Pts',(-0.0409428629847105,0.150065802569334,
0.605021021313407));
#11197=CARTESIAN_POINT('Ctrl Pts',(-0.0396442999892002,0.150415517988506,
0.604924707635625));
#11198=CARTESIAN_POINT('Ctrl Pts',(-0.0388369753361092,0.150625986701401,
0.604864747064989));
#11199=CARTESIAN_POINT('Ctrl Pts',(-0.0351396480552566,0.151558175603332,
0.604589737204761));
#11200=CARTESIAN_POINT('Ctrl Pts',(-0.032231162169451,0.152203237054385,
0.604372252406214));
#11201=CARTESIAN_POINT('Ctrl Pts',(-0.0242527408110029,0.153733807643722,
0.603772016513123));
#11202=CARTESIAN_POINT('Ctrl Pts',(-0.0191548954397207,0.154451801169225,
0.603384420198587));
#11203=CARTESIAN_POINT('Ctrl Pts',(-0.00144627765254581,0.156055737879248,
0.602026066894407));
#11204=CARTESIAN_POINT('Ctrl Pts',(0.0112299305269262,0.155657820024943,
0.601028703700662));
#11205=CARTESIAN_POINT('Ctrl Pts',(0.0263353323862714,0.153327316201151,
0.59987773287967));
#11206=CARTESIAN_POINT('Ctrl Pts',(0.0289420747006572,0.152856711330897,
0.599680701166667));
#11207=CARTESIAN_POINT('Ctrl Pts',(0.0320409827575366,0.152215124572108,
0.59944934011767));
#11208=CARTESIAN_POINT('Ctrl Pts',(0.032545723287219,0.152108003209668,
0.59941174860009));
#11209=CARTESIAN_POINT('Ctrl Pts',(0.0333686425723911,0.151929070860057,
0.599350620327875));
#11210=CARTESIAN_POINT('Ctrl Pts',(0.0336871394586741,0.151858768334015,
0.599327000937595));
#11211=CARTESIAN_POINT('Ctrl Pts',(0.0342570023710706,0.151731100176208,
0.599284813700123));
#11212=CARTESIAN_POINT('Ctrl Pts',(0.0345084479197196,0.15167411116551,
0.599266224792553));
#11213=CARTESIAN_POINT('Ctrl Pts',(0.0350526537515696,0.151549345965948,
0.599226048746406));
#11214=CARTESIAN_POINT('Ctrl Pts',(0.0353453588916062,0.151481346728645,
0.599204474599771));
#11215=CARTESIAN_POINT('Ctrl Pts',(0.036162193650409,0.151289088824309,
0.599144361502053));
#11216=CARTESIAN_POINT('Ctrl Pts',(0.036685884571956,0.151162953606365,
0.599105928259505));
#11217=CARTESIAN_POINT('Ctrl Pts',(0.0397160170218915,0.150416446973662,
0.598884110716867));
#11218=CARTESIAN_POINT('Ctrl Pts',(0.0422075457645097,0.149736417451604,
0.598703949270332));
#11219=CARTESIAN_POINT('Ctrl Pts',(0.0587852181785379,0.144765030107717,
0.597513020807236));
#11220=CARTESIAN_POINT('Ctrl Pts',(0.0722186342837146,0.13855393980055,
0.596579658534424));
#11221=CARTESIAN_POINT('Ctrl Pts',(0.0861695532009537,0.129515252754879,
0.595462850214944));
#11222=CARTESIAN_POINT('Ctrl Pts',(0.0877407240458845,0.128456052936871,
0.595334845684996));
#11223=CARTESIAN_POINT('Ctrl Pts',(0.0925914559234453,0.125055429738614,
0.594931882655904));
#11224=CARTESIAN_POINT('Ctrl Pts',(0.0957994071019434,0.122615280463015,
0.594653960190692));
#11225=CARTESIAN_POINT('Ctrl Pts',(0.099579670333836,0.11950082552985,0.594310100331516));
#11226=CARTESIAN_POINT('Ctrl Pts',(0.100245878746327,0.118942514627391,
0.594248857339703));
#11227=CARTESIAN_POINT('Ctrl Pts',(0.101340066812819,0.118009815855463,
0.594147178516757));
#11228=CARTESIAN_POINT('Ctrl Pts',(0.101770741751611,0.117638607130564,
0.594106872854714));
#11229=CARTESIAN_POINT('Ctrl Pts',(0.102546522857291,0.116962494872795,
0.594033746325486));
#11230=CARTESIAN_POINT('Ctrl Pts',(0.1028923302962,0.116658402675708,0.594000959308965));
#11231=CARTESIAN_POINT('Ctrl Pts',(0.103631486434597,0.116002568777306,
0.593930463874316));
#11232=CARTESIAN_POINT('Ctrl Pts',(0.104024404747847,0.115650352994551,
0.5938927358718));
#11233=CARTESIAN_POINT('Ctrl Pts',(0.105091360867665,0.114684086748224,
0.59378958423956));
#11234=CARTESIAN_POINT('Ctrl Pts',(0.10576179443667,0.114066106508724,0.593723995148152));
#11235=CARTESIAN_POINT('Ctrl Pts',(0.109280168161355,0.110765317267864,
0.593375618965678));
#11236=CARTESIAN_POINT('Ctrl Pts',(0.112031316967832,0.107981894709485,
0.593088523407152));
#11237=CARTESIAN_POINT('Ctrl Pts',(0.124669916825852,0.0941916737298453,
0.591695220831876));
#11238=CARTESIAN_POINT('Ctrl Pts',(0.133057561929886,0.08191580412155,0.590529038508831));
#11239=CARTESIAN_POINT('Ctrl Pts',(0.141535641214404,0.0646762977072758,
0.58906112746275));
#11240=CARTESIAN_POINT('Ctrl Pts',(0.143317416693748,0.0606258055950618,
0.588727897502056));
#11241=CARTESIAN_POINT('Ctrl Pts',(0.145164090562029,0.0558894004613202,
0.588355527009997));
#11242=CARTESIAN_POINT('Ctrl Pts',(0.145399975062929,0.0552728284622067,
0.588307383158202));
#11243=CARTESIAN_POINT('Ctrl Pts',(0.14574646879012,0.0543495684879227,
0.58823580379183));
#11244=CARTESIAN_POINT('Ctrl Pts',(0.145860046609496,0.054044015098693,
0.588212197872362));
#11245=CARTESIAN_POINT('Ctrl Pts',(0.146061729855145,0.0534961684307075,
0.588170025135612));
#11246=CARTESIAN_POINT('Ctrl Pts',(0.146150193816012,0.0532540122067559,
0.588151437320121));
#11247=CARTESIAN_POINT('Ctrl Pts',(0.146340512909937,0.0527289973380136,
0.588111252742142));
#11248=CARTESIAN_POINT('Ctrl Pts',(0.146442149932301,0.0524460637835971,
0.588089669019786));
#11249=CARTESIAN_POINT('Ctrl Pts',(0.146723809301793,0.0516547877635206,
0.588029502264383));
#11250=CARTESIAN_POINT('Ctrl Pts',(0.146902011740119,0.051145794398306,
0.587991025245594));
#11251=CARTESIAN_POINT('Ctrl Pts',(0.147921394689084,0.0481848824878102,
0.587768447572583));
#11252=CARTESIAN_POINT('Ctrl Pts',(0.148703890567598,0.0457129846195717,
0.58758759565725));
#11253=CARTESIAN_POINT('Ctrl Pts',(0.153513528761999,0.0290856049325191,
0.586396676589063));
#11254=CARTESIAN_POINT('Ctrl Pts',(0.155576383426343,0.014438626043585,
0.585463789960434));
#11255=CARTESIAN_POINT('Ctrl Pts',(0.155546295269917,-0.00218796301726947,
0.58434672181089));
#11256=CARTESIAN_POINT('Ctrl Pts',(0.155507796055369,-0.00409415555346438,
0.584217918350292));
#11257=CARTESIAN_POINT('Ctrl Pts',(0.155279377172575,-0.0100123907218766,
0.583815005829561));
#11258=CARTESIAN_POINT('Ctrl Pts',(0.154969120707362,-0.0140178386724394,
0.583537965206974));
#11259=CARTESIAN_POINT('Ctrl Pts',(0.154403745968478,-0.0188690151277756,
0.583195081118856));
#11260=CARTESIAN_POINT('Ctrl Pts',(0.154296009048926,-0.0197306370431628,
0.583133900104402));
#11261=CARTESIAN_POINT('Ctrl Pts',(0.15410583541604,-0.0211545966022298,
0.583032302909887));
#11262=CARTESIAN_POINT('Ctrl Pts',(0.154027519622246,-0.0217174733830872,
0.582992016529782));
#11263=CARTESIAN_POINT('Ctrl Pts',(0.153880166473009,-0.022735630745161,
0.582918910591882));
#11264=CARTESIAN_POINT('Ctrl Pts',(0.153812188264794,-0.0231910601736626,
0.582886124795862));
#11265=CARTESIAN_POINT('Ctrl Pts',(0.153661943070413,-0.0241679210650832,
0.582815615997633));
#11266=CARTESIAN_POINT('Ctrl Pts',(0.153579042173131,-0.0246892476451226,
0.58277787334162));
#11267=CARTESIAN_POINT('Ctrl Pts',(0.153345564860988,-0.0261107888514442,
0.582674640793021));
#11268=CARTESIAN_POINT('Ctrl Pts',(0.153189718277372,-0.0270101037597491,
0.582608985001122));
#11269=CARTESIAN_POINT('Ctrl Pts',(0.152321687257459,-0.0317697209022288,
0.582259607901591));
#11270=CARTESIAN_POINT('Ctrl Pts',(0.15147154203859,-0.0356030670275371,
0.58197154859614));
#11271=CARTESIAN_POINT('Ctrl Pts',(0.146732535953112,-0.0537024556087539,
0.580577816547525));
#11272=CARTESIAN_POINT('Ctrl Pts',(0.140967667305219,-0.0673970505989316,
0.579412328963373));
#11273=CARTESIAN_POINT('Ctrl Pts',(0.131086073568716,-0.0838555672583985,
0.577945561714988));
#11274=CARTESIAN_POINT('Ctrl Pts',(0.128651744106631,-0.0875445747450963,
0.577612738592707));
#11275=CARTESIAN_POINT('Ctrl Pts',(0.125676769017241,-0.0916601755032032,
0.57724076655518));
#11276=CARTESIAN_POINT('Ctrl Pts',(0.125286739093392,-0.0921925761278503,
0.577192635467388));
#11277=CARTESIAN_POINT('Ctrl Pts',(0.124699032105828,-0.0929841928976501,
0.577121071306377));
#11278=CARTESIAN_POINT('Ctrl Pts',(0.124503916508397,-0.0932452868316977,
0.57709746793281));
#11279=CARTESIAN_POINT('Ctrl Pts',(0.12415300458986,-0.0937117944285697,
0.577055297935442));
#11280=CARTESIAN_POINT('Ctrl Pts',(0.123997517683928,-0.0939174348854666,
0.577036710325181));
#11281=CARTESIAN_POINT('Ctrl Pts',(0.123659590254208,-0.0943620614048785,
0.576996524129416));
#11282=CARTESIAN_POINT('Ctrl Pts',(0.123476968387237,-0.0946009047339768,
0.576974938593164));
#11283=CARTESIAN_POINT('Ctrl Pts',(0.122964785637752,-0.0952667567131231,
0.576914761671966));
#11284=CARTESIAN_POINT('Ctrl Pts',(0.122633690129042,-0.0956925885841168,
0.576876276359242));
#11285=CARTESIAN_POINT('Ctrl Pts',(0.120697442856023,-0.0981562996950603,
0.57665355429208));
#11286=CARTESIAN_POINT('Ctrl Pts',(0.119043607125714,-0.100155646942024,
0.576472571206104));
#11287=CARTESIAN_POINT('Ctrl Pts',(0.107680620676554,-0.113213137062743,
0.575281653641704));
#11288=CARTESIAN_POINT('Ctrl Pts',(0.096493776444301,-0.122887715270571,
0.57434885716864));
#11289=CARTESIAN_POINT('Ctrl Pts',(0.0792849207766551,-0.133950149332071,
0.57297438307565));
#11290=CARTESIAN_POINT('Ctrl Pts',(0.0742896539082768,-0.136783682501102,
0.572582295298205));
#11291=CARTESIAN_POINT('Ctrl Pts',(0.0682088221361338,-0.139801510721322,
0.572106437513219));
#11292=CARTESIAN_POINT('Ctrl Pts',(0.067263247175454,-0.140258908096826,
0.572032488594585));
#11293=CARTESIAN_POINT('Ctrl Pts',(0.0658087321236649,-0.14094440111431,
0.571918775317686));
#11294=CARTESIAN_POINT('Ctrl Pts',(0.0653030631271205,-0.141179401332923,
0.57187924927641));
#11295=CARTESIAN_POINT('Ctrl Pts',(0.0644001080599986,-0.141593143760605,
0.571808675958053));
#11296=CARTESIAN_POINT('Ctrl Pts',(0.0640033118394637,-0.141772946448386,
0.571777665461824));
#11297=CARTESIAN_POINT('Ctrl Pts',(0.0632117003290168,-0.142127653574691,
0.571715801367291));
#11298=CARTESIAN_POINT('Ctrl Pts',(0.0628169015662974,-0.142302585499374,
0.571684949042528));
#11299=CARTESIAN_POINT('Ctrl Pts',(0.061714924764121,-0.142785382455695,
0.571598832446714));
#11300=CARTESIAN_POINT('Ctrl Pts',(0.0610061861341762,-0.143089631333867,
0.571543445805745));
#11301=CARTESIAN_POINT('Ctrl Pts',(0.0580919589163292,-0.144315070443383,
0.571315677331949));
#11302=CARTESIAN_POINT('Ctrl Pts',(0.0558677516706189,-0.145190593327374,
0.571141769268236));
#11303=CARTESIAN_POINT('Ctrl Pts',(0.0500746385180267,-0.147318135892371,
0.570688333058454));
#11304=CARTESIAN_POINT('Ctrl Pts',(0.046478842937778,-0.148491802528006,
0.570406393919639));
#11305=CARTESIAN_POINT('Ctrl Pts',(0.0353359879743188,-0.151684443058084,
0.569531267476946));
#11306=CARTESIAN_POINT('Ctrl Pts',(0.0276771766279245,-0.153266937053795,
0.568927145015773));
#11307=CARTESIAN_POINT('Ctrl Pts',(0.0113399063064241,-0.155377857221553,
0.567649605839236));
#11308=CARTESIAN_POINT('Ctrl Pts',(0.00266832128430588,-0.155768374592577,
0.566977973686294));
#11309=CARTESIAN_POINT('Ctrl Pts',(-0.00715261114397514,-0.1553898092933,
0.566251387244432));
#11310=CARTESIAN_POINT('Ctrl Pts',(-0.00831322979201837,-0.15533204146457,
0.566166077189831));
#11311=CARTESIAN_POINT('Ctrl Pts',(-0.00989530206442547,-0.155235512635428,
0.566050643659634));
#11312=CARTESIAN_POINT('Ctrl Pts',(-0.0103173662344781,-0.155208032496642,
0.566019931492819));
#11313=CARTESIAN_POINT('Ctrl Pts',(-0.0109862204691736,-0.155161743711987,
0.565971398494046));
#11314=CARTESIAN_POINT('Ctrl Pts',(-0.0112330824516254,-0.15514406728241,
0.565953515494623));
#11315=CARTESIAN_POINT('Ctrl Pts',(-0.0117413654193336,-0.155106452395721,
0.565916757325326));
#11316=CARTESIAN_POINT('Ctrl Pts',(-0.0120027781935027,-0.155086442197625,
0.565897886696641));
#11317=CARTESIAN_POINT('Ctrl Pts',(-0.0126229524521631,-0.15503739265832,
0.565853197251119));
#11318=CARTESIAN_POINT('Ctrl Pts',(-0.0129816690795313,-0.155007768598415,
0.565827411076315));
#11319=CARTESIAN_POINT('Ctrl Pts',(-0.0141792421804365,-0.154904682487028,
0.565741523969575));
#11320=CARTESIAN_POINT('Ctrl Pts',(-0.0150176245902908,-0.154825652271663,
0.565681724821987));
#11321=CARTESIAN_POINT('Ctrl Pts',(-0.02515584389605,-0.153786843985333,
0.56496211148084));
#11322=CARTESIAN_POINT('Ctrl Pts',(-0.0343531694731221,-0.151997136882406,
0.564344490736005));
#11323=CARTESIAN_POINT('Ctrl Pts',(-0.0550549351542557,-0.145991999442293,
0.562924871311521));
#11324=CARTESIAN_POINT('Ctrl Pts',(-0.0663321685042083,-0.141225721967393,
0.562126286630674));
#11325=CARTESIAN_POINT('Ctrl Pts',(-0.0784320973250131,-0.13433976176749,
0.561158522064545));
#11326=CARTESIAN_POINT('Ctrl Pts',(-0.0799138460732735,-0.133463636530446,
0.561038040599918));
#11327=CARTESIAN_POINT('Ctrl Pts',(-0.0819663793336351,-0.132203583362628,
0.560868212987029));
#11328=CARTESIAN_POINT('Ctrl Pts',(-0.0825496601606235,-0.131840162223192,
0.560819614476925));
#11329=CARTESIAN_POINT('Ctrl Pts',(-0.0835313938487909,-0.131219410556196,
0.560737234379471));
#11330=CARTESIAN_POINT('Ctrl Pts',(-0.0839311168765511,-0.130964098423174,
0.560703527541403));
#11331=CARTESIAN_POINT('Ctrl Pts',(-0.0846963427535504,-0.130470389157694,
0.560638678537535));
#11332=CARTESIAN_POINT('Ctrl Pts',(-0.0850620229337815,-0.130232273918793,
0.560607547082493));
#11333=CARTESIAN_POINT('Ctrl Pts',(-0.0858131449618687,-0.129738662295228,
0.560543306096664));
#11334=CARTESIAN_POINT('Ctrl Pts',(-0.0861984586774024,-0.129482979790762,
0.560510189811726));
#11335=CARTESIAN_POINT('Ctrl Pts',(-0.0875221592688026,-0.128596085229633,
0.560395859201348));
#11336=CARTESIAN_POINT('Ctrl Pts',(-0.088454778928397,-0.127956373262866,
0.560314325677068));
#11337=CARTESIAN_POINT('Ctrl Pts',(-0.0983836808740542,-0.120985417633,
0.55943551362049));
#11338=CARTESIAN_POINT('Ctrl Pts',(-0.106689080910222,-0.113728451407107,
0.558601108919804));
#11339=CARTESIAN_POINT('Ctrl Pts',(-0.121642185123988,-0.0975723848635565,
0.556898317575468));
#11340=CARTESIAN_POINT('Ctrl Pts',(-0.128246305142112,-0.0887136817832488,
0.556035138823591));
#11341=CARTESIAN_POINT('Ctrl Pts',(-0.134447582447173,-0.0782367206849143,
0.555135180266414));
#11342=CARTESIAN_POINT('Ctrl Pts',(-0.135024904544559,-0.0772360813042496,
0.555050376911829));
#11343=CARTESIAN_POINT('Ctrl Pts',(-0.135797800454722,-0.0758613068925079,
0.554935520383834));
#11344=CARTESIAN_POINT('Ctrl Pts',(-0.136003059105635,-0.0754927043956593,
0.554904885841469));
#11345=CARTESIAN_POINT('Ctrl Pts',(-0.136326244569571,-0.0749067332774861,
0.554856445414567));
#11346=CARTESIAN_POINT('Ctrl Pts',(-0.13644515502325,-0.0746899144582098,
0.554838577772579));
#11347=CARTESIAN_POINT('Ctrl Pts',(-0.136689130198624,-0.0742425281514594,
0.554801826374327));
#11348=CARTESIAN_POINT('Ctrl Pts',(-0.136814128794541,-0.0740119278505793,
0.554782947245642));
#11349=CARTESIAN_POINT('Ctrl Pts',(-0.137109611852291,-0.0734635073364975,
0.5547381977602));
#11350=CARTESIAN_POINT('Ctrl Pts',(-0.137279576835164,-0.0731454056213762,
0.554712360288195));
#11351=CARTESIAN_POINT('Ctrl Pts',(-0.137844637208956,-0.0720789471289757,
0.554626124892199));
#11352=CARTESIAN_POINT('Ctrl Pts',(-0.138234741335024,-0.0713279398287831,
0.554566032109108));
#11353=CARTESIAN_POINT('Ctrl Pts',(-0.139153994011338,-0.0695223733999668,
0.554422979475206));
#11354=CARTESIAN_POINT('Ctrl Pts',(-0.139677320218167,-0.0684648879000127,
0.554340345784201));
#11355=CARTESIAN_POINT('Ctrl Pts',(-0.141576080191444,-0.0645156519965605,
0.55403560803146));
#11356=CARTESIAN_POINT('Ctrl Pts',(-0.142874242108495,-0.0615874162646004,
0.553817265486979));
#11357=CARTESIAN_POINT('Ctrl Pts',(-0.148533561568301,-0.0476776978490142,
0.552805796688296));
#11358=CARTESIAN_POINT('Ctrl Pts',(-0.15172489064108,-0.0362625009691681,
0.552046512952225));
#11359=CARTESIAN_POINT('Ctrl Pts',(-0.154592044357726,-0.018357808113916,
0.550832585222723));
#11360=CARTESIAN_POINT('Ctrl Pts',(-0.155209887669435,-0.0120658091122547,
0.550402388706692));
#11361=CARTESIAN_POINT('Ctrl Pts',(-0.155483355582146,-0.00467842002347808,
0.549884384452491));
#11362=CARTESIAN_POINT('Ctrl Pts',(-0.155512009975409,-0.00360223917708829,
0.549808612953919));
#11363=CARTESIAN_POINT('Ctrl Pts',(-0.15553847222879,-0.00197283667481611,
0.549693384679298));
#11364=CARTESIAN_POINT('Ctrl Pts',(-0.155544503861204,-0.00141976478831956,
0.549654184370811));
#11365=CARTESIAN_POINT('Ctrl Pts',(-0.155549213861576,-0.000574435365012869,
0.549594130454558));
#11366=CARTESIAN_POINT('Ctrl Pts',(-0.155550018564031,-0.000282189959955681,
0.549573343335134));
#11367=CARTESIAN_POINT('Ctrl Pts',(-0.155549999675089,1.00538485301794E-5,
0.549552530512073));
#11368=CARTESIAN_POINT('Ctrl Pts',(-0.0636886258329926,0.141913922641526,
0.536610014060325));
#11369=CARTESIAN_POINT('Ctrl Pts',(-0.0730814786960769,0.137698565329387,
0.537345736058591));
#11370=CARTESIAN_POINT('Ctrl Pts',(-0.0820642535703313,0.132542130691616,
0.538081458056857));
#11371=CARTESIAN_POINT('Ctrl Pts',(-0.0904466417708162,0.126551205021452,
0.538817180055122));
#11372=CARTESIAN_POINT('Ctrl Pts',(-0.0988275438342714,0.120561341499243,
0.539552771615179));
#11373=CARTESIAN_POINT('Ctrl Pts',(-0.106607530543232,0.113737839536412,
0.540288363175235));
#11374=CARTESIAN_POINT('Ctrl Pts',(-0.113627370286093,0.106229107225219,
0.541023954735291));
#11375=CARTESIAN_POINT('Ctrl Pts',(-0.120663580662677,0.0987028641572448,
0.541761261733369));
#11376=CARTESIAN_POINT('Ctrl Pts',(-0.126935523776145,0.0904889250916622,
0.542498568731447));
#11377=CARTESIAN_POINT('Ctrl Pts',(-0.132323914233961,0.0817690908705926,
0.543235875729525));
#11378=CARTESIAN_POINT('Ctrl Pts',(-0.133802785515336,0.0793758878336476,
0.543438233400809));
#11379=CARTESIAN_POINT('Ctrl Pts',(-0.135215366375327,0.0769447282492072,
0.543640591072093));
#11380=CARTESIAN_POINT('Ctrl Pts',(-0.136559806045013,0.0744796742269222,
0.543842948743377));
#11381=CARTESIAN_POINT('Ctrl Pts',(-0.141705683718826,0.0650446160803692,
0.544617477973856));
#11382=CARTESIAN_POINT('Ctrl Pts',(-0.145885002942362,0.0550465854919305,
0.545392007204334));
#11383=CARTESIAN_POINT('Ctrl Pts',(-0.148989921630324,0.0446968203856833,
0.546166536434813));
#11384=CARTESIAN_POINT('Ctrl Pts',(-0.152081349398532,0.0343920251690047,
0.546937700323798));
#11385=CARTESIAN_POINT('Ctrl Pts',(-0.15410734778821,0.0237392552038595,
0.547708864212783));
#11386=CARTESIAN_POINT('Ctrl Pts',(-0.155008465445465,0.012968351485135,
0.548480028101768));
#11387=CARTESIAN_POINT('Ctrl Pts',(-0.155368989547926,0.00865906915711002,
0.548788559586739));
#11388=CARTESIAN_POINT('Ctrl Pts',(-0.155550011375819,0.00433105777467094,
0.549097091071709));
#11389=CARTESIAN_POINT('Ctrl Pts',(-0.155549999999463,-4.08543441352294E-7,
0.54940562255668));
#11390=CARTESIAN_POINT('Ctrl Pts',(-0.0636886260274623,0.141913922554251,
0.522938154987668));
#11391=CARTESIAN_POINT('Ctrl Pts',(-0.0693125037711184,0.139390019049978,
0.523370778560055));
#11392=CARTESIAN_POINT('Ctrl Pts',(-0.0747827181519514,0.136533442705235,
0.523785861625993));
#11393=CARTESIAN_POINT('Ctrl Pts',(-0.0881720709049043,0.128494339908574,
0.524823008133113));
#11394=CARTESIAN_POINT('Ctrl Pts',(-0.0958138441722195,0.122901661705836,
0.525436271246095));
#11395=CARTESIAN_POINT('Ctrl Pts',(-0.106154319408019,0.113779985617878,
0.526358747946524));
#11396=CARTESIAN_POINT('Ctrl Pts',(-0.109286072117201,0.110775331897159,
0.526652340563003));
#11397=CARTESIAN_POINT('Ctrl Pts',(-0.114115429594705,0.105737622239116,
0.527133095389452));
#11398=CARTESIAN_POINT('Ctrl Pts',(-0.115893938886627,0.103785208557242,
0.527316858833636));
#11399=CARTESIAN_POINT('Ctrl Pts',(-0.118145049350833,0.101183937358877,
0.527559000245081));
#11400=CARTESIAN_POINT('Ctrl Pts',(-0.118663613682811,0.100575288269287,
0.527615470531124));
#11401=CARTESIAN_POINT('Ctrl Pts',(-0.119500535509174,0.0995774937518589,
0.527707759678011));
#11402=CARTESIAN_POINT('Ctrl Pts',(-0.119821744516277,0.0991907494635538,
0.527743461893031));
#11403=CARTESIAN_POINT('Ctrl Pts',(-0.120436640666833,0.0984430526750521,
0.527812357178973));
#11404=CARTESIAN_POINT('Ctrl Pts',(-0.120730594469286,0.0980823255512263,
0.527845538978341));
#11405=CARTESIAN_POINT('Ctrl Pts',(-0.121401012161318,0.0972520383144402,
0.527921787440167));
#11406=CARTESIAN_POINT('Ctrl Pts',(-0.121776376259455,0.0967816040184198,
0.527964897494571));
#11407=CARTESIAN_POINT('Ctrl Pts',(-0.122768537492344,0.0955232430470036,
0.528079977202787));
#11408=CARTESIAN_POINT('Ctrl Pts',(-0.123380468652547,0.0947315344976719,
0.528152137831722));
#11409=CARTESIAN_POINT('Ctrl Pts',(-0.128056496002495,0.0885595849195694,
0.528712908761808));
#11410=CARTESIAN_POINT('Ctrl Pts',(-0.131773904598353,0.0829269526565161,
0.529214825829898));
#11411=CARTESIAN_POINT('Ctrl Pts',(-0.142082778030083,0.0648545460312558,
0.530796773084979));
#11412=CARTESIAN_POINT('Ctrl Pts',(-0.147361903220405,0.0517499558580485,
0.531911261649214));
#11413=CARTESIAN_POINT('Ctrl Pts',(-0.151352150844595,0.035961937829689,
0.533131441400601));
#11414=CARTESIAN_POINT('Ctrl Pts',(-0.151850193278327,0.0337972591956748,
0.533296019281844));
#11415=CARTESIAN_POINT('Ctrl Pts',(-0.152406305096423,0.0311188887216352,
0.533495729511515));
#11416=CARTESIAN_POINT('Ctrl Pts',(-0.152508375606618,0.0306147425012116,
0.533533150547508));
#11417=CARTESIAN_POINT('Ctrl Pts',(-0.152665069153205,0.0298205675109193,
0.533591822177884));
#11418=CARTESIAN_POINT('Ctrl Pts',(-0.152721369540717,0.029530880037654,
0.533613165624603));
#11419=CARTESIAN_POINT('Ctrl Pts',(-0.152825430129839,0.0289871902928638,
0.533653112515148));
#11420=CARTESIAN_POINT('Ctrl Pts',(-0.152873381138254,0.0287332322634315,
0.533671726189034));
#11421=CARTESIAN_POINT('Ctrl Pts',(-0.152981823220601,0.0281509452489734,
0.533714301494299));
#11422=CARTESIAN_POINT('Ctrl Pts',(-0.153041890338123,0.0278225405328822,
0.533738238860759));
#11423=CARTESIAN_POINT('Ctrl Pts',(-0.153196620213558,0.0269609222069499,
0.533800852382747));
#11424=CARTESIAN_POINT('Ctrl Pts',(-0.153289557658122,0.0264273969038806,
0.533839433249556));
#11425=CARTESIAN_POINT('Ctrl Pts',(-0.153896325876387,0.0228331999091928,
0.534098128723025));
#11426=CARTESIAN_POINT('Ctrl Pts',(-0.154321290711703,0.0197579567617597,
0.534313566233528));
#11427=CARTESIAN_POINT('Ctrl Pts',(-0.155245941276463,0.0111805388222644,
0.534903316546242));
#11428=CARTESIAN_POINT('Ctrl Pts',(-0.155545066027013,0.00566119306105173,
0.53527023616306));
#11429=CARTESIAN_POINT('Ctrl Pts',(-0.155561771596661,-0.0132742945436004,
0.536520045667977));
#11430=CARTESIAN_POINT('Ctrl Pts',(-0.153839235067069,-0.0266292059187267,
0.537391592974479));
#11431=CARTESIAN_POINT('Ctrl Pts',(-0.150008356577863,-0.0411823023591037,
0.538438671652821));
#11432=CARTESIAN_POINT('Ctrl Pts',(-0.149566095899624,-0.042760632256689,
0.538553469462463));
#11433=CARTESIAN_POINT('Ctrl Pts',(-0.148922893840937,-0.0449238909266402,
0.538712653086854));
#11434=CARTESIAN_POINT('Ctrl Pts',(-0.148743271099596,-0.0455150916585728,
0.538756347441353));
#11435=CARTESIAN_POINT('Ctrl Pts',(-0.148429384043841,-0.0465264982652633,
0.538831433186879));
#11436=CARTESIAN_POINT('Ctrl Pts',(-0.148296844728414,-0.0469472355389249,
0.538862768041952));
#11437=CARTESIAN_POINT('Ctrl Pts',(-0.14802078951082,-0.0478107204855038,
0.538927285240482));
#11438=CARTESIAN_POINT('Ctrl Pts',(-0.147877072678076,-0.0482533987223313,
0.538960473889777));
#11439=CARTESIAN_POINT('Ctrl Pts',(-0.147539533466966,-0.0492774196686756,
0.539037512847962));
#11440=CARTESIAN_POINT('Ctrl Pts',(-0.147344259241144,-0.0498582718677507,
0.539081410518519));
#11441=CARTESIAN_POINT('Ctrl Pts',(-0.146714689743651,-0.0516949516154911,
0.539220859009577));
#11442=CARTESIAN_POINT('Ctrl Pts',(-0.146267742511014,-0.0529463455401811,
0.539316825654902));
#11443=CARTESIAN_POINT('Ctrl Pts',(-0.142400915940452,-0.0633501656378722,
0.540122905774491));
#11444=CARTESIAN_POINT('Ctrl Pts',(-0.138142413652402,-0.0721655577750554,
0.540861584510963));
#11445=CARTESIAN_POINT('Ctrl Pts',(-0.126822870264277,-0.0908744721940083,
0.542548868396242));
#11446=CARTESIAN_POINT('Ctrl Pts',(-0.119372412477284,-0.10046131888096,
0.543500752540934));
#11447=CARTESIAN_POINT('Ctrl Pts',(-0.11015969864138,-0.109825837202611,
0.544469936043691));
#11448=CARTESIAN_POINT('Ctrl Pts',(-0.109426476438798,-0.110556411533628,
0.544545815320775));
#11449=CARTESIAN_POINT('Ctrl Pts',(-0.108397557470002,-0.111561348991582,
0.54465049827888));
#11450=CARTESIAN_POINT('Ctrl Pts',(-0.108108025918828,-0.111841941131645,
0.544679761096987));
#11451=CARTESIAN_POINT('Ctrl Pts',(-0.107641822430754,-0.112290248458939,
0.544726564703862));
#11452=CARTESIAN_POINT('Ctrl Pts',(-0.107465844555686,-0.112458677261316,
0.544744160180144));
#11453=CARTESIAN_POINT('Ctrl Pts',(-0.107097768355951,-0.112809310838233,
0.544780812731165));
#11454=CARTESIAN_POINT('Ctrl Pts',(-0.106905599877627,-0.112991439122484,
0.54479986358994));
#11455=CARTESIAN_POINT('Ctrl Pts',(-0.106440345862733,-0.11343013564948,
0.544845784904675));
#11456=CARTESIAN_POINT('Ctrl Pts',(-0.106166793917122,-0.113686211908599,
0.544872617676915));
#11457=CARTESIAN_POINT('Ctrl Pts',(-0.105210563100172,-0.114574893138384,
0.544965845410856));
#11458=CARTESIAN_POINT('Ctrl Pts',(-0.104523115705746,-0.115202374635666,
0.545031863601993));
#11459=CARTESIAN_POINT('Ctrl Pts',(-0.10046826675944,-0.11883734144804,
0.545415733863223));
#11460=CARTESIAN_POINT('Ctrl Pts',(-0.0969764752657212,-0.121703569171678,
0.545724251167426));
#11461=CARTESIAN_POINT('Ctrl Pts',(-0.0884836528162996,-0.128076870265841,
0.546438066479018));
#11462=CARTESIAN_POINT('Ctrl Pts',(-0.0833912005378006,-0.131449446043761,
0.54683875943586));
#11463=CARTESIAN_POINT('Ctrl Pts',(-0.0688114013467321,-0.13991605661537,
0.547948398322483));
#11464=CARTESIAN_POINT('Ctrl Pts',(-0.058975438721653,-0.144337677161704,
0.548658324127951));
#11465=CARTESIAN_POINT('Ctrl Pts',(-0.0470954517241333,-0.148259582951455,
0.549527651141724));
#11466=CARTESIAN_POINT('Ctrl Pts',(-0.0454189706477286,-0.148781726627143,
0.54965051885225));
#11467=CARTESIAN_POINT('Ctrl Pts',(-0.0430565765930316,-0.149473850905517,
0.549824084939934));
#11468=CARTESIAN_POINT('Ctrl Pts',(-0.0423777519413163,-0.149667721981832,
0.549874007337901));
#11469=CARTESIAN_POINT('Ctrl Pts',(-0.0412792271964498,-0.149973386061135,
0.549954884570839));
#11470=CARTESIAN_POINT('Ctrl Pts',(-0.0408603315021957,-0.150088055577804,
0.549985745957495));
#11471=CARTESIAN_POINT('Ctrl Pts',(-0.0399876933493037,-0.150323009648652,
0.550050082098602));
#11472=CARTESIAN_POINT('Ctrl Pts',(-0.0395338762873895,-0.150442997397799,
0.550083566077444));
#11473=CARTESIAN_POINT('Ctrl Pts',(-0.0384623869174121,-0.150721112702892,
0.550162688381621));
#11474=CARTESIAN_POINT('Ctrl Pts',(-0.037844275835988,-0.15087749926949,
0.5502083822503));
#11475=CARTESIAN_POINT('Ctrl Pts',(-0.0358019864413543,-0.151380873770935,
0.550359536614289));
#11476=CARTESIAN_POINT('Ctrl Pts',(-0.0343739032366468,-0.151711521248621,
0.550465518022388));
#11477=CARTESIAN_POINT('Ctrl Pts',(-0.0268574250332789,-0.153340255712135,
0.551025005229703));
#11478=CARTESIAN_POINT('Ctrl Pts',(-0.0207006495548377,-0.15429199289901,
0.551489350421596));
#11479=CARTESIAN_POINT('Ctrl Pts',(-0.00415077271920622,-0.155841926362421,
0.552753384634826));
#11480=CARTESIAN_POINT('Ctrl Pts',(0.00627339725513827,-0.155770825443758,
0.553567563328912));
#11481=CARTESIAN_POINT('Ctrl Pts',(0.0187372909922365,-0.15443214955363,
0.554531483828088));
#11482=CARTESIAN_POINT('Ctrl Pts',(0.0208585245858162,-0.154159973800621,
0.55469509530889));
#11483=CARTESIAN_POINT('Ctrl Pts',(0.02645734918772,-0.153323901271539,
0.555124793947395));
#11484=CARTESIAN_POINT('Ctrl Pts',(0.0299228350788113,-0.152685424671255,
0.555388573096077));
#11485=CARTESIAN_POINT('Ctrl Pts',(0.0339128536530036,-0.151809211373921,
0.555687567446266));
#11486=CARTESIAN_POINT('Ctrl Pts',(0.0344610902840289,-0.151685699995515,
0.555728545343533));
#11487=CARTESIAN_POINT('Ctrl Pts',(0.0353363367607763,-0.15148352685256,
0.555793785451161));
#11488=CARTESIAN_POINT('Ctrl Pts',(0.0356637747607796,-0.1514067725664,
0.55581815198941));
#11489=CARTESIAN_POINT('Ctrl Pts',(0.0362433417141194,-0.151268932626566,
0.555861206189086));
#11490=CARTESIAN_POINT('Ctrl Pts',(0.0364955696305209,-0.151208277545038,
0.555879918186122));
#11491=CARTESIAN_POINT('Ctrl Pts',(0.0370297634157288,-0.151078401545684,
0.555919493958265));
#11492=CARTESIAN_POINT('Ctrl Pts',(0.037311687081137,-0.15100902225746,
0.555940348468868));
#11493=CARTESIAN_POINT('Ctrl Pts',(0.0380716396381659,-0.150819745517151,
0.555996482087961));
#11494=CARTESIAN_POINT('Ctrl Pts',(0.038549301225703,-0.150698363545474,
0.556031677021169));
#11495=CARTESIAN_POINT('Ctrl Pts',(0.0409102182154071,-0.150086454293043,
0.556205237886987));
#11496=CARTESIAN_POINT('Ctrl Pts',(0.0427848393735488,-0.149562856959651,
0.556341801440567));
#11497=CARTESIAN_POINT('Ctrl Pts',(0.0481602952309036,-0.147952096144847,
0.556731115449568));
#11498=CARTESIAN_POINT('Ctrl Pts',(0.051633341615043,-0.146776153148321,
0.556979838778363));
#11499=CARTESIAN_POINT('Ctrl Pts',(0.064024622280468,-0.142086203195988,
0.557867870622627));
#11500=CARTESIAN_POINT('Ctrl Pts',(0.0726549765943762,-0.137872806403243,
0.558488735123943));
#11501=CARTESIAN_POINT('Ctrl Pts',(0.0875190128081615,-0.128830465016337,
0.559644579137773));
#11502=CARTESIAN_POINT('Ctrl Pts',(0.0938785881956358,-0.124272480144846,
0.560172389791356));
#11503=CARTESIAN_POINT('Ctrl Pts',(0.100654469344356,-0.118598194769974,
0.560791343911244));
#11504=CARTESIAN_POINT('Ctrl Pts',(0.101434094282203,-0.1179320924507,0.560863461331539));
#11505=CARTESIAN_POINT('Ctrl Pts',(0.102666203566894,-0.116858136747144,
0.560978917589372));
#11506=CARTESIAN_POINT('Ctrl Pts',(0.103122986361702,-0.116455240945192,
0.561022051956307));
#11507=CARTESIAN_POINT('Ctrl Pts',(0.103925401992304,-0.115739063921458,
0.561098419233729));
#11508=CARTESIAN_POINT('Ctrl Pts',(0.104272016163796,-0.115426889125279,
0.561131605613918));
#11509=CARTESIAN_POINT('Ctrl Pts',(0.104986945006736,-0.114777147043085,
0.561200472242016));
#11510=CARTESIAN_POINT('Ctrl Pts',(0.105355047501936,-0.114439355382329,
0.56123616174279));
#11511=CARTESIAN_POINT('Ctrl Pts',(0.106297601602329,-0.113566012527091,
0.561328150041716));
#11512=CARTESIAN_POINT('Ctrl Pts',(0.106869629941809,-0.113027879135312,
0.561384558662525));
#11513=CARTESIAN_POINT('Ctrl Pts',(0.109254497547434,-0.110750034851705,
0.561622220382414));
#11514=CARTESIAN_POINT('Ctrl Pts',(0.111029027113239,-0.108970955866384,
0.561805171668631));
#11515=CARTESIAN_POINT('Ctrl Pts',(0.11554913318028,-0.10421419968529,0.562287871917499));
#11516=CARTESIAN_POINT('Ctrl Pts',(0.118222720882528,-0.101171066098921,
0.56259044114648));
#11517=CARTESIAN_POINT('Ctrl Pts',(0.125839483265111,-0.0917868518480665,
0.563505312772759));
#11518=CARTESIAN_POINT('Ctrl Pts',(0.13041291285108,-0.0851636777831778,
0.564128483714476));
#11519=CARTESIAN_POINT('Ctrl Pts',(0.136261706820665,-0.0751097640991976,
0.565030292753454));
#11520=CARTESIAN_POINT('Ctrl Pts',(0.137961396377216,-0.071940141979813,
0.565308622955537));
#11521=CARTESIAN_POINT('Ctrl Pts',(0.140106264183853,-0.0675842011487671,
0.565681164445715));
#11522=CARTESIAN_POINT('Ctrl Pts',(0.140649029198706,-0.0664472740911736,
0.565777506874568));
#11523=CARTESIAN_POINT('Ctrl Pts',(0.142826587703963,-0.061739692689556,
0.566172457221779));
#11524=CARTESIAN_POINT('Ctrl Pts',(0.144339862352576,-0.0581139789411102,
0.566467360911001));
#11525=CARTESIAN_POINT('Ctrl Pts',(0.145936017904574,-0.0538412687175233,
0.56680132077099));
#11526=CARTESIAN_POINT('Ctrl Pts',(0.14615401237522,-0.0532466735353458,
0.566847494981841));
#11527=CARTESIAN_POINT('Ctrl Pts',(0.146478284494606,-0.0523452014197282,
0.566917029975448));
#11528=CARTESIAN_POINT('Ctrl Pts',(0.14658723892096,-0.0520393056345255,
0.566940543688161));
#11529=CARTESIAN_POINT('Ctrl Pts',(0.146780922706548,-0.0514900923321722,
0.566982611944645));
#11530=CARTESIAN_POINT('Ctrl Pts',(0.146866005739974,-0.0512469046910303,
0.567001187083172));
#11531=CARTESIAN_POINT('Ctrl Pts',(0.147049308861439,-0.0507187746132098,
0.567041412837719));
#11532=CARTESIAN_POINT('Ctrl Pts',(0.147147304892852,-0.0504337585538178,
0.567063050118036));
#11533=CARTESIAN_POINT('Ctrl Pts',(0.147419539488799,-0.0496344310634207,
0.567123536955249));
#11534=CARTESIAN_POINT('Ctrl Pts',(0.147591916549682,-0.0491194825170829,
0.567162278622683));
#11535=CARTESIAN_POINT('Ctrl Pts',(0.148591637926296,-0.0460801946676753,
0.567389669026069));
#11536=CARTESIAN_POINT('Ctrl Pts',(0.149356968406698,-0.0435357033627789,
0.567574902170907));
#11537=CARTESIAN_POINT('Ctrl Pts',(0.15391810093453,-0.0268311733729513,
0.568765389268736));
#11538=CARTESIAN_POINT('Ctrl Pts',(0.155761446085182,-0.0122135808111399,
0.569694930178027));
#11539=CARTESIAN_POINT('Ctrl Pts',(0.155499901656167,0.00440750625721281,
0.570811857355879));
#11540=CARTESIAN_POINT('Ctrl Pts',(0.155432007072187,0.00636680891806572,
0.570944334246211));
#11541=CARTESIAN_POINT('Ctrl Pts',(0.155115349972588,0.0122755013757389,
0.571347068131));
#11542=CARTESIAN_POINT('Ctrl Pts',(0.154752922132215,0.0162169124391543,
0.571620108153867));
#11543=CARTESIAN_POINT('Ctrl Pts',(0.154128797092813,0.0209967378612288,
0.571958550284801));
#11544=CARTESIAN_POINT('Ctrl Pts',(0.154009787734688,0.0218525587142995,
0.572019433297928));
#11545=CARTESIAN_POINT('Ctrl Pts',(0.15380090287758,0.0232681354354257,
0.572120631130542));
#11546=CARTESIAN_POINT('Ctrl Pts',(0.153715085226818,0.0238284789878695,
0.572160817886219));
#11547=CARTESIAN_POINT('Ctrl Pts',(0.153554047141098,0.0248428848968651,
0.572233807818604));
#11548=CARTESIAN_POINT('Ctrl Pts',(0.153479870395448,0.025297108499979,
0.572266577654775));
#11549=CARTESIAN_POINT('Ctrl Pts',(0.153316167097562,0.0262723209686628,
0.57233712428238));
#11550=CARTESIAN_POINT('Ctrl Pts',(0.153225998612155,0.0267931946422494,
0.572374921028864));
#11551=CARTESIAN_POINT('Ctrl Pts',(0.152972231815096,0.0282159337340021,
0.572478486498202));
#11552=CARTESIAN_POINT('Ctrl Pts',(0.152803316620583,0.0291168162049528,
0.572544423001337));
#11553=CARTESIAN_POINT('Ctrl Pts',(0.151857865829933,0.0339242571912706,
0.572898255308876));
#11554=CARTESIAN_POINT('Ctrl Pts',(0.150939529743546,0.0378010532882317,
0.573190622452226));
#11555=CARTESIAN_POINT('Ctrl Pts',(0.145928221523231,0.0558389479353133,
0.574585869721996));
#11556=CARTESIAN_POINT('Ctrl Pts',(0.139984618828454,0.0694060379413062,
0.575747797526563));
#11557=CARTESIAN_POINT('Ctrl Pts',(0.129906718422113,0.0856703163387146,
0.577209533666793));
#11558=CARTESIAN_POINT('Ctrl Pts',(0.12743150627182,0.0893105743709335,
0.577540981851726));
#11559=CARTESIAN_POINT('Ctrl Pts',(0.124411527018555,0.0933702791090407,
0.577911595776505));
#11560=CARTESIAN_POINT('Ctrl Pts',(0.12401469572336,0.0938967111370229,
0.577959672801102));
#11561=CARTESIAN_POINT('Ctrl Pts',(0.123416798135735,0.0946794726338518,
0.578031168012147));
#11562=CARTESIAN_POINT('Ctrl Pts',(0.123218261005705,0.0949377098961141,
0.57805475607818));
#11563=CARTESIAN_POINT('Ctrl Pts',(0.122861192975882,0.0953991413846882,
0.578096904140811));
#11564=CARTESIAN_POINT('Ctrl Pts',(0.122702967686102,0.0956025660792466,
0.578115485075473));
#11565=CARTESIAN_POINT('Ctrl Pts',(0.122359070869421,0.0960424419440706,
0.57815566268024));
#11566=CARTESIAN_POINT('Ctrl Pts',(0.122173219725323,0.0962787477314077,
0.578177246283805));
#11567=CARTESIAN_POINT('Ctrl Pts',(0.121651912165297,0.0969376390825866,
0.578237432017959));
#11568=CARTESIAN_POINT('Ctrl Pts',(0.121314935987773,0.0973590259488018,
0.578275927983178));
#11569=CARTESIAN_POINT('Ctrl Pts',(0.119342324291338,0.099799622042576,
0.578498975345491));
#11570=CARTESIAN_POINT('Ctrl Pts',(0.117658365088442,0.101779497897026,
0.578680261555918));
#11571=CARTESIAN_POINT('Ctrl Pts',(0.106120526202603,0.114675522262285,
0.57987074767686));
#11572=CARTESIAN_POINT('Ctrl Pts',(0.0948102604855902,0.124190034508338,
0.580802968658051));
#11573=CARTESIAN_POINT('Ctrl Pts',(0.0805585735780984,0.133080732784228,
0.581931485852659));
#11574=CARTESIAN_POINT('Ctrl Pts',(0.0787643933659321,0.134150419339113,
0.58207267139487));
#11575=CARTESIAN_POINT('Ctrl Pts',(0.0735939059578258,0.13709356614276,
0.582477920900257));
#11576=CARTESIAN_POINT('Ctrl Pts',(0.0701688606252284,0.138877772169655,
0.582744481637431));
#11577=CARTESIAN_POINT('Ctrl Pts',(0.0658383334649136,0.140932561071735,
0.583081059724209));
#11578=CARTESIAN_POINT('Ctrl Pts',(0.0649918760668528,0.141324905453235,
0.583146824538289));
#11579=CARTESIAN_POINT('Ctrl Pts',(0.0636582524998469,0.14192854291008,
0.583250426735509));
#11580=CARTESIAN_POINT('Ctrl Pts',(0.0631734360664162,0.142145001202198,
0.58328808694569));
#11581=CARTESIAN_POINT('Ctrl Pts',(0.0623023098357494,0.142528600130034,
0.583355755340711));
#11582=CARTESIAN_POINT('Ctrl Pts',(0.0619164099142628,0.142696663741093,
0.583385731702458));
#11583=CARTESIAN_POINT('Ctrl Pts',(0.0610514947559166,0.143069174672798,
0.583452920093837));
#11584=CARTESIAN_POINT('Ctrl Pts',(0.0605721272073822,0.143272785785984,
0.583490160102854));
#11585=CARTESIAN_POINT('Ctrl Pts',(0.0592464988251205,0.143828003738642,
0.583593152954099));
#11586=CARTESIAN_POINT('Ctrl Pts',(0.0583981514064706,0.144174540498715,
0.583659075957717));
#11587=CARTESIAN_POINT('Ctrl Pts',(0.0538488911843001,0.145986103479568,
0.584012702045417));
#11588=CARTESIAN_POINT('Ctrl Pts',(0.0500961601432995,0.147316037378406,
0.584304870274994));
#11589=CARTESIAN_POINT('Ctrl Pts',(0.032224297022644,0.152887810891637,
0.585700026177644));
#11590=CARTESIAN_POINT('Ctrl Pts',(0.017600403115368,0.155251960987593,
0.586862094208258));
#11591=CARTESIAN_POINT('Ctrl Pts',(-0.00153278850207716,0.155604688009956,
0.58832406579133));
#11592=CARTESIAN_POINT('Ctrl Pts',(-0.0059346966032725,0.155499056735746,
0.588655600127666));
#11593=CARTESIAN_POINT('Ctrl Pts',(-0.0109844704383491,0.155163070780574,
0.589026298474553));
#11594=CARTESIAN_POINT('Ctrl Pts',(-0.0116420078729264,0.155115121181916,
0.589074378230013));
#11595=CARTESIAN_POINT('Ctrl Pts',(-0.0126239542045381,0.155037235480348,
0.589145876694541));
#11596=CARTESIAN_POINT('Ctrl Pts',(-0.0129485945608784,0.155010459354629,
0.589169465305529));
#11597=CARTESIAN_POINT('Ctrl Pts',(-0.0135299268060048,0.154960672421424,
0.58921161395427));
#11598=CARTESIAN_POINT('Ctrl Pts',(-0.0137866466142657,0.154938043408745,
0.589230194932599));
#11599=CARTESIAN_POINT('Ctrl Pts',(-0.0143427124966196,0.154887634992414,
0.589270372189876));
#11600=CARTESIAN_POINT('Ctrl Pts',(-0.0146420338248949,0.154859625871129,
0.589291955404241));
#11601=CARTESIAN_POINT('Ctrl Pts',(-0.0154782965400792,0.154778925934398,
0.589352138956825));
#11602=CARTESIAN_POINT('Ctrl Pts',(-0.0160150549304179,0.154724308419198,
0.589390633142117));
#11603=CARTESIAN_POINT('Ctrl Pts',(-0.0191349079331047,0.154390440360469,
0.589613649436506));
#11604=CARTESIAN_POINT('Ctrl Pts',(-0.0217111616717617,0.154049279045929,
0.589794907421937));
#11605=CARTESIAN_POINT('Ctrl Pts',(-0.0378786016877545,0.151494597106192,
0.590921004805059));
#11606=CARTESIAN_POINT('Ctrl Pts',(-0.0511309123138129,0.14754961718002,
0.591797849353644));
#11607=CARTESIAN_POINT('Ctrl Pts',(-0.0636886259076391,0.141913922608026,
0.592717731153444));
#11608=CARTESIAN_POINT('Origin',(0.,0.,-0.129405622560373));
#11609=CARTESIAN_POINT('',(-0.0636886255638827,0.141913922762298,0.676466729580158));
#11610=CARTESIAN_POINT('',(-0.063688650901166,0.141913911391341,0.662679920979917));
#11611=CARTESIAN_POINT('',(-0.0636886258329924,0.141913922641526,-0.129405622560373));
#11612=CARTESIAN_POINT('Ctrl Pts',(-0.0636886255638827,0.141913922762298,
0.676466729580158));
#11613=CARTESIAN_POINT('Ctrl Pts',(-0.0607908715473581,0.143214386923548,
0.676246520920293));
#11614=CARTESIAN_POINT('Ctrl Pts',(-0.0578533659458898,0.144426060804552,
0.676030425544921));
#11615=CARTESIAN_POINT('Ctrl Pts',(-0.0408568520024256,0.15083479002351,
0.674809111787695));
#11616=CARTESIAN_POINT('Ctrl Pts',(-0.0261433107887304,0.154068097680774,
0.67385525957657));
#11617=CARTESIAN_POINT('Ctrl Pts',(-0.0078701255115844,0.155386513139834,
0.672601056777744));
#11618=CARTESIAN_POINT('Ctrl Pts',(-0.00453975603769017,0.155519436523196,
0.67237013173076));
#11619=CARTESIAN_POINT('Ctrl Pts',(-0.000341490133210229,0.155552038151604,
0.672074937499572));
#11620=CARTESIAN_POINT('Ctrl Pts',(0.000524931679086567,0.15555152709313,
0.672013798845211));
#11621=CARTESIAN_POINT('Ctrl Pts',(0.00190891973239365,0.155539147769742,
0.671915771196146));
#11622=CARTESIAN_POINT('Ctrl Pts',(0.00242651880768871,0.155531933885506,
0.671879027710959));
#11623=CARTESIAN_POINT('Ctrl Pts',(0.00340580789169315,0.155513395738248,
0.671809349983256));
#11624=CARTESIAN_POINT('Ctrl Pts',(0.00386750335110679,0.15550259866258,
0.671776432571904));
#11625=CARTESIAN_POINT('Ctrl Pts',(0.00491255867777641,0.155473502273566,
0.671701767952502));
#11626=CARTESIAN_POINT('Ctrl Pts',(0.0054958745005055,0.155453975466281,
0.671659982850067));
#11627=CARTESIAN_POINT('Ctrl Pts',(0.00721718720756023,0.1553866533049,
0.671536346550711));
#11628=CARTESIAN_POINT('Ctrl Pts',(0.00835476284272535,0.155329641813805,
0.671454209125888));
#11629=CARTESIAN_POINT('Ctrl Pts',(0.0198533780149537,0.154626692247295,
0.670619448973276));
#11630=CARTESIAN_POINT('Ctrl Pts',(0.0301234881892788,0.152957712150837,
0.669834050183851));
#11631=CARTESIAN_POINT('Ctrl Pts',(0.0470126485828665,0.148445566887118,
0.668483817470187));
#11632=CARTESIAN_POINT('Ctrl Pts',(0.0537426513860412,0.146143778992174,
0.667929810837915));
#11633=CARTESIAN_POINT('Ctrl Pts',(0.0635997597744231,0.141999121179274,
0.667109106033747));
#11634=CARTESIAN_POINT('Ctrl Pts',(0.0668588781187584,0.140494036329267,
0.66683623820975));
#11635=CARTESIAN_POINT('Ctrl Pts',(0.0712011965062588,0.138303350058065,
0.666473088430787));
#11636=CARTESIAN_POINT('Ctrl Pts',(0.0723320966343983,0.137715268133416,
0.66637855216442));
#11637=CARTESIAN_POINT('Ctrl Pts',(0.0739984014708397,0.136822579119382,
0.666239454945605));
#11638=CARTESIAN_POINT('Ctrl Pts',(0.0745393992203288,0.136528603499958,
0.666194325393266));
#11639=CARTESIAN_POINT('Ctrl Pts',(0.0755172149347744,0.13598971838742,
0.666112832243787));
#11640=CARTESIAN_POINT('Ctrl Pts',(0.0759546196334397,0.135745898772536,
0.666076405632637));
#11641=CARTESIAN_POINT('Ctrl Pts',(0.0766436851665365,0.135357424138557,
0.666019073651056));
#11642=CARTESIAN_POINT('Ctrl Pts',(0.0768961263943522,0.135214172684108,
0.665998081143176));
#11643=CARTESIAN_POINT('Ctrl Pts',(0.0771487200101584,0.135069898575509,
0.665977088361396));
#11644=CARTESIAN_POINT('Ctrl Pts',(0.0771492720245886,0.135069583276473,
0.665977042484134));
#11645=CARTESIAN_POINT('Ctrl Pts',(0.0771501308440659,0.135069092729863,
0.665976971108763));
#11646=CARTESIAN_POINT('Ctrl Pts',(0.0771504376505049,0.135068917484595,
0.665976945610496));
#11647=CARTESIAN_POINT('Ctrl Pts',(0.0771510513544071,0.135068566939294,
0.665976894606436));
#11648=CARTESIAN_POINT('Ctrl Pts',(0.0771513582558655,0.135068391636978,
0.665976869100309));
#11649=CARTESIAN_POINT('Ctrl Pts',(0.0771519721411672,0.135068040982512,
0.665976818081246));
#11650=CARTESIAN_POINT('Ctrl Pts',(0.0771522791404123,0.135067865621564,
0.665976792567029));
#11651=CARTESIAN_POINT('Ctrl Pts',(0.0771528932496153,0.135067514833651,
0.665976741529432));
#11652=CARTESIAN_POINT('Ctrl Pts',(0.0771532003271718,0.135067339425193,
0.665976716008743));
#11653=CARTESIAN_POINT('Ctrl Pts',(0.0773655494028303,0.134946040691334,
0.665959068054596));
#11654=CARTESIAN_POINT('Ctrl Pts',(0.077577303495344,0.134824419585031,
0.665941478558442));
#11655=CARTESIAN_POINT('Ctrl Pts',(0.0780710238609456,0.134539302677585,
0.665900487357142));
#11656=CARTESIAN_POINT('Ctrl Pts',(0.0783527630941476,0.134375419078258,
0.665877110976581));
#11657=CARTESIAN_POINT('Ctrl Pts',(0.0792033740451375,0.133877046316535,
0.665806573386037));
#11658=CARTESIAN_POINT('Ctrl Pts',(0.079770644310064,0.133539815554879,
0.665759585052068));
#11659=CARTESIAN_POINT('Ctrl Pts',(0.0841173711352894,0.130918191637871,
0.665399805444364));
#11660=CARTESIAN_POINT('Ctrl Pts',(0.0878005854559817,0.128477123788497,
0.665096507782301));
#11661=CARTESIAN_POINT('Ctrl Pts',(0.103336613985805,0.117199850045557,
0.663800907098825));
#11662=CARTESIAN_POINT('Ctrl Pts',(0.113999507537604,0.106857014813201,
0.662861121678506));
#11663=CARTESIAN_POINT('Ctrl Pts',(0.12544618821654,0.0920569741290184,
0.661586645131116));
#11664=CARTESIAN_POINT('Ctrl Pts',(0.12773062221633,0.0888600938032811,
0.661315370790834));
#11665=CARTESIAN_POINT('Ctrl Pts',(0.13039374320141,0.0848180855891804,
0.660975279324153));
#11666=CARTESIAN_POINT('Ctrl Pts',(0.130889278264255,0.0840513692992772,
0.660910894952173));
#11667=CARTESIAN_POINT('Ctrl Pts',(0.131660672036104,0.0828344652946929,
0.660808882154693));
#11668=CARTESIAN_POINT('Ctrl Pts',(0.131941042702394,0.0823871497247103,
0.660771420850201));
#11669=CARTESIAN_POINT('Ctrl Pts',(0.132461689178739,0.0815470136505976,
0.660701126512285));
#11670=CARTESIAN_POINT('Ctrl Pts',(0.132702508990537,0.0811545355150301,
0.660668313917629));
#11671=CARTESIAN_POINT('Ctrl Pts',(0.133236610303401,0.0802753453795863,
0.660594865223563));
#11672=CARTESIAN_POINT('Ctrl Pts',(0.133528973289228,0.0797880860619735,
0.660554196181564));
#11673=CARTESIAN_POINT('Ctrl Pts',(0.134261236267001,0.0785523813350681,
0.660451145471877));
#11674=CARTESIAN_POINT('Ctrl Pts',(0.1346975474557,0.0778018433584267,0.660388635116091));
#11675=CARTESIAN_POINT('Ctrl Pts',(0.137115563779064,0.0735610862337354,
0.660035837665069));
#11676=CARTESIAN_POINT('Ctrl Pts',(0.138967708229039,0.0699991558691533,
0.659740983235701));
#11677=CARTESIAN_POINT('Ctrl Pts',(0.141494432897997,0.0646434225112803,
0.659299267926378));
#11678=CARTESIAN_POINT('Ctrl Pts',(0.142277062937266,0.0629021736573755,
0.659155914057853));
#11679=CARTESIAN_POINT('Ctrl Pts',(0.148813127614827,0.0476138338661142,
0.65789966310097));
#11680=CARTESIAN_POINT('Ctrl Pts',(0.15264810577264,0.0333301975951108,
0.656732500227976));
#11681=CARTESIAN_POINT('Ctrl Pts',(0.154731474706446,0.0161463172334283,
0.655430319233572));
#11682=CARTESIAN_POINT('Ctrl Pts',(0.154979265361752,0.0135632696176046,
0.655237493306741));
#11683=CARTESIAN_POINT('Ctrl Pts',(0.155200396084705,0.0104369779531962,
0.655008542478591));
#11684=CARTESIAN_POINT('Ctrl Pts',(0.155235656017167,0.00989871596476052,
0.654969281737277));
#11685=CARTESIAN_POINT('Ctrl Pts',(0.155286208205535,0.00906015656793316,
0.654908374939859));
#11686=CARTESIAN_POINT('Ctrl Pts',(0.155303430507879,0.00875998701815042,
0.654886624195271));
#11687=CARTESIAN_POINT('Ctrl Pts',(0.155333803735065,0.008202340025924,
0.654846313948852));
#11688=CARTESIAN_POINT('Ctrl Pts',(0.155347184752105,0.00794488238741016,
0.6548277422226));
#11689=CARTESIAN_POINT('Ctrl Pts',(0.155376033967548,0.00736184781897832,
0.654785772137834));
#11690=CARTESIAN_POINT('Ctrl Pts',(0.155391118953179,0.00703625543535908,
0.654762395417264));
#11691=CARTESIAN_POINT('Ctrl Pts',(0.155433651256396,0.00605128740409831,
0.654691855786703));
#11692=CARTESIAN_POINT('Ctrl Pts',(0.155457926377431,0.00539177058821119,
0.654644865767439));
#11693=CARTESIAN_POINT('Ctrl Pts',(0.155612369792172,0.000317377488226763,
0.654285041866687));
#11694=CARTESIAN_POINT('Ctrl Pts',(0.15555865896183,-0.00410159738035948,
0.653981704214066));
#11695=CARTESIAN_POINT('Ctrl Pts',(0.154507946121226,-0.0232720049461217,
0.652685998820199));
#11696=CARTESIAN_POINT('Ctrl Pts',(0.151599564718293,-0.0378406168766032,
0.651746148175031));
#11697=CARTESIAN_POINT('Ctrl Pts',(0.145371370846084,-0.0554831997448552,
0.650471686413573));
#11698=CARTESIAN_POINT('Ctrl Pts',(0.143924621975196,-0.0591347580392705,
0.650200512720392));
#11699=CARTESIAN_POINT('Ctrl Pts',(0.141973291618426,-0.0635627263621239,
0.649860532849883));
#11700=CARTESIAN_POINT('Ctrl Pts',(0.141597853050832,-0.0643947487261666,
0.64979615587648));
#11701=CARTESIAN_POINT('Ctrl Pts',(0.140993768041352,-0.0657026525380222,
0.649694152158946));
#11702=CARTESIAN_POINT('Ctrl Pts',(0.140769980015533,-0.0661807667752452,
0.649656692485117));
#11703=CARTESIAN_POINT('Ctrl Pts',(0.140346437926841,-0.0670737795170796,
0.64958639960946));
#11704=CARTESIAN_POINT('Ctrl Pts',(0.140147266288204,-0.0674889493252753,
0.649553586838374));
#11705=CARTESIAN_POINT('Ctrl Pts',(0.139698183198175,-0.0684144944302647,
0.649480135678284));
#11706=CARTESIAN_POINT('Ctrl Pts',(0.139447313508257,-0.0689243946400924,
0.649439464336476));
#11707=CARTESIAN_POINT('Ctrl Pts',(0.138806098136054,-0.0702098531222488,
0.64933640391563));
#11708=CARTESIAN_POINT('Ctrl Pts',(0.138412046943202,-0.0709835301980151,
0.649273886106094));
#11709=CARTESIAN_POINT('Ctrl Pts',(0.136159428374096,-0.0753162225599389,
0.648920971943723));
#11710=CARTESIAN_POINT('Ctrl Pts',(0.134170251038917,-0.0788052127745625,
0.648626004718085));
#11711=CARTESIAN_POINT('Ctrl Pts',(0.131040288860471,-0.0838324767647021,
0.648184272473799));
#11712=CARTESIAN_POINT('Ctrl Pts',(0.130002392221593,-0.0854331256406525,
0.648041018957942));
#11713=CARTESIAN_POINT('Ctrl Pts',(0.120701593641929,-0.0992148007876205,
0.64678479714447));
#11714=CARTESIAN_POINT('Ctrl Pts',(0.110779271900926,-0.110183149655123,
0.645617555706887));
#11715=CARTESIAN_POINT('Ctrl Pts',(0.0974710130631162,-0.121251509081323,
0.644315407048281));
#11716=CARTESIAN_POINT('Ctrl Pts',(0.0954359874559907,-0.122859681293083,
0.644122668569318));
#11717=CARTESIAN_POINT('Ctrl Pts',(0.0929301613535089,-0.124740043644849,
0.643893807547915));
#11718=CARTESIAN_POINT('Ctrl Pts',(0.0924970894832599,-0.125061512217034,
0.643854551980029));
#11719=CARTESIAN_POINT('Ctrl Pts',(0.0918200125798306,-0.125558664282855,
0.643793651447691));
#11720=CARTESIAN_POINT('Ctrl Pts',(0.0915771612033927,-0.125735899554454,
0.643771901828927));
#11721=CARTESIAN_POINT('Ctrl Pts',(0.0911251070491711,-0.126063808568441,
0.643731592602523));
#11722=CARTESIAN_POINT('Ctrl Pts',(0.0909160456278558,-0.126214664816518,
0.643713020775984));
#11723=CARTESIAN_POINT('Ctrl Pts',(0.0904418049924492,-0.126555081518211,
0.643671049107775));
#11724=CARTESIAN_POINT('Ctrl Pts',(0.0901764049153119,-0.126744328276266,
0.64364767091093));
#11725=CARTESIAN_POINT('Ctrl Pts',(0.0893717952875931,-0.127314258299297,
0.643577122422535));
#11726=CARTESIAN_POINT('Ctrl Pts',(0.088830746239289,-0.127692351859156,
0.643530125085603));
#11727=CARTESIAN_POINT('Ctrl Pts',(0.0846483040597585,-0.130575659077068,
0.643170071970541));
#11728=CARTESIAN_POINT('Ctrl Pts',(0.0809036065800154,-0.1329283780899,
0.642866526092058));
#11729=CARTESIAN_POINT('Ctrl Pts',(0.0642187845658998,-0.142444373853295,
0.641570277701066));
#11730=CARTESIAN_POINT('Ctrl Pts',(0.0503953289308302,-0.147901356878928,
0.640630089722447));
#11731=CARTESIAN_POINT('Ctrl Pts',(0.032196106401791,-0.152231965299856,
0.639355703699344));
#11732=CARTESIAN_POINT('Ctrl Pts',(0.028351012720224,-0.152994693151566,
0.639085049759057));
#11733=CARTESIAN_POINT('Ctrl Pts',(0.0235805968941704,-0.153754967936899,
0.638745646210428));
#11734=CARTESIAN_POINT('Ctrl Pts',(0.0226784799631589,-0.153890614393438,
0.63868130749526));
#11735=CARTESIAN_POINT('Ctrl Pts',(0.0212526578672108,-0.154092198320615,
0.638579350730771));
#11736=CARTESIAN_POINT('Ctrl Pts',(0.0207297100636731,-0.154163420297706,
0.638541899489654));
#11737=CARTESIAN_POINT('Ctrl Pts',(0.0197498307992688,-0.154291797356417,
0.638471614171795));
#11738=CARTESIAN_POINT('Ctrl Pts',(0.0192929870464523,-0.154349587594285,
0.638438800484267));
#11739=CARTESIAN_POINT('Ctrl Pts',(0.0182716410912885,-0.154474181517958,
0.638365336552078));
#11740=CARTESIAN_POINT('Ctrl Pts',(0.0177070182382793,-0.154539920774733,
0.638324653301721));
#11741=CARTESIAN_POINT('Ctrl Pts',(0.0162785674698841,-0.154698304831259,
0.638221542592591));
#11742=CARTESIAN_POINT('Ctrl Pts',(0.0154143100420053,-0.154786809081192,
0.638158986183661));
#11743=CARTESIAN_POINT('Ctrl Pts',(0.0105441372580052,-0.155244346647751,
0.637805467043103));
#11744=CARTESIAN_POINT('Ctrl Pts',(0.00652618807877941,-0.155465074350251,
0.637509915072673));
#11745=CARTESIAN_POINT('Ctrl Pts',(0.000604153676276382,-0.155560437911898,
0.637068094691197));
#11746=CARTESIAN_POINT('Ctrl Pts',(-0.00129654682107055,-0.155556206215626,
0.636925361052969));
#11747=CARTESIAN_POINT('Ctrl Pts',(-0.0179173481626891,-0.155214568757071,
0.635669287651216));
#11748=CARTESIAN_POINT('Ctrl Pts',(-0.0325182388025824,-0.152823689406662,
0.634501636400603));
#11749=CARTESIAN_POINT('Ctrl Pts',(-0.0490328363497881,-0.147642394584557,
0.633199655730459));
#11750=CARTESIAN_POINT('Ctrl Pts',(-0.0514818191483435,-0.146806403639578,
0.633007372754232));
#11751=CARTESIAN_POINT('Ctrl Pts',(-0.0544145526411711,-0.145722851476748,
0.632778979587384));
#11752=CARTESIAN_POINT('Ctrl Pts',(-0.0549191492589548,-0.14553343275501,
0.632739751012789));
#11753=CARTESIAN_POINT('Ctrl Pts',(-0.0557035989922428,-0.14523430000448,
0.63267888317044));
#11754=CARTESIAN_POINT('Ctrl Pts',(-0.0559841291480127,-0.145126393623628,
0.632657139426609));
#11755=CARTESIAN_POINT('Ctrl Pts',(-0.0565047083184651,-0.144924417913407,
0.632616835520038));
#11756=CARTESIAN_POINT('Ctrl Pts',(-0.0567448338330358,-0.144830565851271,
0.632598263167226));
#11757=CARTESIAN_POINT('Ctrl Pts',(-0.0572881290252687,-0.144616662567373,
0.632556283222664));
#11758=CARTESIAN_POINT('Ctrl Pts',(-0.0575911546703196,-0.144496255066921,
0.632532897311704));
#11759=CARTESIAN_POINT('Ctrl Pts',(-0.0585069326082267,-0.144129031471325,
0.632462302527958));
#11760=CARTESIAN_POINT('Ctrl Pts',(-0.0591185042088403,-0.143879259720847,
0.632415266943923));
#11761=CARTESIAN_POINT('Ctrl Pts',(-0.0638248048292751,-0.141922086362662,
0.632054009768443));
#11762=CARTESIAN_POINT('Ctrl Pts',(-0.0678468677682815,-0.140043907651936,
0.63174937006357));
#11763=CARTESIAN_POINT('Ctrl Pts',(-0.0849274118718202,-0.131158857950281,
0.630450232114783));
#11764=CARTESIAN_POINT('Ctrl Pts',(-0.0970271056562661,-0.122478979117119,
0.629508238081551));
#11765=CARTESIAN_POINT('Ctrl Pts',(-0.11051456227126,-0.109532521859507,
0.628234236968684));
#11766=CARTESIAN_POINT('Ctrl Pts',(-0.113210666198235,-0.106743536275944,
0.627966343848601));
#11767=CARTESIAN_POINT('Ctrl Pts',(-0.116406710207291,-0.103179974764915,
0.627630002365092));
#11768=CARTESIAN_POINT('Ctrl Pts',(-0.117007885388992,-0.102497727134985,
0.627565868316161));
#11769=CARTESIAN_POINT('Ctrl Pts',(-0.117948050701247,-0.101411723703796,
0.627464162743053));
#11770=CARTESIAN_POINT('Ctrl Pts',(-0.118291036434266,-0.1010114402217,
0.627426756627974));
#11771=CARTESIAN_POINT('Ctrl Pts',(-0.118929859962621,-0.100258181788982,
0.627356511638086));
#11772=CARTESIAN_POINT('Ctrl Pts',(-0.119226178431301,-0.099905620335656,
0.627323692929973));
#11773=CARTESIAN_POINT('Ctrl Pts',(-0.119885291193279,-0.09911429557228,
0.627250160092359));
#11774=CARTESIAN_POINT('Ctrl Pts',(-0.120247249493325,-0.0986748478825366,
0.627209412672188));
#11775=CARTESIAN_POINT('Ctrl Pts',(-0.121157242471216,-0.0975575976021249,
0.627106030886133));
#11776=CARTESIAN_POINT('Ctrl Pts',(-0.121702001186741,-0.0968771650223936,
0.627043266383169));
#11777=CARTESIAN_POINT('Ctrl Pts',(-0.124753527481387,-0.0929992869566213,
0.626686628009328));
#11778=CARTESIAN_POINT('Ctrl Pts',(-0.12713975376476,-0.089709460591384,
0.626388070035682));
#11779=CARTESIAN_POINT('Ctrl Pts',(-0.130429154726752,-0.0847792123557415,
0.625945803074513));
#11780=CARTESIAN_POINT('Ctrl Pts',(-0.131435999614898,-0.0832097155762332,
0.62580574826096));
#11781=CARTESIAN_POINT('Ctrl Pts',(-0.14015403988719,-0.069066643317702,
0.624550365582026));
#11782=CARTESIAN_POINT('Ctrl Pts',(-0.146067498189948,-0.0554758003983858,
0.623380521592489));
#11783=CARTESIAN_POINT('Ctrl Pts',(-0.150656624586409,-0.0387932093447793,
0.622079420292723));
#11784=CARTESIAN_POINT('Ctrl Pts',(-0.151273595703449,-0.036312985647016,
0.621889556083399));
#11785=CARTESIAN_POINT('Ctrl Pts',(-0.151945968216113,-0.0332943479732488,
0.621663649105777));
#11786=CARTESIAN_POINT('Ctrl Pts',(-0.152060004988231,-0.0327695860510881,
0.621624565164134));
#11787=CARTESIAN_POINT('Ctrl Pts',(-0.152233539435988,-0.0319506189485235,
0.621563872501541));
#11788=CARTESIAN_POINT('Ctrl Pts',(-0.152294905531702,-0.031656821281618,
0.621542160257309));
#11789=CARTESIAN_POINT('Ctrl Pts',(-0.152407413130354,-0.0311102782967215,
0.621501884788927));
#11790=CARTESIAN_POINT('Ctrl Pts',(-0.152458776004204,-0.0308575860024739,
0.621483309529429));
#11791=CARTESIAN_POINT('Ctrl Pts',(-0.152573781388118,-0.0302844916740415,
0.62144128482264));
#11792=CARTESIAN_POINT('Ctrl Pts',(-0.152637043040253,-0.0299640167578431,
0.621417857250302));
#11793=CARTESIAN_POINT('Ctrl Pts',(-0.152825743846724,-0.028991977868985,
0.621347012160336));
#11794=CARTESIAN_POINT('Ctrl Pts',(-0.152948026217467,-0.0283397967778022,
0.621299769743629));
#11795=CARTESIAN_POINT('Ctrl Pts',(-0.153872143155152,-0.023230834555012,
0.620931815243988));
#11796=CARTESIAN_POINT('Ctrl Pts',(-0.154483282768341,-0.0187412167743094,
0.620621090821166));
#11797=CARTESIAN_POINT('Ctrl Pts',(-0.155328034334317,-0.00954638373917771,
0.619998531446841));
#11798=CARTESIAN_POINT('Ctrl Pts',(-0.155545705223899,-0.00484457768735938,
0.619687425983483));
#11799=CARTESIAN_POINT('Ctrl Pts',(-0.155561285277832,0.0124761902052128,
0.618546004554368));
#11800=CARTESIAN_POINT('Ctrl Pts',(-0.154037873253815,0.0250450339594314,
0.617722353371123));
#11801=CARTESIAN_POINT('Ctrl Pts',(-0.150606091338229,0.0389422576042399,
0.616727048739471));
#11802=CARTESIAN_POINT('Ctrl Pts',(-0.150171387750559,0.040586304077064,
0.616608004950626));
#11803=CARTESIAN_POINT('Ctrl Pts',(-0.149520700253385,0.0428934515853061,
0.616438959710814));
#11804=CARTESIAN_POINT('Ctrl Pts',(-0.149327065559149,0.0435627760385117,
0.616389680669495));
#11805=CARTESIAN_POINT('Ctrl Pts',(-0.149005902063342,0.0446456144275852,
0.616309561045339));
#11806=CARTESIAN_POINT('Ctrl Pts',(-0.148881131480382,0.0450599425159485,
0.616278810453712));
#11807=CARTESIAN_POINT('Ctrl Pts',(-0.148616973300796,0.0459240621782781,
0.616214477289995));
#11808=CARTESIAN_POINT('Ctrl Pts',(-0.148477268975909,0.046373751503711,
0.616180884657429));
#11809=CARTESIAN_POINT('Ctrl Pts',(-0.148141258858153,0.0474382380989754,
0.616101092214698));
#11810=CARTESIAN_POINT('Ctrl Pts',(-0.1479431658435,0.0480524574497901,
0.61605483428233));
#11811=CARTESIAN_POINT('Ctrl Pts',(-0.147268845329349,0.0500995982376279,
0.615899922479334));
#11812=CARTESIAN_POINT('Ctrl Pts',(-0.146775589642696,0.0515267749263192,
0.615790711473049));
#11813=CARTESIAN_POINT('Ctrl Pts',(-0.144022803320651,0.0591311884418498,
0.615202078251652));
#11814=CARTESIAN_POINT('Ctrl Pts',(-0.141394268527936,0.0651667365848729,
0.614710512034069));
#11815=CARTESIAN_POINT('Ctrl Pts',(-0.133806050313894,0.0799540043047982,
0.613443751824431));
#11816=CARTESIAN_POINT('Ctrl Pts',(-0.12836520930498,0.0884254022824461,
0.612657426108371));
#11817=CARTESIAN_POINT('Ctrl Pts',(-0.120926640201696,0.0978592414262875,
0.61173390126183));
#11818=CARTESIAN_POINT('Ctrl Pts',(-0.11967754293255,0.0993829446681807,
0.611583163824499));
#11819=CARTESIAN_POINT('Ctrl Pts',(-0.117510817061786,0.101925900652144,
0.611329370879208));
#11820=CARTESIAN_POINT('Ctrl Pts',(-0.116608054918576,0.102957482120815,
0.611225772688831));
#11821=CARTESIAN_POINT('Ctrl Pts',(-0.114103164856635,0.105744589132956,
0.610944379228456));
#11822=CARTESIAN_POINT('Ctrl Pts',(-0.112474164039244,0.107475645877367,
0.610767943271088));
#11823=CARTESIAN_POINT('Ctrl Pts',(-0.110456489777317,0.109523579167342,
0.610557860882373));
#11824=CARTESIAN_POINT('Ctrl Pts',(-0.110105256347507,0.109876672093618,
0.610521589758884));
#11825=CARTESIAN_POINT('Ctrl Pts',(-0.109525097647989,0.110454326789766,
0.610462177472418));
#11826=CARTESIAN_POINT('Ctrl Pts',(-0.109297166699943,0.110679874764104,
0.610438961102276));
#11827=CARTESIAN_POINT('Ctrl Pts',(-0.108884959714948,0.111085257088982,
0.610397202943737));
#11828=CARTESIAN_POINT('Ctrl Pts',(-0.108700934457395,0.111265338924405,
0.610378641961056));
#11829=CARTESIAN_POINT('Ctrl Pts',(-0.108298097466243,0.111657590315717,
0.610338189005064));
#11830=CARTESIAN_POINT('Ctrl Pts',(-0.108079109647944,0.111869573396744,
0.610316311532879));
#11831=CARTESIAN_POINT('Ctrl Pts',(-0.107457153254402,0.112468104420445,
0.61025449140292));
#11832=CARTESIAN_POINT('Ctrl Pts',(-0.107052718689288,0.112853133515076,
0.610214664377523));
#11833=CARTESIAN_POINT('Ctrl Pts',(-0.104513542140358,0.115244542576148,
0.609966861853852));
#11834=CARTESIAN_POINT('Ctrl Pts',(-0.102324367148768,0.117192627600569,
0.609763056576974));
#11835=CARTESIAN_POINT('Ctrl Pts',(-0.0890659403496413,0.128335926790838,
0.608576120101917));
#11836=CARTESIAN_POINT('Ctrl Pts',(-0.0768187175676357,0.136021354216421,
0.607662411453918));
#11837=CARTESIAN_POINT('Ctrl Pts',(-0.0636886258321226,0.141913922641918,
0.606695238001095));
#11838=CARTESIAN_POINT('',(-0.155549956956732,1.69517297940555E-6,0.605448024839579));
#11839=CARTESIAN_POINT('Ctrl Pts',(-0.0636886259076389,0.141913922608026,
0.592717731153444));
#11840=CARTESIAN_POINT('Ctrl Pts',(-0.0645421680723216,0.141530866973851,
0.592780255107091));
#11841=CARTESIAN_POINT('Ctrl Pts',(-0.06539250273425,0.141139999457564,
0.592842952041328));
#11842=CARTESIAN_POINT('Ctrl Pts',(-0.071439591683574,0.138293954046624,
0.593291964667332));
#11843=CARTESIAN_POINT('Ctrl Pts',(-0.0764994376252857,0.135560526283284,
0.593684591834827));
#11844=CARTESIAN_POINT('Ctrl Pts',(-0.0822897660030893,0.132004912109664,
0.594160907074483));
#11845=CARTESIAN_POINT('Ctrl Pts',(-0.083177890784753,0.131447102664529,
0.594234742969407));
#11846=CARTESIAN_POINT('Ctrl Pts',(-0.0845290725455758,0.130579281686744,
0.594348309736595));
#11847=CARTESIAN_POINT('Ctrl Pts',(-0.084996230379702,0.130275683524707,
0.594387803158546));
#11848=CARTESIAN_POINT('Ctrl Pts',(-0.0858254862657522,0.129730404782106,
0.594458322638973));
#11849=CARTESIAN_POINT('Ctrl Pts',(-0.0861882217733486,0.129489700123871,
0.594489311994601));
#11850=CARTESIAN_POINT('Ctrl Pts',(-0.0865582548510905,0.129241909291469,
0.594521072341359));
#11851=CARTESIAN_POINT('Ctrl Pts',(-0.0865665704554396,0.129236339625331,
0.594521786155287));
#11852=CARTESIAN_POINT('Ctrl Pts',(-0.0865815823983888,0.129226282753808,
0.594523074922943));
#11853=CARTESIAN_POINT('Ctrl Pts',(-0.086588278926626,0.129221795829886,
0.594523649866084));
#11854=CARTESIAN_POINT('Ctrl Pts',(-0.0866004540151363,0.129213636694708,
0.594524695271622));
#11855=CARTESIAN_POINT('Ctrl Pts',(-0.0866059326907217,0.129209964655478,
0.594525165727521));
#11856=CARTESIAN_POINT('Ctrl Pts',(-0.0866200706884921,0.129200487470459,
0.594526379848355));
#11857=CARTESIAN_POINT('Ctrl Pts',(-0.0866287296598549,0.129194681803096,
0.594527123532947));
#11858=CARTESIAN_POINT('Ctrl Pts',(-0.0866457235385286,0.129183285270245,
0.594528583232527));
#11859=CARTESIAN_POINT('Ctrl Pts',(-0.086654058488704,0.129177694468374,
0.594529299245118));
#11860=CARTESIAN_POINT('Ctrl Pts',(-0.0866704443701546,0.129166701075337,
0.594530707023049));
#11861=CARTESIAN_POINT('Ctrl Pts',(-0.0866784953374954,0.129161298538042,
0.594531398786348));
#11862=CARTESIAN_POINT('Ctrl Pts',(-0.0866943476260553,0.129150658836807,
0.594532761004112));
#11863=CARTESIAN_POINT('Ctrl Pts',(-0.0867021489779531,0.129145421718671,
0.594533431456842));
#11864=CARTESIAN_POINT('Ctrl Pts',(-0.0867175318159114,0.129135093058236,
0.594534753600041));
#11865=CARTESIAN_POINT('Ctrl Pts',(-0.0867251133285815,0.129130001554818,
0.59453540528906));
#11866=CARTESIAN_POINT('Ctrl Pts',(-0.0867400825157907,0.129119946810574,
0.594536692131201));
#11867=CARTESIAN_POINT('Ctrl Pts',(-0.086747470212533,0.12911498360352,
0.594537327283026));
#11868=CARTESIAN_POINT('Ctrl Pts',(-0.0867620746966495,0.129105170190584,
0.594538583012691));
#11869=CARTESIAN_POINT('Ctrl Pts',(-0.0867692915036335,0.129100320013406,
0.59453920358946));
#11870=CARTESIAN_POINT('Ctrl Pts',(-0.0867835745623629,0.129090719103583,
0.594540431911215));
#11871=CARTESIAN_POINT('Ctrl Pts',(-0.0867906408311332,0.129085968395572,
0.594541039655289));
#11872=CARTESIAN_POINT('Ctrl Pts',(-0.0868046410138762,0.129076554293483,
0.594542243870061));
#11873=CARTESIAN_POINT('Ctrl Pts',(-0.0868115749418122,0.129071890921101,
0.594542840339913));
#11874=CARTESIAN_POINT('Ctrl Pts',(-0.0868253268241844,0.129062640564179,
0.594544023409412));
#11875=CARTESIAN_POINT('Ctrl Pts',(-0.0868321447919833,0.129058053597398,
0.594544610008447));
#11876=CARTESIAN_POINT('Ctrl Pts',(-0.0868456796034278,0.129048946139709,
0.594545774608762));
#11877=CARTESIAN_POINT('Ctrl Pts',(-0.0868523964570442,0.129044425665037,
0.594546352609389));
#11878=CARTESIAN_POINT('Ctrl Pts',(-0.0868657425806166,0.129035442145885,
0.594547501173671));
#11879=CARTESIAN_POINT('Ctrl Pts',(-0.0868723718592643,0.12903097911514,
0.594548071736783));
#11880=CARTESIAN_POINT('Ctrl Pts',(-0.0868855552573491,0.12902210217657,
0.594549206491615));
#11881=CARTESIAN_POINT('Ctrl Pts',(-0.0868921093849075,0.129017688279865,
0.59454977068294));
#11882=CARTESIAN_POINT('Ctrl Pts',(-0.0869051539532847,0.129008901931611,
0.594550893678592));
#11883=CARTESIAN_POINT('Ctrl Pts',(-0.0869116444004273,0.129004529489696,
0.594551452482547));
#11884=CARTESIAN_POINT('Ctrl Pts',(-0.0869245722610375,0.128995818914783,
0.594552565617997));
#11885=CARTESIAN_POINT('Ctrl Pts',(-0.0869310096799614,0.128991480789555,
0.594553119949207));
#11886=CARTESIAN_POINT('Ctrl Pts',(-0.0874011603812284,0.128674598805235,
0.59459360837186));
#11887=CARTESIAN_POINT('Ctrl Pts',(-0.087863179528361,0.128359560928423,
0.594633636409742));
#11888=CARTESIAN_POINT('Ctrl Pts',(-0.0892459848900351,0.127405700887843,
0.594754169434339));
#11889=CARTESIAN_POINT('Ctrl Pts',(-0.0901615584427469,0.126759424480668,
0.594834956732482));
#11890=CARTESIAN_POINT('Ctrl Pts',(-0.0991541728784745,0.120265084962037,
0.595638380511613));
#11891=CARTESIAN_POINT('Ctrl Pts',(-0.106656456765969,0.11366426583745,
0.59639113301573));
#11892=CARTESIAN_POINT('Ctrl Pts',(-0.12184721546711,0.097462354411212,
0.598104197824594));
#11893=CARTESIAN_POINT('Ctrl Pts',(-0.129137025742495,0.0875746634344515,
0.599067737899218));
#11894=CARTESIAN_POINT('Ctrl Pts',(-0.135698187044565,0.0760450565832941,
0.600046258588611));
#11895=CARTESIAN_POINT('Ctrl Pts',(-0.136195290257886,0.0751511254689562,
0.600121232097949));
#11896=CARTESIAN_POINT('Ctrl Pts',(-0.136875068465791,0.0738997908593797,
0.600224875334224));
#11897=CARTESIAN_POINT('Ctrl Pts',(-0.137065218072634,0.0735465122287305,
0.600253992554515));
#11898=CARTESIAN_POINT('Ctrl Pts',(-0.137368440603421,0.0729778951207177,
0.600300623244457));
#11899=CARTESIAN_POINT('Ctrl Pts',(-0.137482377253485,0.0727630235561555,
0.600318190667547));
#11900=CARTESIAN_POINT('Ctrl Pts',(-0.137719445165092,0.0723133956714605,
0.600354838007231));
#11901=CARTESIAN_POINT('Ctrl Pts',(-0.137842480726941,0.0720785909876796,
0.600373911528016));
#11902=CARTESIAN_POINT('Ctrl Pts',(-0.138138764495207,0.0715096211907438,
0.600419976686285));
#11903=CARTESIAN_POINT('Ctrl Pts',(-0.138311402800424,0.0711751364067545,
0.60044693005095));
#11904=CARTESIAN_POINT('Ctrl Pts',(-0.138911504267425,0.070002017823152,
0.60054102882373));
#11905=CARTESIAN_POINT('Ctrl Pts',(-0.139332579561854,0.0691601106604629,
0.600607787988364));
#11906=CARTESIAN_POINT('Ctrl Pts',(-0.141771901241083,0.0641701609473671,
0.600999240119817));
#11907=CARTESIAN_POINT('Ctrl Pts',(-0.143612686445219,0.059937363228163,
0.601314192319064));
#11908=CARTESIAN_POINT('Ctrl Pts',(-0.149088721203819,0.0456377976915111,
0.602342702975756));
#11909=CARTESIAN_POINT('Ctrl Pts',(-0.151873915082035,0.0352787489918909,
0.603033133129283));
#11910=CARTESIAN_POINT('Ctrl Pts',(-0.15461481200792,0.0182476766811929,
0.604183449687493));
#11911=CARTESIAN_POINT('Ctrl Pts',(-0.155245963313012,0.0117214143171901,
0.604627295046638));
#11912=CARTESIAN_POINT('Ctrl Pts',(-0.15550216665472,0.00402527617589184,
0.605164580373047));
#11913=CARTESIAN_POINT('Ctrl Pts',(-0.155527688746032,0.00287482029818528,
0.60524524757909));
#11914=CARTESIAN_POINT('Ctrl Pts',(-0.155546808207301,0.00115006330512711,
0.605366757610222));
#11915=CARTESIAN_POINT('Ctrl Pts',(-0.155549993637752,0.00057589038162694,
0.60540730368657));
#11916=CARTESIAN_POINT('Ctrl Pts',(-0.155549999990479,1.72103705376068E-6,
0.605447948317266));
#11917=CARTESIAN_POINT('Ctrl Pts',(-0.15554999999082,1.68991234156361E-6,
0.60544795052054));
#11918=CARTESIAN_POINT('Ctrl Pts',(-0.15555000269116,-0.000246866046467027,
0.605465545444643));
#11919=CARTESIAN_POINT('Ctrl Pts',(-0.155549409633897,-0.000495420636813976,
0.605483158784546));
#11920=CARTESIAN_POINT('Ctrl Pts',(-0.155546180294664,-0.00117060485290016,
0.605531055424233));
#11921=CARTESIAN_POINT('Ctrl Pts',(-0.155542384543066,-0.00159722384704611,
0.605561374528306));
#11922=CARTESIAN_POINT('Ctrl Pts',(-0.155530851940917,-0.00248354092000977,
0.605624481252254));
#11923=CARTESIAN_POINT('Ctrl Pts',(-0.155522831979431,-0.00294323049001169,
0.605657277404107));
#11924=CARTESIAN_POINT('Ctrl Pts',(-0.155499307288224,-0.00401831901967739,
0.6057341359501));
#11925=CARTESIAN_POINT('Ctrl Pts',(-0.155482187168788,-0.00463367110368875,
0.605778248329937));
#11926=CARTESIAN_POINT('Ctrl Pts',(-0.155416544985987,-0.00657785597660333,
0.605918011214128));
#11927=CARTESIAN_POINT('Ctrl Pts',(-0.155354637239221,-0.00790614499603027,
0.606014077205768));
#11928=CARTESIAN_POINT('Ctrl Pts',(-0.1551945530319,-0.0105982283447777,
0.606210003052721));
#11929=CARTESIAN_POINT('Ctrl Pts',(-0.155095408538991,-0.0119618462158238,
0.60630988477302));
#11930=CARTESIAN_POINT('Ctrl Pts',(-0.154643381828647,-0.0172196250270301,
0.606697545663322));
#11931=CARTESIAN_POINT('Ctrl Pts',(-0.154161718860842,-0.0211009642599832,
0.606989160605566));
#11932=CARTESIAN_POINT('Ctrl Pts',(-0.151181792927924,-0.0394313218854205,
0.608392180677955));
#11933=CARTESIAN_POINT('Ctrl Pts',(-0.146795550196754,-0.0534953471628895,
0.609554571603185));
#11934=CARTESIAN_POINT('Ctrl Pts',(-0.139366153735788,-0.0691371137296447,
0.610858094242812));
#11935=CARTESIAN_POINT('Ctrl Pts',(-0.138164521207684,-0.0715082700154811,
0.611055721580055));
#11936=CARTESIAN_POINT('Ctrl Pts',(-0.136644786718346,-0.0743256329052478,
0.611289588245654));
#11937=CARTESIAN_POINT('Ctrl Pts',(-0.136384448237238,-0.0748022709999217,
0.611329119918695));
#11938=CARTESIAN_POINT('Ctrl Pts',(-0.135975751214151,-0.0755413027792245,
0.611390350450682));
#11939=CARTESIAN_POINT('Ctrl Pts',(-0.13582912088118,-0.0758046388336279,
0.611412155813021));
#11940=CARTESIAN_POINT('Ctrl Pts',(-0.13555573156068,-0.0762922834914956,
0.611452509069153));
#11941=CARTESIAN_POINT('Ctrl Pts',(-0.135429181920111,-0.0765167012204078,
0.611471069481943));
#11942=CARTESIAN_POINT('Ctrl Pts',(-0.13514188300577,-0.0770232392531501,
0.611512939857842));
#11943=CARTESIAN_POINT('Ctrl Pts',(-0.134980807949059,-0.0773051707069598,
0.611536228572002));
#11944=CARTESIAN_POINT('Ctrl Pts',(-0.134503023709644,-0.0781353955398286,
0.611604768540353));
#11945=CARTESIAN_POINT('Ctrl Pts',(-0.134183842933698,-0.078682270909785,
0.611649864596857));
#11946=CARTESIAN_POINT('Ctrl Pts',(-0.131862372778803,-0.0826045992384129,
0.611973046242618));
#11947=CARTESIAN_POINT('Ctrl Pts',(-0.129736096224094,-0.0859055128545022,
0.612243649193784));
#11948=CARTESIAN_POINT('Ctrl Pts',(-0.12676314900073,-0.0901582087722229,
0.612595392087857));
#11949=CARTESIAN_POINT('Ctrl Pts',(-0.126026704905546,-0.0911848032890401,
0.612680551745414));
#11950=CARTESIAN_POINT('Ctrl Pts',(-0.119166425518087,-0.100506051418135,
0.613457201707674));
#11951=CARTESIAN_POINT('Ctrl Pts',(-0.112244448397571,-0.108181816691158,
0.614123508150869));
#11952=CARTESIAN_POINT('Ctrl Pts',(-0.100972321942327,-0.118425509933041,
0.615137940013221));
#11953=CARTESIAN_POINT('Ctrl Pts',(-0.0971763914055755,-0.121559670309547,
0.6154693778377));
#11954=CARTESIAN_POINT('Ctrl Pts',(-0.0909275861478394,-0.126239107451906,
0.616005942718959));
#11955=CARTESIAN_POINT('Ctrl Pts',(-0.0885689952328414,-0.127904923240541,
0.616206547746189));
#11956=CARTESIAN_POINT('Ctrl Pts',(-0.0856597052565283,-0.129840619772417,
0.616452408325497));
#11957=CARTESIAN_POINT('Ctrl Pts',(-0.0851519040148387,-0.130174209701628,
0.616495264475898));
#11958=CARTESIAN_POINT('Ctrl Pts',(-0.0842566150031015,-0.130754871837227,
0.616570729711796));
#11959=CARTESIAN_POINT('Ctrl Pts',(-0.0838699597391991,-0.131003219525641,
0.616603291222935));
#11960=CARTESIAN_POINT('Ctrl Pts',(-0.083094567585844,-0.131496412121985,
0.616668532658772));
#11961=CARTESIAN_POINT('Ctrl Pts',(-0.082705835195802,-0.131741255419529,
0.616701212219627));
#11962=CARTESIAN_POINT('Ctrl Pts',(-0.0819467749141003,-0.132214666224297,
0.616764972139161));
#11963=CARTESIAN_POINT('Ctrl Pts',(-0.081576560870931,-0.13244340902062,
0.616796045667784));
#11964=CARTESIAN_POINT('Ctrl Pts',(-0.0806205312927279,-0.13302857833316,
0.616876230805559));
#11965=CARTESIAN_POINT('Ctrl Pts',(-0.0800333153543437,-0.133382686750331,
0.616925426476372));
#11966=CARTESIAN_POINT('Ctrl Pts',(-0.0779710051651543,-0.134607798404192,
0.617098022535319));
#11967=CARTESIAN_POINT('Ctrl Pts',(-0.0764839294410919,-0.135458278221593,
0.617222159068087));
#11968=CARTESIAN_POINT('Ctrl Pts',(-0.0641464353693927,-0.142246341310883,
0.61824988006041));
#11969=CARTESIAN_POINT('Ctrl Pts',(-0.052639496067444,-0.146893639503891,
0.619200111178757));
#11970=CARTESIAN_POINT('Ctrl Pts',(-0.0360660659531262,-0.151387456761871,
0.620531846263102));
#11971=CARTESIAN_POINT('Ctrl Pts',(-0.0313692226170196,-0.152429978537289,
0.620904672542681));
#11972=CARTESIAN_POINT('Ctrl Pts',(-0.0234788234335609,-0.153801127306779,
0.621517469190521));
#11973=CARTESIAN_POINT('Ctrl Pts',(-0.0203097676359398,-0.154251606995086,
0.621759995265127));
#11974=CARTESIAN_POINT('Ctrl Pts',(-0.0159568541404281,-0.154733873944736,
0.622086414105963));
#11975=CARTESIAN_POINT('Ctrl Pts',(-0.0147833729024979,-0.154850395653898,
0.622173747161028));
#11976=CARTESIAN_POINT('Ctrl Pts',(-0.0127660483161376,-0.155027565103629,
0.622322617529598));
#11977=CARTESIAN_POINT('Ctrl Pts',(-0.0119228444483672,-0.155094693004722,
0.622384464417819));
#11978=CARTESIAN_POINT('Ctrl Pts',(-0.0107195098600563,-0.15518061921468,
0.62247214820256));
#11979=CARTESIAN_POINT('Ctrl Pts',(-0.0103598167694378,-0.155205047195995,
0.622498284529464));
#11980=CARTESIAN_POINT('Ctrl Pts',(-0.0097383726893711,-0.155245081563896,
0.622543309724848));
#11981=CARTESIAN_POINT('Ctrl Pts',(-0.00947666267635023,-0.155261276953991,
0.622562231208876));
#11982=CARTESIAN_POINT('Ctrl Pts',(-0.00896813589807324,-0.155291455493855,
0.622598918283943));
#11983=CARTESIAN_POINT('Ctrl Pts',(-0.00872132697857542,-0.155305512036626,
0.622616688046706));
#11984=CARTESIAN_POINT('Ctrl Pts',(-0.00805333736016125,-0.155341958753017,
0.622664687214997));
#11985=CARTESIAN_POINT('Ctrl Pts',(-0.00763209313398832,-0.15536322459792,
0.622694854263577));
#11986=CARTESIAN_POINT('Ctrl Pts',(-0.0060571073442633,-0.155436314076149,
0.622807282176867));
#11987=CARTESIAN_POINT('Ctrl Pts',(-0.00490284763192702,-0.15547700337552,
0.622888948610456));
#11988=CARTESIAN_POINT('Ctrl Pts',(0.0072041728738317,-0.15576882384188,
0.623738926678597));
#11989=CARTESIAN_POINT('Ctrl Pts',(0.0181556956324896,-0.154875040171725,
0.624452376272599));
#11990=CARTESIAN_POINT('Ctrl Pts',(0.0387287316436798,-0.150981679344767,
0.625831087940597));
#11991=CARTESIAN_POINT('Ctrl Pts',(0.0483309570722019,-0.148187251400893,
0.626492121962202));
#11992=CARTESIAN_POINT('Ctrl Pts',(0.0593417735998711,-0.143798043556098,
0.627315016725813));
#11993=CARTESIAN_POINT('Ctrl Pts',(0.0610720186803714,-0.143071770194556,
0.627446258026023));
#11994=CARTESIAN_POINT('Ctrl Pts',(0.0632775987228548,-0.142098675642065,
0.627616237449259));
#11995=CARTESIAN_POINT('Ctrl Pts',(0.0637654373707554,-0.141880432419188,
0.627654004726327));
#11996=CARTESIAN_POINT('Ctrl Pts',(0.0647151513481073,-0.141449673638688,
0.62772786833199));
#11997=CARTESIAN_POINT('Ctrl Pts',(0.0651771290020639,-0.141237398837473,
0.627763956078891));
#11998=CARTESIAN_POINT('Ctrl Pts',(0.0660456204977071,-0.140833165875177,
0.627832100821028));
#11999=CARTESIAN_POINT('Ctrl Pts',(0.0664523600041686,-0.140641702348329,
0.627864140498651));
#12000=CARTESIAN_POINT('Ctrl Pts',(0.0673772326442361,-0.140201431472514,
0.627937284387844));
#12001=CARTESIAN_POINT('Ctrl Pts',(0.0678948255296149,-0.139951511301741,
0.627978426791504));
#12002=CARTESIAN_POINT('Ctrl Pts',(0.0693780426016128,-0.139225174101158,
0.628096932716961));
#12003=CARTESIAN_POINT('Ctrl Pts',(0.0703401037478813,-0.138741600088303,
0.628174544275768));
#12004=CARTESIAN_POINT('Ctrl Pts',(0.0770090342113652,-0.135302311771293,
0.628717861141329));
#12005=CARTESIAN_POINT('Ctrl Pts',(0.082532122390359,-0.132005810682738,
0.629195563973366));
#12006=CARTESIAN_POINT('Ctrl Pts',(0.0996490245700216,-0.120294574061155,
0.630769478042835));
#12007=CARTESIAN_POINT('Ctrl Pts',(0.110289499669239,-0.110620468326615,
0.631904303893878));
#12008=CARTESIAN_POINT('Ctrl Pts',(0.12092907832483,-0.0978633959929492,
0.633150063928951));
#12009=CARTESIAN_POINT('Ctrl Pts',(0.122362141603887,-0.0960655718432342,
0.633320516656308));
#12010=CARTESIAN_POINT('Ctrl Pts',(0.124069915037214,-0.0938228597556935,
0.63352634502795));
#12011=CARTESIAN_POINT('Ctrl Pts',(0.124382834881437,-0.0934076187350562,
0.633564175279617));
#12012=CARTESIAN_POINT('Ctrl Pts',(0.124870825867942,-0.0927532595643639,
0.633623343633234));
#12013=CARTESIAN_POINT('Ctrl Pts',(0.125047301839897,-0.0925152020985207,
0.633644777172721));
#12014=CARTESIAN_POINT('Ctrl Pts',(0.125376301016954,-0.0920687370261534,
0.63368480058021));
#12015=CARTESIAN_POINT('Ctrl Pts',(0.125528983744005,-0.0918604563240144,
0.633703401130076));
#12016=CARTESIAN_POINT('Ctrl Pts',(0.125876725061937,-0.0913836022620748,
0.63374582645333));
#12017=CARTESIAN_POINT('Ctrl Pts',(0.126071442956404,-0.0911147844818143,
0.633769627593949));
#12018=CARTESIAN_POINT('Ctrl Pts',(0.126668560435871,-0.0902848551013026,
0.633842762147437));
#12019=CARTESIAN_POINT('Ctrl Pts',(0.127068093109419,-0.089721675332436,
0.633891903386442));
#12020=CARTESIAN_POINT('Ctrl Pts',(0.132495237580992,-0.0819626227478519,
0.634562570956439));
#12021=CARTESIAN_POINT('Ctrl Pts',(0.136909582294586,-0.0743550885261985,
0.63514593798261));
#12022=CARTESIAN_POINT('Ctrl Pts',(0.144078785040856,-0.0591714727061843,
0.636253396297089));
#12023=CARTESIAN_POINT('Ctrl Pts',(0.146934007696836,-0.0516754351668931,
0.63677669614464));
#12024=CARTESIAN_POINT('Ctrl Pts',(0.150336621149422,-0.0401357114992056,
0.637583784302255));
#12025=CARTESIAN_POINT('Ctrl Pts',(0.151323898543774,-0.0362360131282377,
0.637856638393564));
#12026=CARTESIAN_POINT('Ctrl Pts',(0.152678077918459,-0.0298572696393413,
0.638306468207153));
#12027=CARTESIAN_POINT('Ctrl Pts',(0.153138172830518,-0.027399832463768,
0.638480586071073));
#12028=CARTESIAN_POINT('Ctrl Pts',(0.153664486387855,-0.0241586976034388,
0.638711774762485));
#12029=CARTESIAN_POINT('Ctrl Pts',(0.153784285989732,-0.0233839771845434,
0.638767149506014));
#12030=CARTESIAN_POINT('Ctrl Pts',(0.153970791512132,-0.0221144104595091,
0.638858095843171));
#12031=CARTESIAN_POINT('Ctrl Pts',(0.154040980901334,-0.0216200828213467,
0.638893557207049));
#12032=CARTESIAN_POINT('Ctrl Pts',(0.154172157427217,-0.020663157708806,
0.638962304098659));
#12033=CARTESIAN_POINT('Ctrl Pts',(0.15423344549532,-0.0202006062824941,
0.638995579750602));
#12034=CARTESIAN_POINT('Ctrl Pts',(0.154370034304574,-0.0191328753607649,
0.639072499629973));
#12035=CARTESIAN_POINT('Ctrl Pts',(0.154443858595634,-0.018527518270096,
0.639116189806916));
#12036=CARTESIAN_POINT('Ctrl Pts',(0.154632568422074,-0.0169005381023726,
0.639233836117936));
#12037=CARTESIAN_POINT('Ctrl Pts',(0.154740886905871,-0.0158781998400958,
0.639307996951977));
#12038=CARTESIAN_POINT('Ctrl Pts',(0.155905784530694,-0.00373595508885958,
0.640191745011383));
#12039=CARTESIAN_POINT('Ctrl Pts',(0.155771534038834,0.00746302211110987,
0.641039755092854));
#12040=CARTESIAN_POINT('Ctrl Pts',(0.153955256975544,0.0225856981260099,
0.642218384041977));
#12041=CARTESIAN_POINT('Ctrl Pts',(0.153312303551222,0.0266021113264362,
0.64253428099494));
#12042=CARTESIAN_POINT('Ctrl Pts',(0.151094189137307,0.0376614446459579,
0.643407165187042));
#12043=CARTESIAN_POINT('Ctrl Pts',(0.149185165957373,0.0446279338210357,
0.643960757063796));
#12044=CARTESIAN_POINT('Ctrl Pts',(0.146520772639784,0.0522319274084485,
0.644553027592142));
#12045=CARTESIAN_POINT('Ctrl Pts',(0.146235966693505,0.0530240811911721,
0.644614573337361));
#12046=CARTESIAN_POINT('Ctrl Pts',(0.145820256044093,0.0541514994325331,
0.644701907512446));
#12047=CARTESIAN_POINT('Ctrl Pts',(0.145694603734264,0.0544886631635209,
0.6447279921791));
#12048=CARTESIAN_POINT('Ctrl Pts',(0.145475405058326,0.0550706610921606,
0.64477295707184));
#12049=CARTESIAN_POINT('Ctrl Pts',(0.145382408268418,0.0553156990422736,
0.644791869676017));
#12050=CARTESIAN_POINT('Ctrl Pts',(0.14520041924754,0.0557915940060938,
0.644828562288324));
#12051=CARTESIAN_POINT('Ctrl Pts',(0.145111495669539,0.0560224735110557,
0.644846346378823));
#12052=CARTESIAN_POINT('Ctrl Pts',(0.14486911791217,0.056647329489976,0.644894433311514));
#12053=CARTESIAN_POINT('Ctrl Pts',(0.144714606110117,0.0570408980704138,
0.644924673391923));
#12054=CARTESIAN_POINT('Ctrl Pts',(0.144129614889571,0.0585132957016289,
0.645037644724764));
#12055=CARTESIAN_POINT('Ctrl Pts',(0.143688646228143,0.0595879586938149,
0.645119774198944));
#12056=CARTESIAN_POINT('Ctrl Pts',(0.139833568364228,0.0686912602035709,
0.645813539009813));
#12057=CARTESIAN_POINT('Ctrl Pts',(0.13576107391466,0.0764257411053781,
0.64639053895324));
#12058=CARTESIAN_POINT('Ctrl Pts',(0.126061897274138,0.0915988074250569,
0.647576828755047));
#12059=CARTESIAN_POINT('Ctrl Pts',(0.120373612641557,0.0989551429633502,
0.648184012387952));
#12060=CARTESIAN_POINT('Ctrl Pts',(0.111126181632568,0.108928608662527,
0.649107596055885));
#12061=CARTESIAN_POINT('Ctrl Pts',(0.108058091947769,0.111972822201948,
0.649405317010247));
#12062=CARTESIAN_POINT('Ctrl Pts',(0.104173958406753,0.115518270006524,
0.64977466579892));
#12063=CARTESIAN_POINT('Ctrl Pts',(0.103474695562522,0.11614504563118,0.649840874181854));
#12064=CARTESIAN_POINT('Ctrl Pts',(0.102369298586383,0.117117948591452,
0.649945117115342));
#12065=CARTESIAN_POINT('Ctrl Pts',(0.101966976729068,0.11746839072352,0.649982971807506));
#12066=CARTESIAN_POINT('Ctrl Pts',(0.101249585405843,0.118086811418107,
0.650050324697209));
#12067=CARTESIAN_POINT('Ctrl Pts',(0.100935233331135,0.11835561770392,0.650079788402867));
#12068=CARTESIAN_POINT('Ctrl Pts',(0.100207337834258,0.118973041045461,
0.650147901580778));
#12069=CARTESIAN_POINT('Ctrl Pts',(0.0997930428047233,0.119320759491201,
0.650186587267329));
#12070=CARTESIAN_POINT('Ctrl Pts',(0.0986488259489147,0.120270974986987,
0.650293212268211));
#12071=CARTESIAN_POINT('Ctrl Pts',(0.0979152161774744,0.120868973077282,
0.650361332083289));
#12072=CARTESIAN_POINT('Ctrl Pts',(0.094105730667767,0.123916813277471,
0.650713878246627));
#12073=CARTESIAN_POINT('Ctrl Pts',(0.0909434855293611,0.126255860982809,
0.651002636668619));
#12074=CARTESIAN_POINT('Ctrl Pts',(0.086058565355115,0.129590345660602,
0.651443508412847));
#12075=CARTESIAN_POINT('Ctrl Pts',(0.0843996863067313,0.130676802528019,
0.65159235915422));
#12076=CARTESIAN_POINT('Ctrl Pts',(0.0703149981521815,0.139521275882966,
0.652848801711777));
#12077=CARTESIAN_POINT('Ctrl Pts',(0.0568732990107603,0.145518848342843,
0.654010097842982));
#12078=CARTESIAN_POINT('Ctrl Pts',(0.0402215194448914,0.150283674043558,
0.65531410674233));
#12079=CARTESIAN_POINT('Ctrl Pts',(0.0376318420634051,0.150952973182189,
0.655512986768204));
#12080=CARTESIAN_POINT('Ctrl Pts',(0.0344959019302548,0.151677721677948,
0.655748136363642));
#12081=CARTESIAN_POINT('Ctrl Pts',(0.0339651626271346,0.151797451411035,
0.655787739653547));
#12082=CARTESIAN_POINT('Ctrl Pts',(0.0331392298437318,0.151979225281166,
0.655849056870482));
#12083=CARTESIAN_POINT('Ctrl Pts',(0.0328444728524854,0.152043198068726,
0.655870877777938));
#12084=CARTESIAN_POINT('Ctrl Pts',(0.0322976091319414,0.152160222508194,
0.65591124527159));
#12085=CARTESIAN_POINT('Ctrl Pts',(0.0320455590713309,0.152213504706742,
0.655929804452719));
#12086=CARTESIAN_POINT('Ctrl Pts',(0.0314758044893956,0.152332470200553,
0.655971653661496));
#12087=CARTESIAN_POINT('Ctrl Pts',(0.0311580268202946,0.152397785796019,
0.655994922532799));
#12088=CARTESIAN_POINT('Ctrl Pts',(0.0302207039556695,0.152587387514851,
0.656063350141667));
#12089=CARTESIAN_POINT('Ctrl Pts',(0.0296005929177064,0.152708895325904,
0.656108354439541));
#12090=CARTESIAN_POINT('Ctrl Pts',(0.0251568271563583,0.153551544291862,
0.656429072115368));
#12091=CARTESIAN_POINT('Ctrl Pts',(0.0213076378996552,0.154132844498649,
0.656697432037));
#12092=CARTESIAN_POINT('Ctrl Pts',(0.0162346410105878,0.154705239273233,
0.65704361564081));
#12093=CARTESIAN_POINT('Ctrl Pts',(0.0150274012392898,0.154827168063572,
0.657125444389107));
#12094=CARTESIAN_POINT('Ctrl Pts',(-0.000984437347845478,0.156255282855507,
0.658204853940127));
#12095=CARTESIAN_POINT('Ctrl Pts',(-0.0159000904905725,0.155447415966817,
0.659151709054206));
#12096=CARTESIAN_POINT('Ctrl Pts',(-0.0336969953422569,0.151891771155205,
0.660394642152622));
#12097=CARTESIAN_POINT('Ctrl Pts',(-0.0368974923166192,0.151146187488856,
0.660622387523984));
#12098=CARTESIAN_POINT('Ctrl Pts',(-0.0409048996753446,0.150077763450468,
0.660914015232223));
#12099=CARTESIAN_POINT('Ctrl Pts',(-0.0417361283034552,0.149848728524489,
0.660974859388766));
#12100=CARTESIAN_POINT('Ctrl Pts',(-0.0430622885310259,0.149471431030984,
0.66107251787399));
#12101=CARTESIAN_POINT('Ctrl Pts',(-0.0435584690630845,0.14932759004664,
0.661109188559251));
#12102=CARTESIAN_POINT('Ctrl Pts',(-0.0444968367759962,0.149050485746035,
0.661178794136787));
#12103=CARTESIAN_POINT('Ctrl Pts',(-0.0449391659758202,0.148917719352486,
0.661211712522855));
#12104=CARTESIAN_POINT('Ctrl Pts',(-0.045940356248095,0.148612342308135,
0.661286469325993));
#12105=CARTESIAN_POINT('Ctrl Pts',(-0.046498845344745,0.148438546149006,
0.661328346080184));
#12106=CARTESIAN_POINT('Ctrl Pts',(-0.0481480985568903,0.147915094314029,
0.661452539222409));
#12107=CARTESIAN_POINT('Ctrl Pts',(-0.0492359744271794,0.147556542424474,
0.66153514579337));
#12108=CARTESIAN_POINT('Ctrl Pts',(-0.0548577449395311,0.145634578815814,
0.661965692596482));
#12109=CARTESIAN_POINT('Ctrl Pts',(-0.0593186914332088,0.143875077990713,
0.662319887710196));
#12110=CARTESIAN_POINT('Ctrl Pts',(-0.063688650901166,0.141913911391341,
0.662679920979917));
#12111=CARTESIAN_POINT('Origin',(0.,0.,-0.129405622560373));
#12112=CARTESIAN_POINT('',(-0.0636886011499548,0.141913933718863,0.746625191472247));
#12113=CARTESIAN_POINT('',(-0.0636886287602419,0.141913921327825,0.732917465391055));
#12114=CARTESIAN_POINT('',(-0.0636886258329924,0.141913922641526,-0.129405622560373));
#12115=CARTESIAN_POINT('',(-0.155549981000406,7.68815545762296E-5,0.689293189475146));
#12116=CARTESIAN_POINT('Ctrl Pts',(-0.0636886011499548,0.141913933718863,
0.746625191472247));
#12117=CARTESIAN_POINT('Ctrl Pts',(-0.0573143785489615,0.144774578267551,
0.746084397578596));
#12118=CARTESIAN_POINT('Ctrl Pts',(-0.0507472492709453,0.147205842133469,
0.745539423472764));
#12119=CARTESIAN_POINT('Ctrl Pts',(-0.0397917799989713,0.15043919305941,
0.744666654528811));
#12120=CARTESIAN_POINT('Ctrl Pts',(-0.0355009023210546,0.151509179577591,
0.744333640805331));
#12121=CARTESIAN_POINT('Ctrl Pts',(-0.0305231620975979,0.152527291743769,
0.743961482087081));
#12122=CARTESIAN_POINT('Ctrl Pts',(-0.0298756598046069,0.15265543928807,
0.743913345014964));
#12123=CARTESIAN_POINT('Ctrl Pts',(-0.0289071952940793,0.152840710570873,
0.743841773724966));
#12124=CARTESIAN_POINT('Ctrl Pts',(-0.0285868488441498,0.152900951030528,
0.743818169157724));
#12125=CARTESIAN_POINT('Ctrl Pts',(-0.0280127969741062,0.153007033073725,
0.743775997876012));
#12126=CARTESIAN_POINT('Ctrl Pts',(-0.0277591659544253,0.153053251103599,
0.743757410169573));
#12127=CARTESIAN_POINT('Ctrl Pts',(-0.0272095078935997,0.153152001512819,
0.743717224732536));
#12128=CARTESIAN_POINT('Ctrl Pts',(-0.0269134439098565,0.153204306167541,
0.743695640046914));
#12129=CARTESIAN_POINT('Ctrl Pts',(-0.0260858465783675,0.153348042017064,
0.743635467893048));
#12130=CARTESIAN_POINT('Ctrl Pts',(-0.0255539795268914,0.153437568853032,
0.743596986469842));
#12131=CARTESIAN_POINT('Ctrl Pts',(-0.0224622143758307,0.153941469810441,
0.743374332132695));
#12132=CARTESIAN_POINT('Ctrl Pts',(-0.0198925461309444,0.154294575207567,
0.743193410574441));
#12133=CARTESIAN_POINT('Ctrl Pts',(-0.0026908929065488,0.156221352204686,
0.742002492315798));
#12134=CARTESIAN_POINT('Ctrl Pts',(0.0120931029397263,0.155776178144092,
0.741069653561887));
#12135=CARTESIAN_POINT('Ctrl Pts',(0.0284752546072518,0.152933323964381,
0.739952558378447));
#12136=CARTESIAN_POINT('Ctrl Pts',(0.03034861823162,0.152572614396229,0.739823673621564));
#12137=CARTESIAN_POINT('Ctrl Pts',(0.0361427178619844,0.151346047875282,
0.739420766145229));
#12138=CARTESIAN_POINT('Ctrl Pts',(0.0400366230296828,0.150362848847467,
0.739143815162361));
#12139=CARTESIAN_POINT('Ctrl Pts',(0.0447208406822449,0.148985243405018,
0.738801030264824));
#12140=CARTESIAN_POINT('Ctrl Pts',(0.0455517259364031,0.14873330680643,
0.738739855559981));
#12141=CARTESIAN_POINT('Ctrl Pts',(0.0469228679489378,0.148304989458365,
0.738638266675863));
#12142=CARTESIAN_POINT('Ctrl Pts',(0.0474643529357969,0.148132577847127,
0.73859798225899));
#12143=CARTESIAN_POINT('Ctrl Pts',(0.0484428727011502,0.147815096055153,
0.738524878416856));
#12144=CARTESIAN_POINT('Ctrl Pts',(0.0488802332889404,0.147671044293031,
0.738492092744318));
#12145=CARTESIAN_POINT('Ctrl Pts',(0.0498176088711473,0.147357683969654,
0.738421582581683));
#12146=CARTESIAN_POINT('Ctrl Pts',(0.0503174131703332,0.147187768166038,
0.738383838430702));
#12147=CARTESIAN_POINT('Ctrl Pts',(0.0516790663679986,0.146717108161522,
0.738280597626148));
#12148=CARTESIAN_POINT('Ctrl Pts',(0.0525391363779293,0.146411320636833,
0.73821493502858));
#12149=CARTESIAN_POINT('Ctrl Pts',(0.0570845946160769,0.144750029256393,
0.737865455598671));
#12150=CARTESIAN_POINT('Ctrl Pts',(0.0607200382423781,0.143263022853464,
0.737577297743301));
#12151=CARTESIAN_POINT('Ctrl Pts',(0.0777568437991727,0.135529467967245,
0.736183521620348));
#12152=CARTESIAN_POINT('Ctrl Pts',(0.0902777091810642,0.127530990518193,
0.73501810489613));
#12153=CARTESIAN_POINT('Ctrl Pts',(0.1048258504892,0.11500804823815,0.733551454573456));
#12154=CARTESIAN_POINT('Ctrl Pts',(0.108049403465252,0.1119850234781,0.73321867317898));
#12155=CARTESIAN_POINT('Ctrl Pts',(0.111601947867011,0.10835701755164,0.732846742012679));
#12156=CARTESIAN_POINT('Ctrl Pts',(0.112060671854064,0.107882546715695,
0.73279861223607));
#12157=CARTESIAN_POINT('Ctrl Pts',(0.112741427880196,0.107169394764387,
0.732727049637053));
#12158=CARTESIAN_POINT('Ctrl Pts',(0.112965743862985,0.106932920344534,
0.732703446525034));
#12159=CARTESIAN_POINT('Ctrl Pts',(0.113366152962936,0.106508142064163,
0.732661276809071));
#12160=CARTESIAN_POINT('Ctrl Pts',(0.113542521938729,0.106320104772796,
0.732642689219873));
#12161=CARTESIAN_POINT('Ctrl Pts',(0.113923566490701,0.105911821313951,
0.73260250285781));
#12162=CARTESIAN_POINT('Ctrl Pts',(0.114128070697715,0.105691420555265,
0.732580917135136));
#12163=CARTESIAN_POINT('Ctrl Pts',(0.114697677639162,0.105073955853852,
0.73252073916913));
#12164=CARTESIAN_POINT('Ctrl Pts',(0.1150613608363,0.104675578432192,0.732482253003976));
#12165=CARTESIAN_POINT('Ctrl Pts',(0.117162101998996,0.102350255315176,
0.73225951608949));
#12166=CARTESIAN_POINT('Ctrl Pts',(0.118852939359672,0.100381840210238,
0.732078519515728));
#12167=CARTESIAN_POINT('Ctrl Pts',(0.129799662769605,0.0869734059699074,
0.730887602100889));
#12168=CARTESIAN_POINT('Ctrl Pts',(0.137441959338346,0.0743111202246647,
0.729954814894502));
#12169=CARTESIAN_POINT('Ctrl Pts',(0.143937072388668,0.0590047947843232,
0.728837690423271));
#12170=CARTESIAN_POINT('Ctrl Pts',(0.144650328733272,0.0572339811682892,
0.728708717953214));
#12171=CARTESIAN_POINT('Ctrl Pts',(0.146761533152933,0.0517007072550992,
0.728305815900108));
#12172=CARTESIAN_POINT('Ctrl Pts',(0.148046487873488,0.0478972171677788,
0.728028961613457));
#12173=CARTESIAN_POINT('Ctrl Pts',(0.149428703404376,0.0432159550750357,
0.727686283715507));
#12174=CARTESIAN_POINT('Ctrl Pts',(0.149667564788807,0.0423813186433418,
0.727625115818986));
#12175=CARTESIAN_POINT('Ctrl Pts',(0.150051190884273,0.0409971403223736,
0.727523535902164));
#12176=CARTESIAN_POINT('Ctrl Pts',(0.150199955253999,0.0404487184784621,
0.727483253603748));
#12177=CARTESIAN_POINT('Ctrl Pts',(0.150463823585566,0.0394544335581914,
0.727410152022919));
#12178=CARTESIAN_POINT('Ctrl Pts',(0.150579959600077,0.0390088489174813,
0.727377366483463));
#12179=CARTESIAN_POINT('Ctrl Pts',(0.150824992727465,0.0380513175959221,
0.727306854847761));
#12180=CARTESIAN_POINT('Ctrl Pts',(0.150953265141815,0.0375392185902024,
0.72726910908299));
#12181=CARTESIAN_POINT('Ctrl Pts',(0.15129623311734,0.0361398084808301,
0.72716585936613));
#12182=CARTESIAN_POINT('Ctrl Pts',(0.151505725112019,0.035251256783263,
0.727100189421808));
#12183=CARTESIAN_POINT('Ctrl Pts',(0.152575112309186,0.030529791735562,
0.726750599483291));
#12184=CARTESIAN_POINT('Ctrl Pts',(0.153297331418468,0.0266675102533206,
0.72646233519781));
#12185=CARTESIAN_POINT('Ctrl Pts',(0.156037704955779,0.0081589522504735,
0.725068511443441));
#12186=CARTESIAN_POINT('Ctrl Pts',(0.156106799749517,-0.00669745341819393,
0.723903171207325));
#12187=CARTESIAN_POINT('Ctrl Pts',(0.153474088293961,-0.0257100987288768,
0.722436647152494));
#12188=CARTESIAN_POINT('Ctrl Pts',(0.15268226752861,-0.0300572639444694,
0.722103910848615));
#12189=CARTESIAN_POINT('Ctrl Pts',(0.151560596950402,-0.0350089052533985,
0.721732023847998));
#12190=CARTESIAN_POINT('Ctrl Pts',(0.151410704451113,-0.0356516004475047,
0.721683895488664));
#12191=CARTESIAN_POINT('Ctrl Pts',(0.151180675191396,-0.0366102742517521,
0.72161233457803));
#12192=CARTESIAN_POINT('Ctrl Pts',(0.151103630809113,-0.0369269751498208,
0.721588731748727));
#12193=CARTESIAN_POINT('Ctrl Pts',(0.15096386417344,-0.0374937418411552,
0.721546562336935));
#12194=CARTESIAN_POINT('Ctrl Pts',(0.150901515460847,-0.0377438948517119,
0.721527974770501));
#12195=CARTESIAN_POINT('Ctrl Pts',(0.150765105280708,-0.0382854532088609,
0.721487788228665));
#12196=CARTESIAN_POINT('Ctrl Pts',(0.150690820978907,-0.0385767983973127,
0.721466202304468));
#12197=CARTESIAN_POINT('Ctrl Pts',(0.150480905628401,-0.0393902336871026,
0.721406023209));
#12198=CARTESIAN_POINT('Ctrl Pts',(0.150343401098537,-0.0399118433277011,
0.721367536122352));
#12199=CARTESIAN_POINT('Ctrl Pts',(0.149528780023052,-0.0429380712438971,
0.721144783156171));
#12200=CARTESIAN_POINT('Ctrl Pts',(0.148791746389422,-0.0454263398781971,
0.720963772000498));
#12201=CARTESIAN_POINT('Ctrl Pts',(0.143462005232925,-0.0618948608962483,
0.719772854746293));
#12202=CARTESIAN_POINT('Ctrl Pts',(0.136967398017042,-0.0751821893527464,
0.718840077557524));
#12203=CARTESIAN_POINT('Ctrl Pts',(0.127629077402446,-0.0889396771574107,
0.717722947372951));
#12204=CARTESIAN_POINT('Ctrl Pts',(0.126527868172901,-0.0904994239460685,
0.717593957835289));
#12205=CARTESIAN_POINT('Ctrl Pts',(0.123023644878245,-0.095273770286096,
0.717191056835136));
#12206=CARTESIAN_POINT('Ctrl Pts',(0.12052490920674,-0.0984156999940041,
0.716914221361773));
#12207=CARTESIAN_POINT('Ctrl Pts',(0.117341438995376,-0.102115340843822,
0.71657156428182));
#12208=CARTESIAN_POINT('Ctrl Pts',(0.116769717040258,-0.102768620060293,
0.716510397710175));
#12209=CARTESIAN_POINT('Ctrl Pts',(0.115814775525421,-0.103841529089779,
0.716408819538363));
#12210=CARTESIAN_POINT('Ctrl Pts',(0.115434665751914,-0.104263911881839,
0.716368537652197));
#12211=CARTESIAN_POINT('Ctrl Pts',(0.1147423594554,-0.105024785082451,0.716295436511397));
#12212=CARTESIAN_POINT('Ctrl Pts',(0.114430956485173,-0.105363991593605,
0.716262650997818));
#12213=CARTESIAN_POINT('Ctrl Pts',(0.113759309866574,-0.10608911643179,
0.716192139075365));
#12214=CARTESIAN_POINT('Ctrl Pts',(0.11339859944167,-0.106474592455557,
0.716154392996477));
#12215=CARTESIAN_POINT('Ctrl Pts',(0.112408779293291,-0.107521636363341,
0.716051141544854));
#12216=CARTESIAN_POINT('Ctrl Pts',(0.111775805241721,-0.108179504736383,
0.715985470170497));
#12217=CARTESIAN_POINT('Ctrl Pts',(0.108388515998469,-0.111638545556464,
0.71563585871652));
#12218=CARTESIAN_POINT('Ctrl Pts',(0.105534852986288,-0.114339953218292,
0.715347573709146));
#12219=CARTESIAN_POINT('Ctrl Pts',(0.0914698378970639,-0.12667910983429,
0.713953740676999));
#12220=CARTESIAN_POINT('Ctrl Pts',(0.0790250668364783,-0.134793256058008,
0.712788415328505));
#12221=CARTESIAN_POINT('Ctrl Pts',(0.0616220930406426,-0.142891681479338,
0.711321820428744));
#12222=CARTESIAN_POINT('Ctrl Pts',(0.0575391416232965,-0.144584131753525,
0.710989000140358));
#12223=CARTESIAN_POINT('Ctrl Pts',(0.052770145372486,-0.1463268557379,0.710617093930375));
#12224=CARTESIAN_POINT('Ctrl Pts',(0.0521496093558077,-0.146549156389626,
0.710569023775148));
#12225=CARTESIAN_POINT('Ctrl Pts',(0.0512202836077782,-0.146875427406823,
0.710497532206486));
#12226=CARTESIAN_POINT('Ctrl Pts',(0.0509125608467141,-0.146982379155182,
0.710473940991376));
#12227=CARTESIAN_POINT('Ctrl Pts',(0.0503680306711304,-0.147169720129574,
0.710432341750079));
#12228=CARTESIAN_POINT('Ctrl Pts',(0.050131364257746,-0.147250505458193,
0.710414310626498));
#12229=CARTESIAN_POINT('Ctrl Pts',(0.049618126105051,-0.147424316866571,
0.710375314436903));
#12230=CARTESIAN_POINT('Ctrl Pts',(0.0493414878458612,-0.147517135352908,
0.710354361703613));
#12231=CARTESIAN_POINT('Ctrl Pts',(0.0485842181361713,-0.147768848197215,
0.710297182923058));
#12232=CARTESIAN_POINT('Ctrl Pts',(0.0481030638050704,-0.147926177605941,
0.710261047509789));
#12233=CARTESIAN_POINT('Ctrl Pts',(0.0470262035404419,-0.148272483072258,
0.710180590190179));
#12234=CARTESIAN_POINT('Ctrl Pts',(0.0464301055718878,-0.148460224929537,
0.710136336509763));
#12235=CARTESIAN_POINT('Ctrl Pts',(0.0445892835085485,-0.149027822437778,
0.710000501050794));
#12236=CARTESIAN_POINT('Ctrl Pts',(0.0433408744485835,-0.149395665725621,
0.709909538731034));
#12237=CARTESIAN_POINT('Ctrl Pts',(0.0385245689866483,-0.150749330955579,
0.709562515940091));
#12238=CARTESIAN_POINT('Ctrl Pts',(0.0349262837168794,-0.151623422729105,
0.709311430658154));
#12239=CARTESIAN_POINT('Ctrl Pts',(0.0217032330639749,-0.154339741465093,
0.70840696172466));
#12240=CARTESIAN_POINT('Ctrl Pts',(0.0119414849742218,-0.155400135168206,
0.707772694690845));
#12241=CARTESIAN_POINT('Ctrl Pts',(-0.00541271749503033,-0.155639416076207,
0.706618332509503));
#12242=CARTESIAN_POINT('Ctrl Pts',(-0.0129664430829459,-0.155192690348088,
0.706107115285203));
#12243=CARTESIAN_POINT('Ctrl Pts',(-0.021468665427403,-0.154064727335743,
0.705506414511639));
#12244=CARTESIAN_POINT('Ctrl Pts',(-0.0224788782829936,-0.153920576102233,
0.705434643730842));
#12245=CARTESIAN_POINT('Ctrl Pts',(-0.0240883403744863,-0.153674733425446,
0.705319631136846));
#12246=CARTESIAN_POINT('Ctrl Pts',(-0.0246885511904395,-0.153579449330068,
0.705276591235092));
#12247=CARTESIAN_POINT('Ctrl Pts',(-0.0257483514866636,-0.153404831741451,
0.705200325103425));
#12248=CARTESIAN_POINT('Ctrl Pts',(-0.0262081744201329,-0.153326943460039,
0.705167144937081));
#12249=CARTESIAN_POINT('Ctrl Pts',(-0.0271606444975024,-0.153161197137391,
0.705098225856666));
#12250=CARTESIAN_POINT('Ctrl Pts',(-0.0276532311613021,-0.153073027387669,
0.705062477418416));
#12251=CARTESIAN_POINT('Ctrl Pts',(-0.0289209465170841,-0.152839795923415,
0.704970198329306));
#12252=CARTESIAN_POINT('Ctrl Pts',(-0.0296954046940716,-0.15269121540844,
0.704913556584084));
#12253=CARTESIAN_POINT('Ctrl Pts',(-0.032959060693673,-0.152039311467853,
0.704673703735599));
#12254=CARTESIAN_POINT('Ctrl Pts',(-0.0354367337068162,-0.15148098363632,
0.704488755382251));
#12255=CARTESIAN_POINT('Ctrl Pts',(-0.0418850008861716,-0.149861055280161,
0.703999543462196));
#12256=CARTESIAN_POINT('Ctrl Pts',(-0.0458289086256457,-0.148702370045862,
0.703692364136736));
#12257=CARTESIAN_POINT('Ctrl Pts',(-0.0568361538246493,-0.144989050748367,
0.702812542890346));
#12258=CARTESIAN_POINT('Ctrl Pts',(-0.0637666235067489,-0.142077347630461,
0.702231166674509));
#12259=CARTESIAN_POINT('Ctrl Pts',(-0.0786196394803076,-0.134530810630353,
0.700939165071838));
#12260=CARTESIAN_POINT('Ctrl Pts',(-0.0863993512298343,-0.129671832192135,
0.700230367496002));
#12261=CARTESIAN_POINT('Ctrl Pts',(-0.0942535311948483,-0.123743859101679,
0.699509230520571));
#12262=CARTESIAN_POINT('Ctrl Pts',(-0.0947970337430191,-0.123327990529874,
0.699459303614591));
#12263=CARTESIAN_POINT('Ctrl Pts',(-0.0955991563778857,-0.122705799441843,
0.699385603908957));
#12264=CARTESIAN_POINT('Ctrl Pts',(-0.0958598813393453,-0.12250222476332,
0.699361645813828));
#12265=CARTESIAN_POINT('Ctrl Pts',(-0.0963139517615069,-0.122145348157204,
0.69931991971239));
#12266=CARTESIAN_POINT('Ctrl Pts',(-0.0965075833881976,-0.121992416700293,
0.699302125893107));
#12267=CARTESIAN_POINT('Ctrl Pts',(-0.0967017462591082,-0.121838314054877,
0.699284283190461));
#12268=CARTESIAN_POINT('Ctrl Pts',(-0.0967026378563213,-0.121837606398537,
0.699284201256644));
#12269=CARTESIAN_POINT('Ctrl Pts',(-0.0967044044783999,-0.121836204207641,
0.699284038911921));
#12270=CARTESIAN_POINT('Ctrl Pts',(-0.0967052795046704,-0.121835509672557,
0.699283958500886));
#12271=CARTESIAN_POINT('Ctrl Pts',(-0.0967070133576984,-0.121834133429989,
0.699283799167468));
#12272=CARTESIAN_POINT('Ctrl Pts',(-0.0967078721846693,-0.121833451722899,
0.699283720245065));
#12273=CARTESIAN_POINT('Ctrl Pts',(-0.0967095739965852,-0.121832100854239,
0.699283563856058));
#12274=CARTESIAN_POINT('Ctrl Pts',(-0.0967104169828092,-0.121831431692193,
0.699283486389338));
#12275=CARTESIAN_POINT('Ctrl Pts',(-0.096712087473058,-0.121830105629601,
0.69928333287863));
#12276=CARTESIAN_POINT('Ctrl Pts',(-0.0967129149730638,-0.121829448732764,
0.699283256835012));
#12277=CARTESIAN_POINT('Ctrl Pts',(-0.0967145548245948,-0.121828146937218,
0.699283106139844));
#12278=CARTESIAN_POINT('Ctrl Pts',(-0.0967153671779748,-0.121827502037534,
0.699283031488123));
#12279=CARTESIAN_POINT('Ctrl Pts',(-0.0967169770662906,-0.121826223975774,
0.69928288354642));
#12280=CARTESIAN_POINT('Ctrl Pts',(-0.0967177746039718,-0.121825590811998,
0.699282810256186));
#12281=CARTESIAN_POINT('Ctrl Pts',(-0.0967193551859499,-0.121824335965413,
0.699282665007585));
#12282=CARTESIAN_POINT('Ctrl Pts',(-0.0967201382306162,-0.121823714282771,
0.699282593049185));
#12283=CARTESIAN_POINT('Ctrl Pts',(-0.0967216901463187,-0.121822482145962,
0.699282450434868));
#12284=CARTESIAN_POINT('Ctrl Pts',(-0.0967224590141659,-0.121821871694769,
0.699282379779244));
#12285=CARTESIAN_POINT('Ctrl Pts',(-0.0967239828807618,-0.121820661780387,
0.699282239742497));
#12286=CARTESIAN_POINT('Ctrl Pts',(-0.0967247378780507,-0.121820062318781,
0.699282170361507));
#12287=CARTESIAN_POINT('Ctrl Pts',(-0.0967262342990919,-0.121818874150164,
0.699282032846867));
#12288=CARTESIAN_POINT('Ctrl Pts',(-0.0967269757237147,-0.121818285442869,
0.699281964713136));
#12289=CARTESIAN_POINT('Ctrl Pts',(-0.096728396462962,-0.121817157323821,
0.699281834153307));
#12290=CARTESIAN_POINT('Ctrl Pts',(-0.0967290757812409,-0.121816617910938,
0.699281771726873));
#12291=CARTESIAN_POINT('Ctrl Pts',(-0.0967304316296409,-0.121815541280617,
0.699281647130216));
#12292=CARTESIAN_POINT('Ctrl Pts',(-0.0967311081595325,-0.121815004063437,
0.699281584960014));
#12293=CARTESIAN_POINT('Ctrl Pts',(-0.0967324584536179,-0.121813931806913,
0.699281460873757));
#12294=CARTESIAN_POINT('Ctrl Pts',(-0.0967331322178909,-0.121813396767582,
0.699281398957695));
#12295=CARTESIAN_POINT('Ctrl Pts',(-0.0967344770057696,-0.121812328847102,
0.699281275377418));
#12296=CARTESIAN_POINT('Ctrl Pts',(-0.0967351480288432,-0.12181179596645,
0.699281213713252));
#12297=CARTESIAN_POINT('Ctrl Pts',(-0.0967364873495007,-0.121810732351498,
0.699281090635371));
#12298=CARTESIAN_POINT('Ctrl Pts',(-0.0967371556506375,-0.121810201614449,
0.699281029221331));
#12299=CARTESIAN_POINT('Ctrl Pts',(-0.0967384895595116,-0.121809142261436,
0.699280906640753));
#12300=CARTESIAN_POINT('Ctrl Pts',(-0.0967391551647717,-0.121808613647511,
0.699280845474443));
#12301=CARTESIAN_POINT('Ctrl Pts',(-0.0967404836959832,-0.121807558529772,
0.699280723388032));
#12302=CARTESIAN_POINT('Ctrl Pts',(-0.0967411466243366,-0.121807032024121,
0.69928066246771));
#12303=CARTESIAN_POINT('Ctrl Pts',(-0.0967424698314265,-0.121805981099561,
0.699280540870546));
#12304=CARTESIAN_POINT('Ctrl Pts',(-0.0967431301077306,-0.121805456682653,
0.699280480193928));
#12305=CARTESIAN_POINT('Ctrl Pts',(-0.0969739056985227,-0.121622162747296,
0.699259272885091));
#12306=CARTESIAN_POINT('Ctrl Pts',(-0.0972035052171123,-0.121438739433352,
0.699238173118612));
#12307=CARTESIAN_POINT('Ctrl Pts',(-0.0978276944467504,-0.120937180411758,
0.699180805485452));
#12308=CARTESIAN_POINT('Ctrl Pts',(-0.0982212559773331,-0.12061776113037,
0.699144627896046));
#12309=CARTESIAN_POINT('Ctrl Pts',(-0.0991018854580417,-0.119895863152338,
0.699063644506462));
#12310=CARTESIAN_POINT('Ctrl Pts',(-0.099588080074217,-0.119492326298826,
0.699018910908785));
#12311=CARTESIAN_POINT('Ctrl Pts',(-0.101083450683968,-0.118235716266999,
0.698881205651762));
#12312=CARTESIAN_POINT('Ctrl Pts',(-0.102084255965751,-0.11737271220482,
0.698788873359521));
#12313=CARTESIAN_POINT('Ctrl Pts',(-0.10591016440817,-0.113987633321759,
0.69843467673692));
#12314=CARTESIAN_POINT('Ctrl Pts',(-0.108653999531667,-0.111375295883887,
0.698178010346829));
#12315=CARTESIAN_POINT('Ctrl Pts',(-0.11844027040805,-0.101351742704892,
0.697240172004058));
#12316=CARTESIAN_POINT('Ctrl Pts',(-0.124842511012778,-0.093352211292088,
0.696579335331345));
#12317=CARTESIAN_POINT('Ctrl Pts',(-0.134248632985664,-0.0788835020583746,
0.695428563669994));
#12318=CARTESIAN_POINT('Ctrl Pts',(-0.137678259648649,-0.072732233019689,
0.694951309978228));
#12319=CARTESIAN_POINT('Ctrl Pts',(-0.141109804188978,-0.0654587067498898,
0.694387931426037));
#12320=CARTESIAN_POINT('Ctrl Pts',(-0.141531134578908,-0.0645426757093185,
0.69431700659571));
#12321=CARTESIAN_POINT('Ctrl Pts',(-0.142190640742558,-0.0630713026462111,
0.694203094601393));
#12322=CARTESIAN_POINT('Ctrl Pts',(-0.142434542903887,-0.0625185452596902,
0.694160303252533));
#12323=CARTESIAN_POINT('Ctrl Pts',(-0.142860776174381,-0.0615371279369823,
0.694084324979772));
#12324=CARTESIAN_POINT('Ctrl Pts',(-0.143044414786842,-0.0611090408493635,
0.694051182981923));
#12325=CARTESIAN_POINT('Ctrl Pts',(-0.143421937037418,-0.0602179577078676,
0.693982191268251));
#12326=CARTESIAN_POINT('Ctrl Pts',(-0.143615507670087,-0.059754835786256,
0.693946331409538));
#12327=CARTESIAN_POINT('Ctrl Pts',(-0.144110065923122,-0.0585553096000549,
0.693853439062178));
#12328=CARTESIAN_POINT('Ctrl Pts',(-0.144407648515963,-0.0578175266608104,
0.69379629263784));
#12329=CARTESIAN_POINT('Ctrl Pts',(-0.145654356664466,-0.0546569451104951,
0.693551405221163));
#12330=CARTESIAN_POINT('Ctrl Pts',(-0.146548215135496,-0.0522129522661191,
0.693361834721557));
#12331=CARTESIAN_POINT('Ctrl Pts',(-0.148739539438872,-0.0457210490005038,
0.692857372415726));
#12332=CARTESIAN_POINT('Ctrl Pts',(-0.149933042137028,-0.04164062662355,
0.692539332812466));
#12333=CARTESIAN_POINT('Ctrl Pts',(-0.15401454500164,-0.0252177077964493,
0.691256012606266));
#12334=CARTESIAN_POINT('Ctrl Pts',(-0.155556243311404,-0.0125932883211169,
0.690257429517547));
#12335=CARTESIAN_POINT('Ctrl Pts',(-0.155549981000406,7.68815545762296E-5,
0.689293189475146));
#12336=CARTESIAN_POINT('Ctrl Pts',(-0.155549980890396,7.71038094666679E-5,
0.68929317256085));
#12337=CARTESIAN_POINT('Ctrl Pts',(-0.155548056574785,0.00395923698251686,
0.688997730089396));
#12338=CARTESIAN_POINT('Ctrl Pts',(-0.15540079960715,0.00784042716544082,
0.688706369629833));
#12339=CARTESIAN_POINT('Ctrl Pts',(-0.155075286701211,0.0121511941037518,
0.688389983467841));
#12340=CARTESIAN_POINT('Ctrl Pts',(-0.155040297377641,0.0125897682665448,
0.688357878401912));
#12341=CARTESIAN_POINT('Ctrl Pts',(-0.15497865262095,0.0133231891107395,
0.68830433629505));
#12342=CARTESIAN_POINT('Ctrl Pts',(-0.154953015720463,0.0136181151163825,
0.688282845453773));
#12343=CARTESIAN_POINT('Ctrl Pts',(-0.154904757642047,0.0141554883212025,
0.688243762381385));
#12344=CARTESIAN_POINT('Ctrl Pts',(-0.154882408930206,0.0143979580482441,
0.688226155275795));
#12345=CARTESIAN_POINT('Ctrl Pts',(-0.154835217158718,0.0148971319366596,
0.688189965794114));
#12346=CARTESIAN_POINT('Ctrl Pts',(-0.154810305346525,0.0151538237033385,
0.68817138804088));
#12347=CARTESIAN_POINT('Ctrl Pts',(-0.154752344408021,0.0157359912993524,
0.68812932610603));
#12348=CARTESIAN_POINT('Ctrl Pts',(-0.154718906907653,0.0160614249862333,
0.688105863960416));
#12349=CARTESIAN_POINT('Ctrl Pts',(-0.154629746679346,0.0169030620505461,
0.688045311430264));
#12350=CARTESIAN_POINT('Ctrl Pts',(-0.154572465116616,0.0174191019555854,
0.688008306387435));
#12351=CARTESIAN_POINT('Ctrl Pts',(-0.154201181055804,0.0206177932842343,
0.687779631978769));
#12352=CARTESIAN_POINT('Ctrl Pts',(-0.153819910266708,0.0232923853163874,
0.687591491639772));
#12353=CARTESIAN_POINT('Ctrl Pts',(-0.153044980709305,0.0278713163664628,
0.687272560353994));
#12354=CARTESIAN_POINT('Ctrl Pts',(-0.152684951868742,0.029780572569399,
0.687140533614673));
#12355=CARTESIAN_POINT('Ctrl Pts',(-0.149850644858165,0.0434042532131832,
0.686202102441212));
#12356=CARTESIAN_POINT('Ctrl Pts',(-0.146066886193278,0.0548054974957794,
0.685433189541829));
#12357=CARTESIAN_POINT('Ctrl Pts',(-0.139216402343899,0.0695176245208165,
0.684346709819848));
#12358=CARTESIAN_POINT('Ctrl Pts',(-0.137262951775136,0.0732992780673955,
0.684058575602304));
#12359=CARTESIAN_POINT('Ctrl Pts',(-0.133867993735918,0.0792587214602847,
0.683585924482481));
#12360=CARTESIAN_POINT('Ctrl Pts',(-0.132522354160731,0.0814887043504419,
0.683404658647205));
#12361=CARTESIAN_POINT('Ctrl Pts',(-0.130693321582756,0.084354558036373,
0.683165338058722));
#12362=CARTESIAN_POINT('Ctrl Pts',(-0.130260068153889,0.0850220581387679,
0.683109134882886));
#12363=CARTESIAN_POINT('Ctrl Pts',(-0.129545185613298,0.0861051647237944,
0.683017165748169));
#12364=CARTESIAN_POINT('Ctrl Pts',(-0.129266628529204,0.0865227903249757,
0.682981514826514));
#12365=CARTESIAN_POINT('Ctrl Pts',(-0.128725717600621,0.087325306151855,
0.682912637185019));
#12366=CARTESIAN_POINT('Ctrl Pts',(-0.128463646509426,0.0877103812734499,
0.682879421384209));
#12367=CARTESIAN_POINT('Ctrl Pts',(-0.127857749995387,0.0885921167593224,
0.682802978899054));
#12368=CARTESIAN_POINT('Ctrl Pts',(-0.12751275505738,0.0890879602662635,
0.682759708149617));
#12369=CARTESIAN_POINT('Ctrl Pts',(-0.126584451991756,0.0904057233087287,
0.682643943686541));
#12370=CARTESIAN_POINT('Ctrl Pts',(-0.125996037532316,0.0912239920758776,
0.682571255456006));
#12371=CARTESIAN_POINT('Ctrl Pts',(-0.121246579160543,0.0976951311066141,
0.681989871605733));
#12372=CARTESIAN_POINT('Ctrl Pts',(-0.116715854506798,0.103065285289254,
0.681466714900051));
#12373=CARTESIAN_POINT('Ctrl Pts',(-0.104725685928213,0.115468931355165,
0.680152935583966));
#12374=CARTESIAN_POINT('Ctrl Pts',(-0.0969039435813654,0.122107098736112,
0.679351573746187));
#12375=CARTESIAN_POINT('Ctrl Pts',(-0.0853706033661158,0.130084705134222,
0.678273735803344));
#12376=CARTESIAN_POINT('Ctrl Pts',(-0.082175160234284,0.132126522617949,
0.677985047102469));
#12377=CARTESIAN_POINT('Ctrl Pts',(-0.0777686033058295,0.134720433213035,
0.677602921839187));
#12378=CARTESIAN_POINT('Ctrl Pts',(-0.0766205822576034,0.135376650302601,
0.67750478131097));
#12379=CARTESIAN_POINT('Ctrl Pts',(-0.0749115506911382,0.136324838650471,
0.677360903756288));
#12380=CARTESIAN_POINT('Ctrl Pts',(-0.0743569380349156,0.136628137150924,
0.677314553919367));
#12381=CARTESIAN_POINT('Ctrl Pts',(-0.0733506689532501,0.137170488695617,
0.677231093725719));
#12382=CARTESIAN_POINT('Ctrl Pts',(-0.0728996576866927,0.137410711132035,
0.677193915534618));
#12383=CARTESIAN_POINT('Ctrl Pts',(-0.0721883460888214,0.137785089647908,
0.677135648498658));
#12384=CARTESIAN_POINT('Ctrl Pts',(-0.0719288423143392,0.137920737699267,
0.677114467982603));
#12385=CARTESIAN_POINT('Ctrl Pts',(-0.0714399602564044,0.138174531476272,
0.677074712035956));
#12386=CARTESIAN_POINT('Ctrl Pts',(-0.0712106735813902,0.138292837992195,
0.677056126966165));
#12387=CARTESIAN_POINT('Ctrl Pts',(-0.0706887849509646,0.13856047810894,
0.677013961093206));
#12388=CARTESIAN_POINT('Ctrl Pts',(-0.0703960041067318,0.138709455419689,
0.676990402773698));
#12389=CARTESIAN_POINT('Ctrl Pts',(-0.0695021677941161,0.139160712145041,
0.676918769035741));
#12390=CARTESIAN_POINT('Ctrl Pts',(-0.0688996103649754,0.139460026058571,
0.676870874489821));
#12391=CARTESIAN_POINT('Ctrl Pts',(-0.0667713643040441,0.14050004870385,
0.676703030614361));
#12392=CARTESIAN_POINT('Ctrl Pts',(-0.0652356599949374,0.141219639250885,
0.676584293174888));
#12393=CARTESIAN_POINT('Ctrl Pts',(-0.0636886255638827,0.141913922762298,
0.676466729580158));
#12394=CARTESIAN_POINT('Ctrl Pts',(-0.063688650901166,0.141913911391341,
0.662679920979917));
#12395=CARTESIAN_POINT('Ctrl Pts',(-0.068017198513575,0.13997132975792,
0.663036542399741));
#12396=CARTESIAN_POINT('Ctrl Pts',(-0.0722564768373429,0.137830888847813,
0.663398887752939));
#12397=CARTESIAN_POINT('Ctrl Pts',(-0.0823242436398772,0.132154769206293,
0.664289282501908));
#12398=CARTESIAN_POINT('Ctrl Pts',(-0.0880293688476399,0.128425043328055,
0.664819914915556));
#12399=CARTESIAN_POINT('Ctrl Pts',(-0.096980935203349,0.12169542033187,
0.665683656014293));
#12400=CARTESIAN_POINT('Ctrl Pts',(-0.100377194888951,0.118909638481955,
0.666019496001153));
#12401=CARTESIAN_POINT('Ctrl Pts',(-0.105287253112897,0.114521660550206,
0.66651276070101));
#12402=CARTESIAN_POINT('Ctrl Pts',(-0.106892224411513,0.113025086184047,
0.666675320035616));
#12403=CARTESIAN_POINT('Ctrl Pts',(-0.108832375128955,0.111137658665867,
0.666872923066296));
#12404=CARTESIAN_POINT('Ctrl Pts',(-0.109197889274138,0.110778545070602,
0.666910199700956));
#12405=CARTESIAN_POINT('Ctrl Pts',(-0.109770801141017,0.110210074616639,
0.666968695988504));
#12406=CARTESIAN_POINT('Ctrl Pts',(-0.10997938538448,0.110001927821948,
0.666990007588517));
#12407=CARTESIAN_POINT('Ctrl Pts',(-0.110369854245646,0.109610057054866,
0.667029927782906));
#12408=CARTESIAN_POINT('Ctrl Pts',(-0.110551870131244,0.10942647461075,
0.667048546446941));
#12409=CARTESIAN_POINT('Ctrl Pts',(-0.110968381864329,0.109004278111474,
0.667091176375138));
#12410=CARTESIAN_POINT('Ctrl Pts',(-0.111202565996398,0.10876536094595,
0.667115163145199));
#12411=CARTESIAN_POINT('Ctrl Pts',(-0.111927105996519,0.108021391223322,
0.667189439115347));
#12412=CARTESIAN_POINT('Ctrl Pts',(-0.112414815037905,0.107513754602276,
0.667239527358037));
#12413=CARTESIAN_POINT('Ctrl Pts',(-0.117790473135738,0.10184187731401,
0.667792873615856));
#12414=CARTESIAN_POINT('Ctrl Pts',(-0.122323032149567,0.0963507700116848,
0.668271257306462));
#12415=CARTESIAN_POINT('Ctrl Pts',(-0.131528878105711,0.083496195099452,
0.669319885775283));
#12416=CARTESIAN_POINT('Ctrl Pts',(-0.135991181485854,0.0760122343812776,
0.669885513167569));
#12417=CARTESIAN_POINT('Ctrl Pts',(-0.142578586869586,0.0625074910798073,
0.670888272363713));
#12418=CARTESIAN_POINT('Ctrl Pts',(-0.145002715499442,0.0566571867506787,
0.671317233501453));
#12419=CARTESIAN_POINT('Ctrl Pts',(-0.147545489508619,0.0492779641791501,
0.671861516353689));
#12420=CARTESIAN_POINT('Ctrl Pts',(-0.148007272575461,0.0478731263711093,
0.671965256782573));
#12421=CARTESIAN_POINT('Ctrl Pts',(-0.148640062992512,0.0458513203841124,
0.672114826235472));
#12422=CARTESIAN_POINT('Ctrl Pts',(-0.148827410435187,0.045239515784646,
0.672160121225386));
#12423=CARTESIAN_POINT('Ctrl Pts',(-0.149145760143502,0.0441765259790005,
0.672238888096389));
#12424=CARTESIAN_POINT('Ctrl Pts',(-0.149278503926231,0.0437258673218194,
0.672272302819173));
#12425=CARTESIAN_POINT('Ctrl Pts',(-0.149529880770881,0.0428579679601338,
0.672336698404793));
#12426=CARTESIAN_POINT('Ctrl Pts',(-0.149648814251913,0.0424408181707076,
0.672367669154412));
#12427=CARTESIAN_POINT('Ctrl Pts',(-0.149955946836966,0.0413462313604879,
0.672448989485316));
#12428=CARTESIAN_POINT('Ctrl Pts',(-0.150141298564831,0.0406680129175078,
0.67249943073348));
#12429=CARTESIAN_POINT('Ctrl Pts',(-0.150769090616767,0.0383080640462042,
0.67267515177128));
#12430=CARTESIAN_POINT('Ctrl Pts',(-0.1511879085321,0.0366202445901691,
0.672801187063284));
#12431=CARTESIAN_POINT('Ctrl Pts',(-0.154228616276149,0.0234235497555797,
0.673789832264847));
#12432=CARTESIAN_POINT('Ctrl Pts',(-0.155560517056396,0.0116593737878267,
0.674694483054675));
#12433=CARTESIAN_POINT('Ctrl Pts',(-0.155544977013624,-0.00567160696188913,
0.676038358415671));
#12434=CARTESIAN_POINT('Ctrl Pts',(-0.155244895077116,-0.0111997338309086,
0.676467881282379));
#12435=CARTESIAN_POINT('Ctrl Pts',(-0.154171825791168,-0.0211367527301333,
0.67723176138205));
#12436=CARTESIAN_POINT('Ctrl Pts',(-0.153502005772645,-0.0255510788692451,
0.677568072100292));
#12437=CARTESIAN_POINT('Ctrl Pts',(-0.152515935877645,-0.0305798805954947,
0.67794344683171));
#12438=CARTESIAN_POINT('Ctrl Pts',(-0.152384551991569,-0.0312280026626399,
0.677991675472776));
#12439=CARTESIAN_POINT('Ctrl Pts',(-0.152182202474545,-0.0321945044890838,
0.678063351289277));
#12440=CARTESIAN_POINT('Ctrl Pts',(-0.152114364642188,-0.0325135194051921,
0.678086969586603));
#12441=CARTESIAN_POINT('Ctrl Pts',(-0.151991120312434,-0.0330842602826696,
0.678129150189201));
#12442=CARTESIAN_POINT('Ctrl Pts',(-0.151936091315621,-0.0333360629282256,
0.678147733572009));
#12443=CARTESIAN_POINT('Ctrl Pts',(-0.151815586118259,-0.0338809756018943,
0.678187892017362));
#12444=CARTESIAN_POINT('Ctrl Pts',(-0.151749887030346,-0.0341740323433377,
0.678209454121508));
#12445=CARTESIAN_POINT('Ctrl Pts',(-0.151564095228498,-0.0349916724720893,
0.678269519380939));
#12446=CARTESIAN_POINT('Ctrl Pts',(-0.15144212677316,-0.0355158326118633,
0.678307917057136));
#12447=CARTESIAN_POINT('Ctrl Pts',(-0.150720649827556,-0.0385450774292413,
0.678529257147511));
#12448=CARTESIAN_POINT('Ctrl Pts',(-0.150061666619405,-0.0410357841172182,
0.678708992518197));
#12449=CARTESIAN_POINT('Ctrl Pts',(-0.145222769189471,-0.0576448396847631,
0.679899500002206));
#12450=CARTESIAN_POINT('Ctrl Pts',(-0.139118076193454,-0.0711255991963758,
0.680832789825957));
#12451=CARTESIAN_POINT('Ctrl Pts',(-0.130206582842128,-0.08512064414634,
0.68194741897197));
#12452=CARTESIAN_POINT('Ctrl Pts',(-0.129177055985994,-0.0866750604225387,
0.682073351012123));
#12453=CARTESIAN_POINT('Ctrl Pts',(-0.125815431985952,-0.0915575919891249,
0.682476466585702));
#12454=CARTESIAN_POINT('Ctrl Pts',(-0.12338091746222,-0.0948127620834062,
0.68275669834497));
#12455=CARTESIAN_POINT('Ctrl Pts',(-0.120273046910367,-0.098645609184231,
0.683103111027972));
#12456=CARTESIAN_POINT('Ctrl Pts',(-0.119718484239365,-0.0993179062447148,
0.683164513302434));
#12457=CARTESIAN_POINT('Ctrl Pts',(-0.118792444629253,-0.10042151947745,
0.683266395062366));
#12458=CARTESIAN_POINT('Ctrl Pts',(-0.118424191953835,-0.100855526470347,
0.683306743395405));
#12459=CARTESIAN_POINT('Ctrl Pts',(-0.117753774679885,-0.101636917605477,
0.683379905781965));
#12460=CARTESIAN_POINT('Ctrl Pts',(-0.117452432537582,-0.101985001614719,
0.683412685750271));
#12461=CARTESIAN_POINT('Ctrl Pts',(-0.116802903639582,-0.102728583422733,
0.683483119938));
#12462=CARTESIAN_POINT('Ctrl Pts',(-0.116454244598768,-0.103123659036102,
0.683520793529576));
#12463=CARTESIAN_POINT('Ctrl Pts',(-0.115498747311813,-0.104195335346355,
0.683623678845034));
#12464=CARTESIAN_POINT('Ctrl Pts',(-0.114887983981592,-0.104868391854024,
0.683689054668293));
#12465=CARTESIAN_POINT('Ctrl Pts',(-0.111642695206594,-0.108382296460608,
0.68403444839281));
#12466=CARTESIAN_POINT('Ctrl Pts',(-0.108908836611452,-0.111129086813327,
0.684318687967596));
#12467=CARTESIAN_POINT('Ctrl Pts',(-0.0952395680371516,-0.123873791632705,
0.685710298570283));
#12468=CARTESIAN_POINT('Ctrl Pts',(-0.0830164219644928,-0.132376046640035,
0.686878067383553));
#12469=CARTESIAN_POINT('Ctrl Pts',(-0.0658083933527459,-0.141013497902221,
0.688349445391028));
#12470=CARTESIAN_POINT('Ctrl Pts',(-0.0617526037190603,-0.142836186894842,
0.688684336672733));
#12471=CARTESIAN_POINT('Ctrl Pts',(-0.0570101957502238,-0.144727594430487,
0.689058322529715));
#12472=CARTESIAN_POINT('Ctrl Pts',(-0.0563949464308064,-0.144968441628414,
0.689106507441296));
#12473=CARTESIAN_POINT('Ctrl Pts',(-0.055473824203223,-0.145322275030348,
0.689178131172802));
#12474=CARTESIAN_POINT('Ctrl Pts',(-0.0551691112552447,-0.145438227300577,
0.689201740755889));
#12475=CARTESIAN_POINT('Ctrl Pts',(-0.0546228605468499,-0.145644128042777,
0.689243911973408));
#12476=CARTESIAN_POINT('Ctrl Pts',(-0.0543814628258599,-0.145734434613504,
0.689262494645179));
#12477=CARTESIAN_POINT('Ctrl Pts',(-0.0538582053854122,-0.145928703349405,
0.689302658588828));
#12478=CARTESIAN_POINT('Ctrl Pts',(-0.0535762693818314,-0.146032448831979,
0.68932422687121));
#12479=CARTESIAN_POINT('Ctrl Pts',(-0.0527880776877376,-0.146319894031104,
0.689384326743801));
#12480=CARTESIAN_POINT('Ctrl Pts',(-0.0522811592007497,-0.146501784804078,
0.689422752657956));
#12481=CARTESIAN_POINT('Ctrl Pts',(-0.0493382173653042,-0.147540540710993,
0.689644581509973));
#12482=CARTESIAN_POINT('Ctrl Pts',(-0.0468819191985013,-0.148339335988197,
0.689824760815528));
#12483=CARTESIAN_POINT('Ctrl Pts',(-0.0303010697154155,-0.15327840894129,
0.691015260900772));
#12484=CARTESIAN_POINT('Ctrl Pts',(-0.0156691863389914,-0.155457426698968,
0.691948243831195));
#12485=CARTESIAN_POINT('Ctrl Pts',(0.000923992207560616,-0.155558515738684,
0.69306302336376));
#12486=CARTESIAN_POINT('Ctrl Pts',(0.00279560811795781,-0.155536136534543,
0.693189453402145));
#12487=CARTESIAN_POINT('Ctrl Pts',(0.00872016387768964,-0.155358326918353,
0.693592551480902));
#12488=CARTESIAN_POINT('Ctrl Pts',(0.0127673665477948,-0.155078175287072,
0.693872248081887));
#12489=CARTESIAN_POINT('Ctrl Pts',(0.0176644519419164,-0.154546200123709,
0.694218058525394));
#12490=CARTESIAN_POINT('Ctrl Pts',(0.0185293621350384,-0.154444888290468,
0.694279413225571));
#12491=CARTESIAN_POINT('Ctrl Pts',(0.0199578980157496,-0.154265383483883,
0.694381232335576));
#12492=CARTESIAN_POINT('Ctrl Pts',(0.0205220350325007,-0.154191349618434,
0.694421565877277));
#12493=CARTESIAN_POINT('Ctrl Pts',(0.0215418854419725,-0.154051814754689,
0.694494712436008));
#12494=CARTESIAN_POINT('Ctrl Pts',(0.0219977405802601,-0.153987382140934,
0.694527491435966));
#12495=CARTESIAN_POINT('Ctrl Pts',(0.0229748573558366,-0.153844844703004,
0.694597935721334));
#12496=CARTESIAN_POINT('Ctrl Pts',(0.0234960201244876,-0.153766112449707,
0.694635620431662));
#12497=CARTESIAN_POINT('Ctrl Pts',(0.024915422524783,-0.153544298248632,
0.694738567113799));
#12498=CARTESIAN_POINT('Ctrl Pts',(0.0258128110277106,-0.153395986015988,
0.69480399351563));
#12499=CARTESIAN_POINT('Ctrl Pts',(0.0305352080194024,-0.152572899030745,
0.695150138013753));
#12500=CARTESIAN_POINT('Ctrl Pts',(0.0343349179965368,-0.151762962761304,
0.695435099683119));
#12501=CARTESIAN_POINT('Ctrl Pts',(0.0524572277745169,-0.147184667285636,
0.696827025332424));
#12502=CARTESIAN_POINT('Ctrl Pts',(0.0662218406495348,-0.141525996856218,
0.697994265901072));
#12503=CARTESIAN_POINT('Ctrl Pts',(0.0828004875208679,-0.131755820335562,
0.699464785448405));
#12504=CARTESIAN_POINT('Ctrl Pts',(0.0865279212759689,-0.129338489521177,
0.699799377249114));
#12505=CARTESIAN_POINT('Ctrl Pts',(0.0906855103241419,-0.126381869980952,
0.700173069982034));
#12506=CARTESIAN_POINT('Ctrl Pts',(0.0912214013173557,-0.12599561431374,
0.700221245611605));
#12507=CARTESIAN_POINT('Ctrl Pts',(0.0920180708579799,-0.125413649220629,
0.700292858286985));
#12508=CARTESIAN_POINT('Ctrl Pts',(0.0922807116386719,-0.125220521640903,
0.700316466019855));
#12509=CARTESIAN_POINT('Ctrl Pts',(0.0927499054741206,-0.124873231563961,
0.700358635245281));
#12510=CARTESIAN_POINT('Ctrl Pts',(0.0929566833736199,-0.124719380797038,
0.700377217766641));
#12511=CARTESIAN_POINT('Ctrl Pts',(0.0934036705001353,-0.124385075860508,
0.700417382880235));
#12512=CARTESIAN_POINT('Ctrl Pts',(0.0936437389667213,-0.124204440002033,
0.700438952476365));
#12513=CARTESIAN_POINT('Ctrl Pts',(0.0943127491122702,-0.123698011227758,
0.700499059709901));
#12514=CARTESIAN_POINT('Ctrl Pts',(0.0947405298629848,-0.123370679867716,
0.700537491629346));
#12515=CARTESIAN_POINT('Ctrl Pts',(0.0972103351503213,-0.12146039992029,
0.700759424604099));
#12516=CARTESIAN_POINT('Ctrl Pts',(0.0992145216248112,-0.119828873039177,
0.700939698487263));
#12517=CARTESIAN_POINT('Ctrl Pts',(0.112355582129889,-0.10857539188738,
0.702130197129907));
#12518=CARTESIAN_POINT('Ctrl Pts',(0.122119935124537,-0.0974639593988757,
0.703063114775693));
#12519=CARTESIAN_POINT('Ctrl Pts',(0.131203062074052,-0.0835767189661042,
0.704177927175531));
#12520=CARTESIAN_POINT('Ctrl Pts',(0.132199986392239,-0.0819906986190413,
0.704304464028192));
#12521=CARTESIAN_POINT('Ctrl Pts',(0.135263033294116,-0.0769165038369862,
0.704707554756115));
#12522=CARTESIAN_POINT('Ctrl Pts',(0.137221418644689,-0.0733656193836609,
0.704987132868446));
#12523=CARTESIAN_POINT('Ctrl Pts',(0.139429156431116,-0.0689642731076854,
0.705332812218683));
#12524=CARTESIAN_POINT('Ctrl Pts',(0.139812998036409,-0.0681827408774246,
0.705394158646061));
#12525=CARTESIAN_POINT('Ctrl Pts',(0.140436766469974,-0.0668852810136515,
0.705495966861504));
#12526=CARTESIAN_POINT('Ctrl Pts',(0.140680463639622,-0.0663711784387937,
0.705536297830852));
#12527=CARTESIAN_POINT('Ctrl Pts',(0.141116247230638,-0.0654386676416063,
0.705609441637799));
#12528=CARTESIAN_POINT('Ctrl Pts',(0.141309307831825,-0.0650207195200458,
0.705642220470181));
#12529=CARTESIAN_POINT('Ctrl Pts',(0.14171942205374,-0.0641224278479023,
0.705712666515595));
#12530=CARTESIAN_POINT('Ctrl Pts',(0.141935894624611,-0.0636418270073892,
0.705750353162732));
#12531=CARTESIAN_POINT('Ctrl Pts',(0.142519289510958,-0.0623288227238584,
0.705853310535296));
#12532=CARTESIAN_POINT('Ctrl Pts',(0.142881354083872,-0.0614942974160983,
0.705918745748376));
#12533=CARTESIAN_POINT('Ctrl Pts',(0.144751316558782,-0.0570785238603094,
0.706265021247061));
#12534=CARTESIAN_POINT('Ctrl Pts',(0.146131817579184,-0.0534451908844771,
0.706550108933191));
#12535=CARTESIAN_POINT('Ctrl Pts',(0.152111900153953,-0.0357354340290918,
0.70794208972485));
#12536=CARTESIAN_POINT('Ctrl Pts',(0.154821087855728,-0.0211029662831042,
0.709109238293607));
#12537=CARTESIAN_POINT('Ctrl Pts',(0.155602013593444,-0.00187731027392902,
0.710579608063287));
#12538=CARTESIAN_POINT('Ctrl Pts',(0.155592231567148,0.00256466499622176,
0.710914147470928));
#12539=CARTESIAN_POINT('Ctrl Pts',(0.15536265919091,0.00766047926721451,
0.711287788919633));
#12540=CARTESIAN_POINT('Ctrl Pts',(0.155328727619254,0.00832017016775597,
0.711335962923356));
#12541=CARTESIAN_POINT('Ctrl Pts',(0.155271774790372,0.00930509139248887,
0.711407573662109));
#12542=CARTESIAN_POINT('Ctrl Pts',(0.155251932392416,0.00963048628550986,
0.711431181070874));
#12543=CARTESIAN_POINT('Ctrl Pts',(0.15521457096105,0.0102130254034281,
0.711473349947363));
#12544=CARTESIAN_POINT('Ctrl Pts',(0.155197435745348,0.0104701894976847,
0.711491932442396));
#12545=CARTESIAN_POINT('Ctrl Pts',(0.155158941812179,0.0110270366554358,
0.711532097761023));
#12546=CARTESIAN_POINT('Ctrl Pts',(0.155137354088246,0.0113266999756158,
0.711553667587355));
#12547=CARTESIAN_POINT('Ctrl Pts',(0.155074637691405,0.0121634447318391,
0.711613776110747));
#12548=CARTESIAN_POINT('Ctrl Pts',(0.155031586738179,0.0127003850033983,
0.711652209082502));
#12549=CARTESIAN_POINT('Ctrl Pts',(0.154765856369803,0.0158116718584473,
0.711874160309211));
#12550=CARTESIAN_POINT('Ctrl Pts',(0.154481830883446,0.0183805685041798,
0.712054450771302));
#12551=CARTESIAN_POINT('Ctrl Pts',(0.152152610299058,0.0355242166807686,
0.71324494916589));
#12552=CARTESIAN_POINT('Ctrl Pts',(0.148111738869294,0.0497534819534633,
0.714177855371147));
#12553=CARTESIAN_POINT('Ctrl Pts',(0.141369157485213,0.0649158978496598,
0.715292673562299));
#12554=CARTESIAN_POINT('Ctrl Pts',(0.140577064666596,0.0666138197572454,
0.715419229164823));
#12555=CARTESIAN_POINT('Ctrl Pts',(0.137974711268721,0.0719389552762498,
0.715822318605974));
#12556=CARTESIAN_POINT('Ctrl Pts',(0.136053369318516,0.0755096685069591,
0.716101875922684));
#12557=CARTESIAN_POINT('Ctrl Pts',(0.133552716758185,0.0797510654385667,
0.716447532265028));
#12558=CARTESIAN_POINT('Ctrl Pts',(0.133104230248,0.0804973566478612,0.71650887724018));
#12559=CARTESIAN_POINT('Ctrl Pts',(0.132352370400346,0.0817250037313298,
0.716610683543158));
#12560=CARTESIAN_POINT('Ctrl Pts',(0.132052574800892,0.0822085376243107,
0.716651014060941));
#12561=CARTESIAN_POINT('Ctrl Pts',(0.131505395881217,0.0830803545301993,
0.716724157384853));
#12562=CARTESIAN_POINT('Ctrl Pts',(0.13125892735468,0.0834692065140469,
0.716756936187843));
#12563=CARTESIAN_POINT('Ctrl Pts',(0.130726573604193,0.0843009092418634,
0.716827382542345));
#12564=CARTESIAN_POINT('Ctrl Pts',(0.130440157072864,0.0847434112806142,
0.716865069529576));
#12565=CARTESIAN_POINT('Ctrl Pts',(0.129653314814835,0.0859456108310081,
0.716968028779353));
#12566=CARTESIAN_POINT('Ctrl Pts',(0.129148471793413,0.0867023773128583,
0.717033465539673));
#12567=CARTESIAN_POINT('Ctrl Pts',(0.126452185197167,0.0906683444717917,
0.717379764048225));
#12568=CARTESIAN_POINT('Ctrl Pts',(0.124147878108818,0.0937987377124655,
0.717664873869456));
#12569=CARTESIAN_POINT('Ctrl Pts',(0.112510817896961,0.108426754153507,
0.719056864351944));
#12570=CARTESIAN_POINT('Ctrl Pts',(0.101685834197047,0.118637638695264,
0.720223996766467));
#12571=CARTESIAN_POINT('Ctrl Pts',(0.0859561132231783,0.129719145390344,
0.721694342009498));
#12572=CARTESIAN_POINT('Ctrl Pts',(0.0822187321792526,0.132119639955574,
0.722028873941542));
#12573=CARTESIAN_POINT('Ctrl Pts',(0.0778128282158,0.13469002395874,0.722402506895644));
#12574=CARTESIAN_POINT('Ctrl Pts',(0.0772401708133397,0.135019238790746,
0.722450679531708));
#12575=CARTESIAN_POINT('Ctrl Pts',(0.0763817739542957,0.135505473607316,
0.722522288641374));
#12576=CARTESIAN_POINT('Ctrl Pts',(0.0760976199348284,0.135665253530529,
0.722545895777497));
#12577=CARTESIAN_POINT('Ctrl Pts',(0.0755922805287867,0.135947318832112,
0.722587703039956));
#12578=CARTESIAN_POINT('Ctrl Pts',(0.0753712983987127,0.136069959044185,
0.722605925603602));
#12579=CARTESIAN_POINT('Ctrl Pts',(0.0748947144111918,0.136332935403301,
0.722645097131703));
#12580=CARTESIAN_POINT('Ctrl Pts',(0.0746390173088581,0.136473091198937,
0.722666034555502));
#12581=CARTESIAN_POINT('Ctrl Pts',(0.0741084946162756,0.136761950719259,
0.722709315728716));
#12582=CARTESIAN_POINT('Ctrl Pts',(0.0738336116769774,0.136910547183552,
0.722731652718698));
#12583=CARTESIAN_POINT('Ctrl Pts',(0.0731355265874104,0.137285204772479,
0.72278815984087));
#12584=CARTESIAN_POINT('Ctrl Pts',(0.0727117188291189,0.137510140205285,
0.722822261778076));
#12585=CARTESIAN_POINT('Ctrl Pts',(0.071490863686974,0.138150885147711,
0.722919935026978));
#12586=CARTESIAN_POINT('Ctrl Pts',(0.070691227261039,0.138561759304666,
0.722983222341033));
#12587=CARTESIAN_POINT('Ctrl Pts',(0.0615260607739091,0.143171066941971,
0.723701319482948));
#12588=CARTESIAN_POINT('Ctrl Pts',(0.0528002153092404,0.146613783699978,
0.724316828381261));
#12589=CARTESIAN_POINT('Ctrl Pts',(0.0327889707256326,0.152488605101206,
0.725689542534843));
#12590=CARTESIAN_POINT('Ctrl Pts',(0.0214381869515838,0.154493521305979,
0.726444795148573));
#12591=CARTESIAN_POINT('Ctrl Pts',(0.00822654953847539,0.155342143845186,
0.727364808355722));
#12592=CARTESIAN_POINT('Ctrl Pts',(0.00648051060938771,0.155424773837839,
0.727487129460105));
#12593=CARTESIAN_POINT('Ctrl Pts',(0.00402922224027828,0.155499403050392,
0.72766004637409));
#12594=CARTESIAN_POINT('Ctrl Pts',(0.00332480763725275,0.155516058995937,
0.727709873957952));
#12595=CARTESIAN_POINT('Ctrl Pts',(0.00218631863673489,0.155535240111994,
0.727790638388596));
#12596=CARTESIAN_POINT('Ctrl Pts',(0.00175229812578089,0.155540735340245,
0.727821482295465));
#12597=CARTESIAN_POINT('Ctrl Pts',(0.000848684763719505,0.15554839361092,
0.72788581431212));
#12598=CARTESIAN_POINT('Ctrl Pts',(0.000379094422689995,0.155550246863475,
0.727919311763792));
#12599=CARTESIAN_POINT('Ctrl Pts',(-0.000729141509548038,0.155549602138571,
0.727998523893856));
#12600=CARTESIAN_POINT('Ctrl Pts',(-0.0013677732940302,0.155545297410417,
0.728044294469447));
#12601=CARTESIAN_POINT('Ctrl Pts',(-0.00347811302031817,0.155518075063737,
0.728195962925053));
#12602=CARTESIAN_POINT('Ctrl Pts',(-0.00494948184701168,0.155478201990687,
0.728302386616676));
#12603=CARTESIAN_POINT('Ctrl Pts',(-0.0126876976832074,0.15515855012282,
0.728865835223222));
#12604=CARTESIAN_POINT('Ctrl Pts',(-0.0189330890713884,0.154520780887436,
0.729333872232452));
#12605=CARTESIAN_POINT('Ctrl Pts',(-0.0343353319763814,0.152000139872101,
0.730521081495637));
#12606=CARTESIAN_POINT('Ctrl Pts',(-0.0433935718138847,0.149666067153807,
0.731249759660826));
#12607=CARTESIAN_POINT('Ctrl Pts',(-0.0560812712273453,0.145147451604106,
0.732289502199682));
#12608=CARTESIAN_POINT('Ctrl Pts',(-0.0599181983650028,0.143606028342147,
0.732606338978805));
#12609=CARTESIAN_POINT('Ctrl Pts',(-0.0636886287602419,0.141913921327825,
0.732917465391055));
#12610=CARTESIAN_POINT('Origin',(0.,0.,-0.129405622560373));
#12611=CARTESIAN_POINT('',(-0.0636886258329888,0.141913922641528,0.816746504307747));
#12612=CARTESIAN_POINT('',(-0.0636886325197553,0.141913919640617,0.802807733721352));
#12613=CARTESIAN_POINT('',(-0.0636886258329924,0.141913922641526,-0.129405622560373));
#12614=CARTESIAN_POINT('Ctrl Pts',(-0.0636886258329888,0.141913922641528,
0.816746504307747));
#12615=CARTESIAN_POINT('Ctrl Pts',(-0.0626085849357707,0.14239862716739,
0.816663661869299));
#12616=CARTESIAN_POINT('Ctrl Pts',(-0.061523072900136,0.142870974281785,
0.816580416551277));
#12617=CARTESIAN_POINT('Ctrl Pts',(-0.0598935254377186,0.143558037018761,
0.816455425860265));
#12618=CARTESIAN_POINT('Ctrl Pts',(-0.0593534800960053,0.143782157327041,
0.816413999010022));
#12619=CARTESIAN_POINT('Ctrl Pts',(-0.0583832635698295,0.144178402337241,
0.816339560473828));
#12620=CARTESIAN_POINT('Ctrl Pts',(-0.0579535603104242,0.144351660899428,
0.816306587444798));
#12621=CARTESIAN_POINT('Ctrl Pts',(-0.0570488798741372,0.144711742125908,
0.816237154243));
#12622=CARTESIAN_POINT('Ctrl Pts',(-0.056573745295578,0.144898151595469,
0.816200680660453));
#12623=CARTESIAN_POINT('Ctrl Pts',(-0.055320109028202,0.145382884469277,
0.816104420640522));
#12624=CARTESIAN_POINT('Ctrl Pts',(-0.0545401206827073,0.145677289737176,
0.816044504199232));
#12625=CARTESIAN_POINT('Ctrl Pts',(-0.0512584627898476,0.146885896426461,
0.81579227986365));
#12626=CARTESIAN_POINT('Ctrl Pts',(-0.048736031798294,0.14774198507016,
0.815598065871951));
#12627=CARTESIAN_POINT('Ctrl Pts',(-0.0315718790675979,0.153079954475024,
0.81427322900165));
#12628=CARTESIAN_POINT('Ctrl Pts',(-0.0163612209060666,0.155442490040404,
0.813071153392481));
#12629=CARTESIAN_POINT('Ctrl Pts',(0.00426227194055146,0.155582527565222,
0.811487537108713));
#12630=CARTESIAN_POINT('Ctrl Pts',(0.00957980275595861,0.155345845516234,
0.811084657667849));
#12631=CARTESIAN_POINT('Ctrl Pts',(0.0155236950559502,0.154774809316907,
0.810647354029034));
#12632=CARTESIAN_POINT('Ctrl Pts',(0.0161716398631995,0.154708451002783,
0.810599859752694));
#12633=CARTESIAN_POINT('Ctrl Pts',(0.0171414634305739,0.154602968397244,
0.810529054691374));
#12634=CARTESIAN_POINT('Ctrl Pts',(0.0174636565176181,0.154566905617053,
0.810505578784916));
#12635=CARTESIAN_POINT('Ctrl Pts',(0.0180417315800823,0.154500371592342,
0.810463545457661));
#12636=CARTESIAN_POINT('Ctrl Pts',(0.018297651351116,0.15447027176465,0.810444967639323));
#12637=CARTESIAN_POINT('Ctrl Pts',(0.0188533090009909,0.154403518164273,
0.810404698237779));
#12638=CARTESIAN_POINT('Ctrl Pts',(0.0191530144861062,0.154366627617865,
0.810383020167474));
#12639=CARTESIAN_POINT('Ctrl Pts',(0.0199792050220714,0.154262489187437,
0.810323372053753));
#12640=CARTESIAN_POINT('Ctrl Pts',(0.020505463007932,0.154193418187613,
0.810285502740853));
#12641=CARTESIAN_POINT('Ctrl Pts',(0.0231937495080265,0.153826575893572,
0.810092644510992));
#12642=CARTESIAN_POINT('Ctrl Pts',(0.0253498308491427,0.153486002113901,
0.809939918326207));
#12643=CARTESIAN_POINT('Ctrl Pts',(0.0413045518527728,0.150620389460298,
0.808819457603409));
#12644=CARTESIAN_POINT('Ctrl Pts',(0.0547137116318943,0.146284266570763,
0.80792688339334));
#12645=CARTESIAN_POINT('Ctrl Pts',(0.0714805038753536,0.13822889498148,
0.806684765406559));
#12646=CARTESIAN_POINT('Ctrl Pts',(0.0755104611525617,0.136069300286315,
0.80637606028091));
#12647=CARTESIAN_POINT('Ctrl Pts',(0.0809988836628154,0.132809163889201,
0.805936707844174));
#12648=CARTESIAN_POINT('Ctrl Pts',(0.0825421222573581,0.131855567813592,
0.805810992977536));
#12649=CARTESIAN_POINT('Ctrl Pts',(0.0848592039434004,0.130367180249647,
0.805618674622934));
#12650=CARTESIAN_POINT('Ctrl Pts',(0.0856454910997768,0.129851977138239,
0.805552775382605));
#12651=CARTESIAN_POINT('Ctrl Pts',(0.0870953527582119,0.128883079271673,
0.80543004021721));
#12652=CARTESIAN_POINT('Ctrl Pts',(0.0877601768812447,0.128431304224809,
0.80537327658187));
#12653=CARTESIAN_POINT('Ctrl Pts',(0.0888359245777928,0.127688036998965,
0.805280620159881));
#12654=CARTESIAN_POINT('Ctrl Pts',(0.0892489924009949,0.127399661038663,
0.805244845728522));
#12655=CARTESIAN_POINT('Ctrl Pts',(0.0900407870163033,0.126841143089946,
0.805175888606833));
#12656=CARTESIAN_POINT('Ctrl Pts',(0.0904197176996317,0.12657129828423,
0.805142717539861));
#12657=CARTESIAN_POINT('Ctrl Pts',(0.0912847066690999,0.125949454079457,
0.805066603235888));
#12658=CARTESIAN_POINT('Ctrl Pts',(0.0917699470874756,0.125596335326539,
0.805023617185629));
#12659=CARTESIAN_POINT('Ctrl Pts',(0.0930538170499614,0.124650626144344,
0.804909107669234));
#12660=CARTESIAN_POINT('Ctrl Pts',(0.0938488161834835,0.124053178440869,
0.804837396287636));
#12661=CARTESIAN_POINT('Ctrl Pts',(0.0997841511117801,0.119503023061095,
0.804295830195685));
#12662=CARTESIAN_POINT('Ctrl Pts',(0.104677797073148,0.115240556817054,
0.803813702258976));
#12663=CARTESIAN_POINT('Ctrl Pts',(0.11672015718757,0.103349980929197,0.802528909301267));
#12664=CARTESIAN_POINT('Ctrl Pts',(0.123391803047791,0.0952850644481384,
0.801711899434893));
#12665=CARTESIAN_POINT('Ctrl Pts',(0.131455646399825,0.0832559801104097,
0.800597074853583));
#12666=CARTESIAN_POINT('Ctrl Pts',(0.133575094106209,0.0798113065309945,
0.800288597757142));
#12667=CARTESIAN_POINT('Ctrl Pts',(0.136577370427651,0.0744764658864343,
0.799830652367178));
#12668=CARTESIAN_POINT('Ctrl Pts',(0.137560344625351,0.0726448540707293,
0.799676812357502));
#12669=CARTESIAN_POINT('Ctrl Pts',(0.138735614427269,0.0703454724372923,
0.799488334681132));
#12670=CARTESIAN_POINT('Ctrl Pts',(0.138962678204106,0.0698958531548797,
0.799451697553405));
#12671=CARTESIAN_POINT('Ctrl Pts',(0.139318278893569,0.0691831294363092,
0.799393973926168));
#12672=CARTESIAN_POINT('Ctrl Pts',(0.139448261067244,0.0689207568274182,
0.799372799462109));
#12673=CARTESIAN_POINT('Ctrl Pts',(0.139691812633638,0.0684256315443816,
0.799332984548816));
#12674=CARTESIAN_POINT('Ctrl Pts',(0.139805540188643,0.0681929652020945,
0.799314334754582));
#12675=CARTESIAN_POINT('Ctrl Pts',(0.14006388166321,0.0676610818179139,
0.799271835528155));
#12676=CARTESIAN_POINT('Ctrl Pts',(0.140208118034519,0.0673616848225591,
0.799248009657173));
#12677=CARTESIAN_POINT('Ctrl Pts',(0.140587751108258,0.0665671637603513,
0.799185032373793));
#12678=CARTESIAN_POINT('Ctrl Pts',(0.140821494548802,0.0660712475263667,
0.799145980539543));
#12679=CARTESIAN_POINT('Ctrl Pts',(0.142415816649116,0.0626417941857988,
0.798877616826963));
#12680=CARTESIAN_POINT('Ctrl Pts',(0.143687376820304,0.0596674187302281,
0.798653387365905));
#12681=CARTESIAN_POINT('Ctrl Pts',(0.145165924370437,0.0558868299186629,
0.798376278328924));
#12682=CARTESIAN_POINT('Ctrl Pts',(0.145460347577447,0.0551159748852266,
0.7983201810209));
#12683=CARTESIAN_POINT('Ctrl Pts',(0.15008170145632,0.0427213984830013,
0.797424109162421));
#12684=CARTESIAN_POINT('Ctrl Pts',(0.15300952956646,0.0306229239145531,
0.796629134099632));
#12685=CARTESIAN_POINT('Ctrl Pts',(0.154977757385461,0.0140132086590769,
0.795510002567479));
#12686=CARTESIAN_POINT('Ctrl Pts',(0.155307185208447,0.00970302182048626,
0.79521753718701));
#12687=CARTESIAN_POINT('Ctrl Pts',(0.155547925680275,0.00275317695041912,
0.794738445293535));
#12688=CARTESIAN_POINT('Ctrl Pts',(0.155572238601344,0.000119635029152116,
0.794555186514293));
#12689=CARTESIAN_POINT('Ctrl Pts',(0.155516788792295,-0.00331198555048525,
0.79431360584295));
#12690=CARTESIAN_POINT('Ctrl Pts',(0.155497725947619,-0.00411072097472965,
0.794257180163994));
#12691=CARTESIAN_POINT('Ctrl Pts',(0.155456645201601,-0.00541171655463531,
0.794164938212319));
#12692=CARTESIAN_POINT('Ctrl Pts',(0.155438343978517,-0.00591408689546025,
0.794129238289805));
#12693=CARTESIAN_POINT('Ctrl Pts',(0.155398404274547,-0.00688151059171137,
0.794060329517132));
#12694=CARTESIAN_POINT('Ctrl Pts',(0.155377112495579,-0.00734657355316305,
0.794027131866808));
#12695=CARTESIAN_POINT('Ctrl Pts',(0.155323477785036,-0.00841324720877495,
0.793950821495057));
#12696=CARTESIAN_POINT('Ctrl Pts',(0.155289726863767,-0.00901477628714574,
0.793907665212274));
#12697=CARTESIAN_POINT('Ctrl Pts',(0.155190510014185,-0.0106166402521328,
0.793792405864537));
#12698=CARTESIAN_POINT('Ctrl Pts',(0.155118867785877,-0.0116165493168872,
0.793720110953034));
#12699=CARTESIAN_POINT('Ctrl Pts',(0.154485427316412,-0.0194010770670998,
0.793154472652925));
#12700=CARTESIAN_POINT('Ctrl Pts',(0.153488524643234,-0.0261418498296094,
0.792647555200766));
#12701=CARTESIAN_POINT('Ctrl Pts',(0.149098247854497,-0.0464974245144076,
0.791063655255003));
#12702=CARTESIAN_POINT('Ctrl Pts',(0.14430465426185,-0.059736316186918,
0.789953025093026));
#12703=CARTESIAN_POINT('Ctrl Pts',(0.136781677907786,-0.0741041370850376,
0.788738067490588));
#12704=CARTESIAN_POINT('Ctrl Pts',(0.135718961954988,-0.076032988018343,
0.788574922000234));
#12705=CARTESIAN_POINT('Ctrl Pts',(0.134358495576523,-0.0783827813864158,
0.788376698583588));
#12706=CARTESIAN_POINT('Ctrl Pts',(0.134099214983862,-0.0788255435261533,
0.788339371711147));
#12707=CARTESIAN_POINT('Ctrl Pts',(0.133687475256215,-0.0795207420331388,
0.788280810163883));
#12708=CARTESIAN_POINT('Ctrl Pts',(0.133536484198099,-0.0797740361637073,
0.788259483245344));
#12709=CARTESIAN_POINT('Ctrl Pts',(0.133251734654675,-0.0802486422257836,
0.788219542989181));
#12710=CARTESIAN_POINT('Ctrl Pts',(0.133118146222098,-0.0804700473184797,
0.788200919533595));
#12711=CARTESIAN_POINT('Ctrl Pts',(0.132810494090436,-0.0809770772155301,
0.788158289600803));
#12712=CARTESIAN_POINT('Ctrl Pts',(0.132636060972183,-0.0812624741832928,
0.788134307575406));
#12713=CARTESIAN_POINT('Ctrl Pts',(0.13209202594785,-0.0821461730290882,
0.788060084684401));
#12714=CARTESIAN_POINT('Ctrl Pts',(0.131719279150754,-0.0827425441493287,
0.788010044305072));
#12715=CARTESIAN_POINT('Ctrl Pts',(0.127644534946307,-0.089164553880836,
0.787471486488151));
#12716=CARTESIAN_POINT('Ctrl Pts',(0.123562153832671,-0.0947410595434836,
0.787006390933967));
#12717=CARTESIAN_POINT('Ctrl Pts',(0.113412838903229,-0.106827684865006,
0.785958630532125));
#12718=CARTESIAN_POINT('Ctrl Pts',(0.107131986916895,-0.113125441977779,
0.785381687976477));
#12719=CARTESIAN_POINT('Ctrl Pts',(0.0967835193588346,-0.12186269964518,
0.784477970004902));
#12720=CARTESIAN_POINT('Ctrl Pts',(0.0930855587242266,-0.124710224258607,
0.784163084549768));
#12721=CARTESIAN_POINT('Ctrl Pts',(0.0877587324118492,-0.128442954097473,
0.783715585541222));
#12722=CARTESIAN_POINT('Ctrl Pts',(0.0862334300851427,-0.129471937620841,
0.783588117719509));
#12723=CARTESIAN_POINT('Ctrl Pts',(0.0835357942098381,-0.131222970597773,
0.783363566231928));
#12724=CARTESIAN_POINT('Ctrl Pts',(0.0823714390042258,-0.131956973098525,
0.783266926512843));
#12725=CARTESIAN_POINT('Ctrl Pts',(0.0806672503466133,-0.132999938862592,
0.783125808822505));
#12726=CARTESIAN_POINT('Ctrl Pts',(0.080135037936016,-0.133321283712045,
0.78308178401757));
#12727=CARTESIAN_POINT('Ctrl Pts',(0.0791997804380966,-0.133878360019871,
0.783004491590087));
#12728=CARTESIAN_POINT('Ctrl Pts',(0.0787975708131618,-0.134115485042924,
0.782971275056694));
#12729=CARTESIAN_POINT('Ctrl Pts',(0.0780154280004287,-0.13457186895908,
0.782906723474683));
#12730=CARTESIAN_POINT('Ctrl Pts',(0.0776356224819512,-0.13479133887533,
0.782875396443397));
#12731=CARTESIAN_POINT('Ctrl Pts',(0.0767269771719916,-0.135311283453173,
0.782800491922773));
#12732=CARTESIAN_POINT('Ctrl Pts',(0.0761972968241275,-0.135610266546859,
0.782756861383812));
#12733=CARTESIAN_POINT('Ctrl Pts',(0.0742888151924397,-0.136672815728198,
0.782599767334483));
#12734=CARTESIAN_POINT('Ctrl Pts',(0.0729002228940245,-0.137418498696092,
0.78248567167684));
#12735=CARTESIAN_POINT('Ctrl Pts',(0.0706118758295029,-0.138602910796911,
0.782297911750962));
#12736=CARTESIAN_POINT('Ctrl Pts',(0.0697187671307334,-0.139054296277507,
0.782224697044403));
#12737=CARTESIAN_POINT('Ctrl Pts',(0.0681303428149257,-0.13983795142238,
0.782094585367641));
#12738=CARTESIAN_POINT('Ctrl Pts',(0.0674367890467702,-0.140173734039405,
0.782037809160768));
#12739=CARTESIAN_POINT('Ctrl Pts',(0.0662166273033565,-0.140753321432988,
0.781937980280856));
#12740=CARTESIAN_POINT('Ctrl Pts',(0.0656910917040262,-0.140999360567433,
0.781895001367356));
#12741=CARTESIAN_POINT('Ctrl Pts',(0.0650242859477797,-0.141307000814208,
0.781840491854575));
#12742=CARTESIAN_POINT('Ctrl Pts',(0.0648842785343968,-0.141371343068167,
0.781829047898492));
#12743=CARTESIAN_POINT('Ctrl Pts',(0.0646896543854195,-0.141460435143653,
0.781813141411207));
#12744=CARTESIAN_POINT('Ctrl Pts',(0.0646351182220086,-0.141485361744407,
0.781808684400974));
#12745=CARTESIAN_POINT('Ctrl Pts',(0.0515529581325114,-0.147455623864881,
0.780739580222501));
#12746=CARTESIAN_POINT('Ctrl Pts',(0.0377679009634067,-0.151572796241196,
0.779614413181161));
#12747=CARTESIAN_POINT('Ctrl Pts',(0.0201187780993151,-0.154284075085249,
0.778244404138055));
#12748=CARTESIAN_POINT('Ctrl Pts',(0.0166012349691905,-0.154702113430027,
0.77797525350488));
#12749=CARTESIAN_POINT('Ctrl Pts',(0.0111778435190974,-0.15515950686183,
0.777568955580236));
#12750=CARTESIAN_POINT('Ctrl Pts',(0.0092805598676607,-0.155284541596335,
0.777428446666504));
#12751=CARTESIAN_POINT('Ctrl Pts',(0.0068927935365231,-0.155397976564714,
0.777254037794324));
#12752=CARTESIAN_POINT('Ctrl Pts',(0.00640412442419206,-0.155418882156921,
0.777218471633737));
#12753=CARTESIAN_POINT('Ctrl Pts',(0.00562600500076877,-0.15544849440568,
0.777162050264291));
#12754=CARTESIAN_POINT('Ctrl Pts',(0.00533662056392088,-0.155458698148318,
0.777141113570064));
#12755=CARTESIAN_POINT('Ctrl Pts',(0.00478762127951809,-0.15547652117854,
0.777101484377287));
#12756=CARTESIAN_POINT('Ctrl Pts',(0.00452801919361408,-0.155484298238487,
0.777082783758662));
#12757=CARTESIAN_POINT('Ctrl Pts',(0.00393051748116529,-0.155500700250034,
0.777039829415925));
#12758=CARTESIAN_POINT('Ctrl Pts',(0.00359260825401031,-0.155508874080279,
0.777015601080654));
#12759=CARTESIAN_POINT('Ctrl Pts',(0.00268722705150434,-0.155527822090269,
0.776950849349461));
#12760=CARTESIAN_POINT('Ctrl Pts',(0.00211971098721477,-0.155536592109872,
0.776910434681687));
#12761=CARTESIAN_POINT('Ctrl Pts',(-0.00210115335165072,-0.155578711893932,
0.776611056855797));
#12762=CARTESIAN_POINT('Ctrl Pts',(-0.00575498535910577,-0.15548644970198,
0.776358597155457));
#12763=CARTESIAN_POINT('Ctrl Pts',(-0.0112980827973848,-0.155150772185236,
0.775981161612917));
#12764=CARTESIAN_POINT('Ctrl Pts',(-0.0131914376173044,-0.15500127500968,
0.775853232195567));
#12765=CARTESIAN_POINT('Ctrl Pts',(-0.0295991060914255,-0.153402908098742,
0.774749637375592));
#12766=CARTESIAN_POINT('Ctrl Pts',(-0.0438448907086237,-0.149953998417868,
0.773818113933568));
#12767=CARTESIAN_POINT('Ctrl Pts',(-0.0603302557095414,-0.143408467471548,
0.772601907898211));
#12768=CARTESIAN_POINT('Ctrl Pts',(-0.063222220694162,-0.142157225304195,
0.772383351094607));
#12769=CARTESIAN_POINT('Ctrl Pts',(-0.0668438866724197,-0.140457895692484,
0.772101996903965));
#12770=CARTESIAN_POINT('Ctrl Pts',(-0.0676107458562194,-0.14009037312098,
0.772041978666779));
#12771=CARTESIAN_POINT('Ctrl Pts',(-0.0688363051439574,-0.139490608601823,
0.771945327069034));
#12772=CARTESIAN_POINT('Ctrl Pts',(-0.069296942507977,-0.139262344305525,
0.77190883204996));
#12773=CARTESIAN_POINT('Ctrl Pts',(-0.0701698145683913,-0.138824398154907,
0.771839353218202));
#12774=CARTESIAN_POINT('Ctrl Pts',(-0.0705822630678265,-0.138615152603784,
0.771806384945972));
#12775=CARTESIAN_POINT('Ctrl Pts',(-0.0715185099331964,-0.138134908839416,
0.771731229221048));
#12776=CARTESIAN_POINT('Ctrl Pts',(-0.0720417098791794,-0.137862766268129,
0.771689001910026));
#12777=CARTESIAN_POINT('Ctrl Pts',(-0.0736318896006051,-0.137024109968243,
0.771559952344894));
#12778=CARTESIAN_POINT('Ctrl Pts',(-0.0746938060136661,-0.136448147912775,
0.771472797511643));
#12779=CARTESIAN_POINT('Ctrl Pts',(-0.0772647476860239,-0.135014715655852,
0.771259350217379));
#12780=CARTESIAN_POINT('Ctrl Pts',(-0.0787663059520426,-0.134144262922644,
0.77113260313));
#12781=CARTESIAN_POINT('Ctrl Pts',(-0.0925912967294179,-0.125817769953142,
0.769945723517359));
#12782=CARTESIAN_POINT('Ctrl Pts',(-0.10383574540402,-0.116709988593688,
0.768821737720165));
#12783=CARTESIAN_POINT('Ctrl Pts',(-0.116738583117244,-0.10289890668422,
0.767363211441435));
#12784=CARTESIAN_POINT('Ctrl Pts',(-0.119668737455807,-0.0994760356110558,
0.767018462642592));
#12785=CARTESIAN_POINT('Ctrl Pts',(-0.123822150326273,-0.094174591394553,
0.766513781260716));
#12786=CARTESIAN_POINT('Ctrl Pts',(-0.125160038838041,-0.0923890938442791,
0.76634845656961));
#12787=CARTESIAN_POINT('Ctrl Pts',(-0.126759137757643,-0.0901564690941939,
0.766147959126184));
#12788=CARTESIAN_POINT('Ctrl Pts',(-0.127057053304051,-0.0897361306863186,
0.7661104770143));
#12789=CARTESIAN_POINT('Ctrl Pts',(-0.127522463560698,-0.0890725042688893,
0.76605172697451));
#12790=CARTESIAN_POINT('Ctrl Pts',(-0.127691359454263,-0.0888302113811323,
0.766030365828257));
#12791=CARTESIAN_POINT('Ctrl Pts',(-0.128006789729661,-0.0883749461662716,
0.765990396820721));
#12792=CARTESIAN_POINT('Ctrl Pts',(-0.128153481558411,-0.0881620921527741,
0.765971778669144));
#12793=CARTESIAN_POINT('Ctrl Pts',(-0.128488338955865,-0.0876736028043386,
0.765929207171701));
#12794=CARTESIAN_POINT('Ctrl Pts',(-0.128676148384388,-0.0873977271955276,
0.765905278032215));
#12795=CARTESIAN_POINT('Ctrl Pts',(-0.129254798523519,-0.0865418322503385,
0.765831381176145));
#12796=CARTESIAN_POINT('Ctrl Pts',(-0.1296426237012,-0.0859597687272538,
0.765781611419586));
#12797=CARTESIAN_POINT('Ctrl Pts',(-0.133444714767209,-0.0801691728839793,
0.765291049750526));
#12798=CARTESIAN_POINT('Ctrl Pts',(-0.136547691992521,-0.0747618785240991,
0.764869276763085));
#12799=CARTESIAN_POINT('Ctrl Pts',(-0.140424437915346,-0.0669549424434565,
0.76428857545107));
#12800=CARTESIAN_POINT('Ctrl Pts',(-0.141476951996176,-0.0647013112755856,
0.764124074343465));
#12801=CARTESIAN_POINT('Ctrl Pts',(-0.145695951793674,-0.0550718725152586,
0.763430601390425));
#12802=CARTESIAN_POINT('Ctrl Pts',(-0.148342966282279,-0.0474824152885466,
0.762906312659745));
#12803=CARTESIAN_POINT('Ctrl Pts',(-0.15195045667767,-0.0338242616384623,
0.76195880842185));
#12804=CARTESIAN_POINT('Ctrl Pts',(-0.153159867661364,-0.0278399330092353,
0.761542520224111));
#12805=CARTESIAN_POINT('Ctrl Pts',(-0.154158837767367,-0.0207825048141482,
0.761042573029926));
#12806=CARTESIAN_POINT('Ctrl Pts',(-0.154292845160762,-0.0197630364581568,
0.760970145401697));
#12807=CARTESIAN_POINT('Ctrl Pts',(-0.154483351593567,-0.0181934679079019,
0.760858283341127));
#12808=CARTESIAN_POINT('Ctrl Pts',(-0.15454704279997,-0.0176442551995465,
0.760819075118087));
#12809=CARTESIAN_POINT('Ctrl Pts',(-0.154657849414168,-0.0166420997802093,
0.760747405397276));
#12810=CARTESIAN_POINT('Ctrl Pts',(-0.154705906630079,-0.016189265461627,
0.760714973859669));
#12811=CARTESIAN_POINT('Ctrl Pts',(-0.154806477594729,-0.0152002385909582,
0.760644035308861));
#12812=CARTESIAN_POINT('Ctrl Pts',(-0.154858195272737,-0.0146639729231184,
0.760605503745893));
#12813=CARTESIAN_POINT('Ctrl Pts',(-0.154992201550675,-0.0131945981169751,
0.760499735612869));
#12814=CARTESIAN_POINT('Ctrl Pts',(-0.155068847639527,-0.0122610106195149,
0.7604323233414));
#12815=CARTESIAN_POINT('Ctrl Pts',(-0.155414542529894,-0.00752621732812435,
0.760089314549051));
#12816=CARTESIAN_POINT('Ctrl Pts',(-0.155552250998398,-0.00371705200902001,
0.7598096602253));
#12817=CARTESIAN_POINT('Ctrl Pts',(-0.155541110402596,0.0149096492034718,
0.758422610536678));
#12818=CARTESIAN_POINT('Ctrl Pts',(-0.153415077015676,0.029647957652074,
0.757254684268284));
#12819=CARTESIAN_POINT('Ctrl Pts',(-0.147988193807677,0.0481141380828599,
0.755783922740216));
#12820=CARTESIAN_POINT('Ctrl Pts',(-0.146555982731543,0.0523147091798366,
0.755449689641221));
#12821=CARTESIAN_POINT('Ctrl Pts',(-0.144706278994157,0.0570642765115517,
0.755076336933976));
#12822=CARTESIAN_POINT('Ctrl Pts',(-0.144462640524784,0.0576782833369183,
0.75502816176344));
#12823=CARTESIAN_POINT('Ctrl Pts',(-0.144092904592088,0.0585930342396851,
0.754956545089647));
#12824=CARTESIAN_POINT('Ctrl Pts',(-0.143969765240692,0.058894953239144,
0.754932932924854));
#12825=CARTESIAN_POINT('Ctrl Pts',(-0.143747561398075,0.0594349018711088,
0.754890753466581));
#12826=CARTESIAN_POINT('Ctrl Pts',(-0.143648854107371,0.0596730733706338,
0.75487216514607));
#12827=CARTESIAN_POINT('Ctrl Pts',(-0.143433787027275,0.0601883840977885,
0.754831984529495));
#12828=CARTESIAN_POINT('Ctrl Pts',(-0.14331721631369,0.0604654310623273,
0.754810405251202));
#12829=CARTESIAN_POINT('Ctrl Pts',(-0.142989368791817,0.0612383329075057,
0.754750263399946));
#12830=CARTESIAN_POINT('Ctrl Pts',(-0.142776313920289,0.0617334367346935,
0.754711806699295));
#12831=CARTESIAN_POINT('Ctrl Pts',(-0.141525570992927,0.0645988412845397,
0.754489582247166));
#12832=CARTESIAN_POINT('Ctrl Pts',(-0.14043136454327,0.0669442417802616,
0.754309051192415));
#12833=CARTESIAN_POINT('Ctrl Pts',(-0.132724621279661,0.082441871521703,
0.753118128068271));
#12834=CARTESIAN_POINT('Ctrl Pts',(-0.124331899563472,0.094626504330818,
0.752185020633095));
#12835=CARTESIAN_POINT('Ctrl Pts',(-0.113061510702215,0.106848074958021,
0.751068075083847));
#12836=CARTESIAN_POINT('Ctrl Pts',(-0.111747307059217,0.108221787466916,
0.750939644489558));
#12837=CARTESIAN_POINT('Ctrl Pts',(-0.107574890917782,0.112426086162214,
0.750536708609445));
#12838=CARTESIAN_POINT('Ctrl Pts',(-0.104632046356623,0.115169927026694,
0.750259256634307));
#12839=CARTESIAN_POINT('Ctrl Pts',(-0.100928498481501,0.118363826468811,
0.749915917372416));
#12840=CARTESIAN_POINT('Ctrl Pts',(-0.100265875354558,0.118925654956956,
0.749854707426298));
#12841=CARTESIAN_POINT('Ctrl Pts',(-0.0991619669570246,0.119845859010989,
0.749753072126332));
#12842=CARTESIAN_POINT('Ctrl Pts',(-0.0987233548899906,0.120207424049308,
0.7497127767447));
#12843=CARTESIAN_POINT('Ctrl Pts',(-0.0979258540281336,0.12085752628741,
0.749639661195743));
#12844=CARTESIAN_POINT('Ctrl Pts',(-0.0975676452605391,0.121146890745929,
0.74960687483169));
#12845=CARTESIAN_POINT('Ctrl Pts',(-0.0967961294994244,0.121764487314958,
0.749536372280422));
#12846=CARTESIAN_POINT('Ctrl Pts',(-0.0963824273403182,0.122092214102517,
0.749498636471835));
#12847=CARTESIAN_POINT('Ctrl Pts',(-0.095249097409192,0.122980666028845,
0.749395441736298));
#12848=CARTESIAN_POINT('Ctrl Pts',(-0.0945262017524837,0.123537168052934,
0.749329817114607));
#12849=CARTESIAN_POINT('Ctrl Pts',(-0.0906718212744912,0.126450722236682,
0.748980908209767));
#12850=CARTESIAN_POINT('Ctrl Pts',(-0.0874572513636142,0.128694943135836,
0.748693299755616));
#12851=CARTESIAN_POINT('Ctrl Pts',(-0.077615623880683,0.135026678807705,
0.747821586081134));
#12852=CARTESIAN_POINT('Ctrl Pts',(-0.0707711937600463,0.138735384551554,
0.74722608401625));
#12853=CARTESIAN_POINT('Ctrl Pts',(-0.0636886011499548,0.141913933718863,
0.746625191472247));
#12854=CARTESIAN_POINT('',(-0.155550013165998,8.25752365483191E-5,0.745715654272581));
#12855=CARTESIAN_POINT('Ctrl Pts',(-0.0636886287602419,0.141913921327825,
0.732917465391055));
#12856=CARTESIAN_POINT('Ctrl Pts',(-0.0658868196071155,0.140927409507978,
0.733098854558852));
#12857=CARTESIAN_POINT('Ctrl Pts',(-0.0680624092442903,0.139889680523272,
0.733278291559734));
#12858=CARTESIAN_POINT('Ctrl Pts',(-0.0708388259518219,0.138485212855949,
0.733506388586994));
#12859=CARTESIAN_POINT('Ctrl Pts',(-0.071461926926368,0.138164707837504,
0.733557520036753));
#12860=CARTESIAN_POINT('Ctrl Pts',(-0.0723787520957292,0.137685257899643,
0.733632643283517));
#12861=CARTESIAN_POINT('Ctrl Pts',(-0.0726741524091138,0.137529566185343,
0.733656830780006));
#12862=CARTESIAN_POINT('Ctrl Pts',(-0.0731883917908159,0.137256415116443,
0.733698903986489));
#12863=CARTESIAN_POINT('Ctrl Pts',(-0.0734074529175393,0.137139381810263,
0.733716816203875));
#12864=CARTESIAN_POINT('Ctrl Pts',(-0.0736269661597238,0.137021430275701,
0.733734754444373));
#12865=CARTESIAN_POINT('Ctrl Pts',(-0.0736276946533431,0.137021038825177,
0.733734813975475));
#12866=CARTESIAN_POINT('Ctrl Pts',(-0.0736291513747163,0.13702025605188,
0.733734933015738));
#12867=CARTESIAN_POINT('Ctrl Pts',(-0.0736298762907878,0.137019866508793,
0.733734992254266));
#12868=CARTESIAN_POINT('Ctrl Pts',(-0.0736313216189784,0.137019089828089,
0.733735110363035));
#12869=CARTESIAN_POINT('Ctrl Pts',(-0.0736320419228137,0.137018702748759,
0.733735169224429));
#12870=CARTESIAN_POINT('Ctrl Pts',(-0.0736334780672034,0.137017930973993,
0.733735286582259));
#12871=CARTESIAN_POINT('Ctrl Pts',(-0.0736341937935272,0.137017546340039,
0.73373534506936));
#12872=CARTESIAN_POINT('Ctrl Pts',(-0.0736356208233877,0.13701677943454,
0.73373546168192));
#12873=CARTESIAN_POINT('Ctrl Pts',(-0.0736363320090056,0.137016397226459,
0.733735519797743));
#12874=CARTESIAN_POINT('Ctrl Pts',(-0.0736377499825418,0.137015635159494,
0.733735635669798));
#12875=CARTESIAN_POINT('Ctrl Pts',(-0.0736384566581405,0.137015255361068,
0.733735693416853));
#12876=CARTESIAN_POINT('Ctrl Pts',(-0.0736398656455024,0.137014498095477,
0.733735808554144));
#12877=CARTESIAN_POINT('Ctrl Pts',(-0.0736405678422688,0.137014120690211,
0.733735865934984));
#12878=CARTESIAN_POINT('Ctrl Pts',(-0.0736419693503222,0.137013367416629,
0.733735980460655));
#12879=CARTESIAN_POINT('Ctrl Pts',(-0.0736426685448713,0.137012991611061,
0.733736037595963));
#12880=CARTESIAN_POINT('Ctrl Pts',(-0.0736440569327213,0.137012245361901,
0.733736151049072));
#12881=CARTESIAN_POINT('Ctrl Pts',(-0.0736447503153976,0.137011872666577,
0.733736207709228));
#12882=CARTESIAN_POINT('Ctrl Pts',(-0.0736461327094075,0.137011129612014,
0.733736320672119));
#12883=CARTESIAN_POINT('Ctrl Pts',(-0.0736468217146804,0.137010759256118,
0.733736376974361));
#12884=CARTESIAN_POINT('Ctrl Pts',(-0.0736481953872075,0.137010020862753,
0.733736489224152));
#12885=CARTESIAN_POINT('Ctrl Pts',(-0.0736488800500122,0.137009652827759,
0.733736545171339));
#12886=CARTESIAN_POINT('Ctrl Pts',(-0.0736502450542464,0.137008919067505,
0.733736656712383));
#12887=CARTESIAN_POINT('Ctrl Pts',(-0.073650925401184,0.137008553339366,
0.733736712306692));
#12888=CARTESIAN_POINT('Ctrl Pts',(-0.0736522818143393,0.137007824171214,
0.733736823145308));
#12889=CARTESIAN_POINT('Ctrl Pts',(-0.0736529578801308,0.137007460731512,
0.733736878389581));
#12890=CARTESIAN_POINT('Ctrl Pts',(-0.0736543057557409,0.137006736127176,
0.733736988530151));
#12891=CARTESIAN_POINT('Ctrl Pts',(-0.0736549775684109,0.13700637496109,
0.733737043426682));
#12892=CARTESIAN_POINT('Ctrl Pts',(-0.07365631697955,0.13700565488177,0.733737152875184));
#12893=CARTESIAN_POINT('Ctrl Pts',(-0.0736569845740336,0.137005295970758,
0.733737207426831));
#12894=CARTESIAN_POINT('Ctrl Pts',(-0.0736583155734067,0.137004580388598,
0.73373731618758));
#12895=CARTESIAN_POINT('Ctrl Pts',(-0.0736589789788319,0.137004223717239,
0.733737370396727));
#12896=CARTESIAN_POINT('Ctrl Pts',(-0.073660301632553,0.137003512597165,
0.733737478475132));
#12897=CARTESIAN_POINT('Ctrl Pts',(-0.0736609608805821,0.13700315814867,
0.733737532344371));
#12898=CARTESIAN_POINT('Ctrl Pts',(-0.0736622752456853,0.137002451460484,
0.733737639745101));
#12899=CARTESIAN_POINT('Ctrl Pts',(-0.0736629303647093,0.137002099219819,
0.733737693276754));
#12900=CARTESIAN_POINT('Ctrl Pts',(-0.0736642365069524,0.137001396928623,
0.73373780000519));
#12901=CARTESIAN_POINT('Ctrl Pts',(-0.0736648875282756,0.137001046879186,
0.73373785320182));
#12902=CARTESIAN_POINT('Ctrl Pts',(-0.0736661855103606,0.137000348951719,
0.733737959263092));
#12903=CARTESIAN_POINT('Ctrl Pts',(-0.0736668324687862,0.137000001075019,
0.733738012127545));
#12904=CARTESIAN_POINT('Ctrl Pts',(-0.0739239134974,0.136861763415723,0.733759018769638));
#12905=CARTESIAN_POINT('Ctrl Pts',(-0.0741799627949866,0.136723152375748,
0.733779926514437));
#12906=CARTESIAN_POINT('Ctrl Pts',(-0.0748786279704719,0.136342392942848,
0.733836940432022));
#12907=CARTESIAN_POINT('Ctrl Pts',(-0.0753204626956025,0.136098805866748,
0.733872956663408));
#12908=CARTESIAN_POINT('Ctrl Pts',(-0.0763041978149138,0.135550206797253,
0.733953076125712));
#12909=CARTESIAN_POINT('Ctrl Pts',(-0.0768454737280182,0.135244084409275,
0.733997112211482));
#12910=CARTESIAN_POINT('Ctrl Pts',(-0.0785060874229395,0.134291724297996,
0.734132112599383));
#12911=CARTESIAN_POINT('Ctrl Pts',(-0.0796192512344375,0.133634756243729,
0.734222466151496));
#12912=CARTESIAN_POINT('Ctrl Pts',(-0.0838562748442795,0.131062404452488,
0.734566350561137));
#12913=CARTESIAN_POINT('Ctrl Pts',(-0.0869204983846739,0.129050610064148,
0.734815001678183));
#12914=CARTESIAN_POINT('Ctrl Pts',(-0.0977256739393813,0.121396888921269,
0.735702516373472));
#12915=CARTESIAN_POINT('Ctrl Pts',(-0.105012667391308,0.115151494326533,
0.736322957523172));
#12916=CARTESIAN_POINT('Ctrl Pts',(-0.117124236043512,0.10265917083873,
0.737478845861239));
#12917=CARTESIAN_POINT('Ctrl Pts',(-0.122137070180012,0.0966410904870666,
0.73800717596665));
#12918=CARTESIAN_POINT('Ctrl Pts',(-0.127270881815958,0.0894369999562729,
0.738626702342981));
#12919=CARTESIAN_POINT('Ctrl Pts',(-0.127857782842325,0.088595945713987,
0.738698830534396));
#12920=CARTESIAN_POINT('Ctrl Pts',(-0.128779932887381,0.0872462172202169,
0.738814300794546));
#12921=CARTESIAN_POINT('Ctrl Pts',(-0.129120592126282,0.0867412600990741,
0.738857438314034));
#12922=CARTESIAN_POINT('Ctrl Pts',(-0.129716881011497,0.0858460883448823,
0.738933809255411));
#12923=CARTESIAN_POINT('Ctrl Pts',(-0.12997373932828,0.0854566976884622,
0.738966996132539));
#12924=CARTESIAN_POINT('Ctrl Pts',(-0.130502050164645,0.0846479000879931,
0.739035861903078));
#12925=CARTESIAN_POINT('Ctrl Pts',(-0.13077324105906,0.0842283295492287,
0.739071550041686));
#12926=CARTESIAN_POINT('Ctrl Pts',(-0.131465500655869,0.0831459037549432,
0.739163530832447));
#12927=CARTESIAN_POINT('Ctrl Pts',(-0.131883574980984,0.0824811601651463,
0.739219933272772));
#12928=CARTESIAN_POINT('Ctrl Pts',(-0.133617705970058,0.0796769749716854,
0.739457534509738));
#12929=CARTESIAN_POINT('Ctrl Pts',(-0.13488680548366,0.077509096415319,
0.739640430414));
#12930=CARTESIAN_POINT('Ctrl Pts',(-0.138062650781598,0.0717697191835356,
0.740122949748545));
#12931=CARTESIAN_POINT('Ctrl Pts',(-0.139883330741691,0.068153038618028,
0.740425390804462));
#12932=CARTESIAN_POINT('Ctrl Pts',(-0.147000785032031,0.0525247438556022,
0.741725257506989));
#12933=CARTESIAN_POINT('Ctrl Pts',(-0.150906399022489,0.0399409552940836,
0.742760508761882));
#12934=CARTESIAN_POINT('Ctrl Pts',(-0.153513178247386,0.0251606928274965,
0.743901568080885));
#12935=CARTESIAN_POINT('Ctrl Pts',(-0.153806848468763,0.0232982913102516,
0.744043910567974));
#12936=CARTESIAN_POINT('Ctrl Pts',(-0.154146351899127,0.0208576066405569,
0.744228218212873));
#12937=CARTESIAN_POINT('Ctrl Pts',(-0.154222902538861,0.0202838338052238,
0.744271385766656));
#12938=CARTESIAN_POINT('Ctrl Pts',(-0.154491345450532,0.0181823372761071,
0.74442887259747));
#12939=CARTESIAN_POINT('Ctrl Pts',(-0.154663763591989,0.0166521448237655,
0.744542351714121));
#12940=CARTESIAN_POINT('Ctrl Pts',(-0.154859417385346,0.0146487914606559,
0.744689150924813));
#12941=CARTESIAN_POINT('Ctrl Pts',(-0.154903248054186,0.0141777996257191,
0.744723536089202));
#12942=CARTESIAN_POINT('Ctrl Pts',(-0.154970124340366,0.0134218035172789,
0.744778515905987));
#12943=CARTESIAN_POINT('Ctrl Pts',(-0.154994533366409,0.0131369280225778,
0.744799185147332));
#12944=CARTESIAN_POINT('Ctrl Pts',(-0.155038717563621,0.0126039867289663,
0.7448377605169));
#12945=CARTESIAN_POINT('Ctrl Pts',(-0.155058682692638,0.0123559438278507,
0.744855676729856));
#12946=CARTESIAN_POINT('Ctrl Pts',(-0.155097922028982,0.011853364064749,
0.744891903455346));
#12947=CARTESIAN_POINT('Ctrl Pts',(-0.155117164896952,0.0115988281403929,
0.744910212052376));
#12948=CARTESIAN_POINT('Ctrl Pts',(-0.15516028559773,0.0110091401994567,
0.744952540600203));
#12949=CARTESIAN_POINT('Ctrl Pts',(-0.155183704369946,0.0106739542026328,
0.744976535382325));
#12950=CARTESIAN_POINT('Ctrl Pts',(-0.155241700513122,0.00980330706539756,
0.745038698609322));
#12951=CARTESIAN_POINT('Ctrl Pts',(-0.155274594083551,0.00926773227578935,
0.74507677770032));
#12952=CARTESIAN_POINT('Ctrl Pts',(-0.155466653342219,0.00585181955296553,
0.745318687248882));
#12953=CARTESIAN_POINT('Ctrl Pts',(-0.155548450466375,0.00296749491786026,
0.745518602194368));
#12954=CARTESIAN_POINT('Ctrl Pts',(-0.155549978192756,8.23664555785925E-5,
0.745715729333107));
#12955=CARTESIAN_POINT('Ctrl Pts',(-0.155549978079878,8.25793517535353E-5,
0.745715714786916));
#12956=CARTESIAN_POINT('Ctrl Pts',(-0.155556853675459,-0.0128685848205831,
0.746600607013714));
#12957=CARTESIAN_POINT('Ctrl Pts',(-0.15394629247449,-0.0257717735182719,
0.747428745924574));
#12958=CARTESIAN_POINT('Ctrl Pts',(-0.149220890194732,-0.0443581414932631,
0.748709406296978));
#12959=CARTESIAN_POINT('Ctrl Pts',(-0.147327452226894,-0.0502904133857493,
0.74913151030482));
#12960=CARTESIAN_POINT('Ctrl Pts',(-0.144555614530026,-0.0574597637479467,
0.749667613277752));
#12961=CARTESIAN_POINT('Ctrl Pts',(-0.144007872702005,-0.058819065656376,
0.749770433443441));
#12962=CARTESIAN_POINT('Ctrl Pts',(-0.143194412099914,-0.0607582857442818,
0.749918909348949));
#12963=CARTESIAN_POINT('Ctrl Pts',(-0.142944192343963,-0.0613446558102792,
0.749964041898562));
#12964=CARTESIAN_POINT('Ctrl Pts',(-0.142503493861355,-0.0623600599469477,
0.750042617960528));
#12965=CARTESIAN_POINT('Ctrl Pts',(-0.142314663107363,-0.0627898040694738,
0.750076005092705));
#12966=CARTESIAN_POINT('Ctrl Pts',(-0.141947373841504,-0.0636155185224228,
0.750140412923053));
#12967=CARTESIAN_POINT('Ctrl Pts',(-0.141769196103932,-0.0640116096217815,
0.750171423764564));
#12968=CARTESIAN_POINT('Ctrl Pts',(-0.141297017472815,-0.0650496261149102,
0.750252997356559));
#12969=CARTESIAN_POINT('Ctrl Pts',(-0.141000303660039,-0.065690298687884,
0.750303652880535));
#12970=CARTESIAN_POINT('Ctrl Pts',(-0.139950321550031,-0.0679175577687259,
0.750480846203047));
#12971=CARTESIAN_POINT('Ctrl Pts',(-0.139174577777274,-0.0694933348297017,
0.750608156344875));
#12972=CARTESIAN_POINT('Ctrl Pts',(-0.13349409367168,-0.0805554064374866,
0.751516153660548));
#12973=CARTESIAN_POINT('Ctrl Pts',(-0.127651511328569,-0.0895257062755262,
0.752330599354084));
#12974=CARTESIAN_POINT('Ctrl Pts',(-0.117010113811023,-0.102681266320282,
0.753641065290989));
#12975=CARTESIAN_POINT('Ctrl Pts',(-0.112793330642627,-0.107296213723833,
0.754127125459592));
#12976=CARTESIAN_POINT('Ctrl Pts',(-0.105919506967761,-0.113964718411044,
0.754860723414654));
#12977=CARTESIAN_POINT('Ctrl Pts',(-0.103454519627854,-0.116206990704938,
0.755113481581829));
#12978=CARTESIAN_POINT('Ctrl Pts',(-0.0999970293591358,-0.119154795676602,
0.755452335202484));
#12979=CARTESIAN_POINT('Ctrl Pts',(-0.0990656156982189,-0.119930293191213,
0.755542138252442));
#12980=CARTESIAN_POINT('Ctrl Pts',(-0.0976644579142919,-0.121069437740297,
0.755674931246396));
#12981=CARTESIAN_POINT('Ctrl Pts',(-0.0972015665344496,-0.121441387455473,
0.755718434035197));
#12982=CARTESIAN_POINT('Ctrl Pts',(-0.0963591599275317,-0.122110388752919,
0.755796924755105));
#12983=CARTESIAN_POINT('Ctrl Pts',(-0.0959803753407263,-0.122408342482916,
0.755831972000189));
#12984=CARTESIAN_POINT('Ctrl Pts',(-0.0953729661787505,-0.122881580411988,
0.755887773470156));
#12985=CARTESIAN_POINT('Ctrl Pts',(-0.0951452330586423,-0.123057994913729,
0.755908605872835));
#12986=CARTESIAN_POINT('Ctrl Pts',(-0.0947224800282469,-0.123383607369907,
0.755947111653722));
#12987=CARTESIAN_POINT('Ctrl Pts',(-0.0945275992113327,-0.123532974460131,
0.755964796656662));
#12988=CARTESIAN_POINT('Ctrl Pts',(-0.0940711323089854,-0.123881122464299,
0.756006068536476));
#12989=CARTESIAN_POINT('Ctrl Pts',(-0.0938092696723706,-0.124079536450808,
0.756029629529322));
#12990=CARTESIAN_POINT('Ctrl Pts',(-0.0930088493814255,-0.124682034621621,
0.756101302298344));
#12991=CARTESIAN_POINT('Ctrl Pts',(-0.0924682853137486,-0.12508346044055,
0.75614923285879));
#12992=CARTESIAN_POINT('Ctrl Pts',(-0.0879959686971424,-0.128359789228604,
0.756542059500712));
#12993=CARTESIAN_POINT('Ctrl Pts',(-0.0839332856556553,-0.131052437568517,
0.756875381402291));
#12994=CARTESIAN_POINT('Ctrl Pts',(-0.0707747838078598,-0.138910125620825,
0.757905854604968));
#12995=CARTESIAN_POINT('Ctrl Pts',(-0.0612813702914252,-0.143351694687048,
0.758581099640804));
#12996=CARTESIAN_POINT('Ctrl Pts',(-0.0450135437998744,-0.149048884657759,
0.759728422725725));
#12997=CARTESIAN_POINT('Ctrl Pts',(-0.0384744050131824,-0.150869118422769,
0.760186842136539));
#12998=CARTESIAN_POINT('Ctrl Pts',(-0.0303357676596908,-0.152570963627185,
0.760766282235592));
#12999=CARTESIAN_POINT('Ctrl Pts',(-0.0288290612976303,-0.152862823052504,
0.760873897590779));
#13000=CARTESIAN_POINT('Ctrl Pts',(-0.0266789515540542,-0.15324639590601,
0.761028062431324));
#13001=CARTESIAN_POINT('Ctrl Pts',(-0.0260388746616454,-0.153356451763358,
0.761074031013052));
#13002=CARTESIAN_POINT('Ctrl Pts',(-0.0249329514654142,-0.153539482723705,
0.761153592257944));
#13003=CARTESIAN_POINT('Ctrl Pts',(-0.0244674240336009,-0.153614354720019,
0.761187124514826));
#13004=CARTESIAN_POINT('Ctrl Pts',(-0.0235750981601126,-0.153753710716794,
0.761251482506231));
#13005=CARTESIAN_POINT('Ctrl Pts',(-0.0231483569175283,-0.153818537171378,
0.761282297088505));
#13006=CARTESIAN_POINT('Ctrl Pts',(-0.0220373166845191,-0.153982587598456,
0.761362621923545));
#13007=CARTESIAN_POINT('Ctrl Pts',(-0.0213526226194976,-0.15407902546687,
0.761412219528569));
#13008=CARTESIAN_POINT('Ctrl Pts',(-0.0190128809935731,-0.154392678609546,
0.76158204843877));
#13009=CARTESIAN_POINT('Ctrl Pts',(-0.0173550432431517,-0.154587809746761,
0.761702969280892));
#13010=CARTESIAN_POINT('Ctrl Pts',(-0.00270078989406502,-0.156073955986166,
0.762777420994795));
#13011=CARTESIAN_POINT('Ctrl Pts',(0.010404389635215,-0.155749711482677,
0.763783662581983));
#13012=CARTESIAN_POINT('Ctrl Pts',(0.0312462930030291,-0.152590559824126,
0.76541814411691));
#13013=CARTESIAN_POINT('Ctrl Pts',(0.0390770468872219,-0.150775409498959,
0.766038588046395));
#13014=CARTESIAN_POINT('Ctrl Pts',(0.0475331000389493,-0.14811181502562,
0.76669462996299));
#13015=CARTESIAN_POINT('Ctrl Pts',(0.0483307028768224,-0.147853469990355,
0.766756362153185));
#13016=CARTESIAN_POINT('Ctrl Pts',(0.0495594885391126,-0.147444457797167,
0.766851197318819));
#13017=CARTESIAN_POINT('Ctrl Pts',(0.0499921468907001,-0.147298324166876,
0.766884537127157));
#13018=CARTESIAN_POINT('Ctrl Pts',(0.0507106981471287,-0.14705209735635,
0.766939813726873));
#13019=CARTESIAN_POINT('Ctrl Pts',(0.0509969496684277,-0.146953072006535,
0.766961809657108));
#13020=CARTESIAN_POINT('Ctrl Pts',(0.0515511604380897,-0.146759534916859,
0.767004345389014));
#13021=CARTESIAN_POINT('Ctrl Pts',(0.0518191533043671,-0.14666512395893,
0.76702489090427));
#13022=CARTESIAN_POINT('Ctrl Pts',(0.0523231756130922,-0.14648600846526,
0.767063486229943));
#13023=CARTESIAN_POINT('Ctrl Pts',(0.0525592559546091,-0.14640146856186,
0.767081545004875));
#13024=CARTESIAN_POINT('Ctrl Pts',(0.0531098822975063,-0.146202786791173,
0.767123621745067));
#13025=CARTESIAN_POINT('Ctrl Pts',(0.0534242651829672,-0.146088200613596,
0.767147613066528));
#13026=CARTESIAN_POINT('Ctrl Pts',(0.0543991799857938,-0.145729295964849,
0.767221917151304));
#13027=CARTESIAN_POINT('Ctrl Pts',(0.055058436845694,-0.145481500775259,
0.767272028738349));
#13028=CARTESIAN_POINT('Ctrl Pts',(0.0624055939506118,-0.142662824135343,
0.767829243674299));
#13029=CARTESIAN_POINT('Ctrl Pts',(0.068910965225607,-0.139636852474163,
0.76831108731601));
#13030=CARTESIAN_POINT('Ctrl Pts',(0.0827584142275593,-0.131991220583771,
0.769359922734358));
#13031=CARTESIAN_POINT('Ctrl Pts',(0.0899693779636657,-0.127185490687428,
0.769922567487994));
#13032=CARTESIAN_POINT('Ctrl Pts',(0.101693326904764,-0.117873776491494,
0.770921776088418));
#13033=CARTESIAN_POINT('Ctrl Pts',(0.106398382466766,-0.113644747375297,
0.771350325729344));
#13034=CARTESIAN_POINT('Ctrl Pts',(0.111869795767525,-0.108088554786076,
0.771894117673135));
#13035=CARTESIAN_POINT('Ctrl Pts',(0.112891715704575,-0.107020779021166,
0.771997803076025));
#13036=CARTESIAN_POINT('Ctrl Pts',(0.114333916121706,-0.105470220226416,
0.772147307165418));
#13037=CARTESIAN_POINT('Ctrl Pts',(0.114766697052267,-0.104999128358048,
0.772192592469312));
#13038=CARTESIAN_POINT('Ctrl Pts',(0.115512233795035,-0.104177478551907,
0.772271347954059));
#13039=CARTESIAN_POINT('Ctrl Pts',(0.115826332675114,-0.103828145721331,
0.77230476102306));
#13040=CARTESIAN_POINT('Ctrl Pts',(0.116427425445298,-0.103153503543321,
0.772369157302719));
#13041=CARTESIAN_POINT('Ctrl Pts',(0.116714650808961,-0.102828405455886,
0.772400130415386));
#13042=CARTESIAN_POINT('Ctrl Pts',(0.117463938886023,-0.101973134434213,
0.772481465697885));
#13043=CARTESIAN_POINT('Ctrl Pts',(0.117923768022064,-0.101441027155288,
0.772531919599824));
#13044=CARTESIAN_POINT('Ctrl Pts',(0.11950870162044,-0.0995816262723197,
0.772707728197258));
#13045=CARTESIAN_POINT('Ctrl Pts',(0.120615094335134,-0.0982386309734471,
0.772833839393779));
#13046=CARTESIAN_POINT('Ctrl Pts',(0.129031178712947,-0.0876662341274678,
0.77382035741648));
#13047=CARTESIAN_POINT('Ctrl Pts',(0.135292697004802,-0.0776542807933108,
0.774722566529805));
#13048=CARTESIAN_POINT('Ctrl Pts',(0.142639297104381,-0.0622711754104519,
0.77604442713586));
#13049=CARTESIAN_POINT('Ctrl Pts',(0.144670329487358,-0.0573948408394731,
0.776454280726952));
#13050=CARTESIAN_POINT('Ctrl Pts',(0.147922236439142,-0.0483105401481043,
0.7771929533274));
#13051=CARTESIAN_POINT('Ctrl Pts',(0.14922108313896,-0.0441358460368841,
0.777523220145323));
#13052=CARTESIAN_POINT('Ctrl Pts',(0.15057723397387,-0.0390273751942305,
0.777912244373114));
#13053=CARTESIAN_POINT('Ctrl Pts',(0.150804166019929,-0.0381410936575152,
0.777979193991493));
#13054=CARTESIAN_POINT('Ctrl Pts',(0.151112391534664,-0.0368915450473225,
0.778072773973506));
#13055=CARTESIAN_POINT('Ctrl Pts',(0.151200214830678,-0.0365299331270809,
0.778099760315207));
#13056=CARTESIAN_POINT('Ctrl Pts',(0.15134818898269,-0.0359109737036286,
0.778145785365745));
#13057=CARTESIAN_POINT('Ctrl Pts',(0.15140898285055,-0.0356537832095708,
0.778164860615984));
#13058=CARTESIAN_POINT('Ctrl Pts',(0.151524688081587,-0.0351586551006461,
0.778201487260176));
#13059=CARTESIAN_POINT('Ctrl Pts',(0.151579694723989,-0.0349207427806138,
0.77821904423203));
#13060=CARTESIAN_POINT('Ctrl Pts',(0.151724730578397,-0.0342866402606119,
0.778265728072107));
#13061=CARTESIAN_POINT('Ctrl Pts',(0.151813769042295,-0.0338902214313781,
0.778294798544624));
#13062=CARTESIAN_POINT('Ctrl Pts',(0.152128235824517,-0.0324640352510709,
0.778398988106287));
#13063=CARTESIAN_POINT('Ctrl Pts',(0.152344755071913,-0.0314323000054422,
0.778473619215755));
#13064=CARTESIAN_POINT('Ctrl Pts',(0.152612994249233,-0.0300861736746981,
0.778570123937446));
#13065=CARTESIAN_POINT('Ctrl Pts',(0.152674253895215,-0.0297737478619322,
0.77859246128141));
#13066=CARTESIAN_POINT('Ctrl Pts',(0.15281520101481,-0.029043039524621,
0.77864456734425));
#13067=CARTESIAN_POINT('Ctrl Pts',(0.152894131498634,-0.0286246112407429,
0.778674300258396));
#13068=CARTESIAN_POINT('Ctrl Pts',(0.153133495662976,-0.0273264462662894,
0.778766236433758));
#13069=CARTESIAN_POINT('Ctrl Pts',(0.153288065097442,-0.0264456298460426,
0.77882817589768));
#13070=CARTESIAN_POINT('Ctrl Pts',(0.153654327342955,-0.0242472828642634,
0.778981781069904));
#13071=CARTESIAN_POINT('Ctrl Pts',(0.153856682283298,-0.0229282485285171,
0.779073068593096));
#13072=CARTESIAN_POINT('Ctrl Pts',(0.154748899773841,-0.0165673141999273,
0.77950978665694));
#13073=CARTESIAN_POINT('Ctrl Pts',(0.155208085289536,-0.0114958824002954,
0.779847459529292));
#13074=CARTESIAN_POINT('Ctrl Pts',(0.155750349392639,0.00165039431151851,
0.780715614663966));
#13075=CARTESIAN_POINT('Ctrl Pts',(0.155455190247727,0.00972487931033154,
0.781242438282852));
#13076=CARTESIAN_POINT('Ctrl Pts',(0.153830882395702,0.0238744926984932,
0.782197292971392));
#13077=CARTESIAN_POINT('Ctrl Pts',(0.152762090744374,0.0299609729633764,
0.782618468815589));
#13078=CARTESIAN_POINT('Ctrl Pts',(0.151096219339256,0.0369702268929665,
0.783123778231147));
#13079=CARTESIAN_POINT('Ctrl Pts',(0.150847898004737,0.0379707354645114,
0.783196388881908));
#13080=CARTESIAN_POINT('Ctrl Pts',(0.150451030483555,0.0395043809974338,
0.783308466792793));
#13081=CARTESIAN_POINT('Ctrl Pts',(0.150309549378168,0.0400393311996677,
0.783347706370615));
#13082=CARTESIAN_POINT('Ctrl Pts',(0.150046471007586,0.0410130015107262,
0.783419398180742));
#13083=CARTESIAN_POINT('Ctrl Pts',(0.149925795750907,0.0414519663601781,
0.783451820268677));
#13084=CARTESIAN_POINT('Ctrl Pts',(0.149658305003929,0.0424085334404736,
0.783522696273284));
#13085=CARTESIAN_POINT('Ctrl Pts',(0.149510728046123,0.0429259146775495,
0.783561174536549));
#13086=CARTESIAN_POINT('Ctrl Pts',(0.149099628430607,0.0443393234998059,
0.783666690344779));
#13087=CARTESIAN_POINT('Ctrl Pts',(0.148830718840912,0.0452337469723748,
0.783733902286087));
#13088=CARTESIAN_POINT('Ctrl Pts',(0.147432924375321,0.0497355269152193,
0.78407446898486));
#13089=CARTESIAN_POINT('Ctrl Pts',(0.14618096609324,0.0533030053836293,
0.784351813502948));
#13090=CARTESIAN_POINT('Ctrl Pts',(0.144409475143314,0.0578173977539785,
0.78471284232296));
#13091=CARTESIAN_POINT('Ctrl Pts',(0.144008247882034,0.0588096288020261,
0.784792828435677));
#13092=CARTESIAN_POINT('Ctrl Pts',(0.13908194124866,0.0706395641171971,
0.785754076635668));
#13093=CARTESIAN_POINT('Ctrl Pts',(0.133354060236117,0.0809342850009497,
0.786671678836341));
#13094=CARTESIAN_POINT('Ctrl Pts',(0.123916329447004,0.09413097579025,0.787923552299801));
#13095=CARTESIAN_POINT('Ctrl Pts',(0.121152069317364,0.0976630940760973,
0.788266680825109));
#13096=CARTESIAN_POINT('Ctrl Pts',(0.116793819120748,0.102761628635682,
0.788769278904082));
#13097=CARTESIAN_POINT('Ctrl Pts',(0.115312571246287,0.104421074562778,
0.788934093877867));
#13098=CARTESIAN_POINT('Ctrl Pts',(0.113445312365403,0.106424754669651,
0.789134051440653));
#13099=CARTESIAN_POINT('Ctrl Pts',(0.113092610202952,0.106799479595455,
0.789171489307682));
#13100=CARTESIAN_POINT('Ctrl Pts',(0.112534689739361,0.107386373536638,
0.789230181373474));
#13101=CARTESIAN_POINT('Ctrl Pts',(0.112330720464652,0.107599715891554,
0.789251528530322));
#13102=CARTESIAN_POINT('Ctrl Pts',(0.111947017038074,0.107998771601096,
0.789291478543127));
#13103=CARTESIAN_POINT('Ctrl Pts',(0.111767429463248,0.108184615374602,
0.789310091647807));
#13104=CARTESIAN_POINT('Ctrl Pts',(0.111354843299807,0.108609450666968,
0.789352660645121));
#13105=CARTESIAN_POINT('Ctrl Pts',(0.111121538323439,0.108848140208246,
0.789376592299338));
#13106=CARTESIAN_POINT('Ctrl Pts',(0.110507870358779,0.109471941927973,
0.789439181082622));
#13107=CARTESIAN_POINT('Ctrl Pts',(0.11012625787481,0.109855827474938,0.789477743044949));
#13108=CARTESIAN_POINT('Ctrl Pts',(0.107546896565529,0.112423604842781,
0.789736052218443));
#13109=CARTESIAN_POINT('Ctrl Pts',(0.105286131660525,0.114543597972723,
0.78995113818279));
#13110=CARTESIAN_POINT('Ctrl Pts',(0.10227824088442,0.117199826536193,0.790225472673442));
#13111=CARTESIAN_POINT('Ctrl Pts',(0.101587804607612,0.117798794222096,
0.79028766996987));
#13112=CARTESIAN_POINT('Ctrl Pts',(0.0915458374841799,0.126356452460334,
0.791181881236259));
#13113=CARTESIAN_POINT('Ctrl Pts',(0.0812888453034642,0.133186943557129,
0.791969342723043));
#13114=CARTESIAN_POINT('Ctrl Pts',(0.0663738002059899,0.140748145014673,
0.793087125375898));
#13115=CARTESIAN_POINT('Ctrl Pts',(0.0623291906936536,0.142585372432512,
0.793387385172353));
#13116=CARTESIAN_POINT('Ctrl Pts',(0.0557217693590248,0.14525183942048,
0.793878029224762));
#13117=CARTESIAN_POINT('Ctrl Pts',(0.0532062908837309,0.146192002284986,
0.794064829713856));
#13118=CARTESIAN_POINT('Ctrl Pts',(0.0499073590577501,0.147328561509932,
0.794310411203595));
#13119=CARTESIAN_POINT('Ctrl Pts',(0.0491448422838382,0.147584667082986,
0.794367215226336));
#13120=CARTESIAN_POINT('Ctrl Pts',(0.047901577854178,0.147991537425799,
0.794459913687363));
#13121=CARTESIAN_POINT('Ctrl Pts',(0.0474220163572628,0.14814590329908,
0.794495689498111));
#13122=CARTESIAN_POINT('Ctrl Pts',(0.0464984133227592,0.148438257428172,
0.794564632754068));
#13123=CARTESIAN_POINT('Ctrl Pts',(0.0460544856375709,0.148576589858141,
0.794597788510254));
#13124=CARTESIAN_POINT('Ctrl Pts',(0.0450367710393607,0.148888720828842,
0.794673844323989));
#13125=CARTESIAN_POINT('Ctrl Pts',(0.044462589310013,0.149061195718147,
0.79471678703855));
#13126=CARTESIAN_POINT('Ctrl Pts',(0.0429349999975343,0.149510447326604,
0.794831129950518));
#13127=CARTESIAN_POINT('Ctrl Pts',(0.0419799291292653,0.149781419241201,
0.794902717268526));
#13128=CARTESIAN_POINT('Ctrl Pts',(0.0348225602128495,0.151738269304934,
0.795440016857477));
#13129=CARTESIAN_POINT('Ctrl Pts',(0.0285245959452449,0.153047178533373,
0.795917780370095));
#13130=CARTESIAN_POINT('Ctrl Pts',(0.0080011785399801,0.15600173438768,
0.797491389239621));
#13131=CARTESIAN_POINT('Ctrl Pts',(-0.00637404542214832,0.156076522523706,
0.798625780759763));
#13132=CARTESIAN_POINT('Ctrl Pts',(-0.022833188343903,0.153882179321186,
0.7998710130445));
#13133=CARTESIAN_POINT('Ctrl Pts',(-0.0251033999956616,0.153528174743988,
0.800041356368757));
#13134=CARTESIAN_POINT('Ctrl Pts',(-0.0278768176971603,0.153032531702818,
0.800247071002812));
#13135=CARTESIAN_POINT('Ctrl Pts',(-0.028388089491437,0.152938514181768,
0.800284893780436));
#13136=CARTESIAN_POINT('Ctrl Pts',(-0.0291900412426293,0.152786883572281,
0.800344053064149));
#13137=CARTESIAN_POINT('Ctrl Pts',(-0.0294810378070146,0.152731001153364,
0.800365484960294));
#13138=CARTESIAN_POINT('Ctrl Pts',(-0.0300253575047191,0.1526248574209,
0.800405506959248));
#13139=CARTESIAN_POINT('Ctrl Pts',(-0.0302787122072849,0.152574797344376,
0.8004241077357));
#13140=CARTESIAN_POINT('Ctrl Pts',(-0.0308574497311752,0.152458946912431,
0.800466535736156));
#13141=CARTESIAN_POINT('Ctrl Pts',(-0.031182747021868,0.152392745861793,
0.800490339316069));
#13142=CARTESIAN_POINT('Ctrl Pts',(-0.032184173411267,0.152185605390961,
0.800563488802791));
#13143=CARTESIAN_POINT('Ctrl Pts',(-0.0328595903921099,0.152041201235197,
0.800612642422108));
#13144=CARTESIAN_POINT('Ctrl Pts',(-0.042148116187281,0.149990525887887,
0.80128638672946));
#13145=CARTESIAN_POINT('Ctrl Pts',(-0.0505863797026703,0.147359064157851,
0.80187243974495));
#13146=CARTESIAN_POINT('Ctrl Pts',(-0.0604135697152416,0.14334993345218,
0.802572387203032));
#13147=CARTESIAN_POINT('Ctrl Pts',(-0.0620576279375163,0.142645887665595,
0.80269007939709));
#13148=CARTESIAN_POINT('Ctrl Pts',(-0.0636886325197553,0.141913919640617,
0.802807733721352));
#13149=CARTESIAN_POINT('Origin',(0.,0.,-0.129405622560373));
#13150=CARTESIAN_POINT('',(-0.0636885883104208,0.141913939481031,0.886533246392299));
#13151=CARTESIAN_POINT('',(-0.0636886258347646,0.141913922640731,0.87264646002013));
#13152=CARTESIAN_POINT('',(-0.0636886258329924,0.141913922641526,-0.129405622560373));
#13153=CARTESIAN_POINT('',(-0.155549948690716,-0.000126342057708579,0.829469708790686));
#13154=CARTESIAN_POINT('Ctrl Pts',(-0.0636885883104107,0.141913939481036,
0.886533246392299));
#13155=CARTESIAN_POINT('Ctrl Pts',(-0.0557309582408581,0.145485189967631,
0.885954834675078));
#13156=CARTESIAN_POINT('Ctrl Pts',(-0.0474779691464282,0.148384890244849,
0.885387010768159));
#13157=CARTESIAN_POINT('Ctrl Pts',(-0.0324099555367,0.152289041749862,0.88434789329685));
#13158=CARTESIAN_POINT('Ctrl Pts',(-0.0257003671515546,0.153563761069064,
0.883884516764253));
#13159=CARTESIAN_POINT('Ctrl Pts',(-0.0179340183461664,0.154515951193323,
0.883336355006266));
#13160=CARTESIAN_POINT('Ctrl Pts',(-0.0169374964047631,0.154628358716609,
0.883265808559678));
#13161=CARTESIAN_POINT('Ctrl Pts',(-0.0153405636421684,0.154792870369464,
0.883152389149448));
#13162=CARTESIAN_POINT('Ctrl Pts',(-0.014740803744391,0.154851135922697,
0.883109709302275));
#13163=CARTESIAN_POINT('Ctrl Pts',(-0.0136770867155704,0.154948238304049,
0.883033859799711));
#13164=CARTESIAN_POINT('Ctrl Pts',(-0.0132132624224909,0.154988480030233,
0.883000734561069));
#13165=CARTESIAN_POINT('Ctrl Pts',(-0.0122483026607682,0.155067837563457,
0.882931708464853));
#13166=CARTESIAN_POINT('Ctrl Pts',(-0.0117471450188714,0.155106607653069,
0.882895797181827));
#13167=CARTESIAN_POINT('Ctrl Pts',(-0.0104491585834692,0.155200694518073,
0.882802622072632));
#13168=CARTESIAN_POINT('Ctrl Pts',(-0.00965208463037596,0.155252303403557,
0.882745242992048));
#13169=CARTESIAN_POINT('Ctrl Pts',(-0.00622756059518912,0.155447560575373,
0.882497999231447));
#13170=CARTESIAN_POINT('Ctrl Pts',(-0.00359724039065065,0.155530655786621,
0.88230626098265));
#13171=CARTESIAN_POINT('Ctrl Pts',(0.00335036183627117,0.155573812660352,
0.881794589444205));
#13172=CARTESIAN_POINT('Ctrl Pts',(0.00766579282231143,0.15542092993162,
0.881471395099634));
#13173=CARTESIAN_POINT('Ctrl Pts',(0.0243262636164154,0.154135162763463,
0.880203431210545));
#13174=CARTESIAN_POINT('Ctrl Pts',(0.0365238279629842,0.151708208869297,
0.879227542470186));
#13175=CARTESIAN_POINT('Ctrl Pts',(0.0491519596285416,0.147582804468907,
0.878215292317797));
#13176=CARTESIAN_POINT('Ctrl Pts',(0.0499980865010896,0.147298305208132,
0.878147483289698));
#13177=CARTESIAN_POINT('Ctrl Pts',(0.0538547442220192,0.145964492626417,
0.877838606861723));
#13178=CARTESIAN_POINT('Ctrl Pts',(0.056835295690395,0.144829967604943,
0.877600439671863));
#13179=CARTESIAN_POINT('Ctrl Pts',(0.0602831581317987,0.14339470498393,
0.877327199666263));
#13180=CARTESIAN_POINT('Ctrl Pts',(0.0607860925730163,0.143182231946716,
0.877287400392466));
#13181=CARTESIAN_POINT('Ctrl Pts',(0.0615927333595057,0.142836436848808,
0.877223672571824));
#13182=CARTESIAN_POINT('Ctrl Pts',(0.0618971440517604,0.142704786388414,
0.877199647075541));
#13183=CARTESIAN_POINT('Ctrl Pts',(0.0624384277052468,0.142468636095738,
0.877156972506382));
#13184=CARTESIAN_POINT('Ctrl Pts',(0.0626754630306191,0.142364517571019,
0.877138300646802));
#13185=CARTESIAN_POINT('Ctrl Pts',(0.0631803986298991,0.142141217454963,
0.877098560322931));
#13186=CARTESIAN_POINT('Ctrl Pts',(0.0634482216213194,0.142021870314343,
0.877077502187409));
#13187=CARTESIAN_POINT('Ctrl Pts',(0.0641768760939549,0.141694695131272,
0.877020261922814));
#13188=CARTESIAN_POINT('Ctrl Pts',(0.0646370400312778,0.141485374256706,
0.876984169713385));
#13189=CARTESIAN_POINT('Ctrl Pts',(0.0670051412948642,0.140394199923349,
0.876798681558541));
#13190=CARTESIAN_POINT('Ctrl Pts',(0.0688962019565898,0.1394759293378,0.876651398413019));
#13191=CARTESIAN_POINT('Ctrl Pts',(0.0744298143608292,0.136648864523816,
0.876221200489449));
#13192=CARTESIAN_POINT('Ctrl Pts',(0.0780161417610215,0.134633564841213,
0.87594339282131));
#13193=CARTESIAN_POINT('Ctrl Pts',(0.0904043013319887,0.127010686872075,
0.874972431110522));
#13194=CARTESIAN_POINT('Ctrl Pts',(0.0987173285323472,0.120662965108255,
0.87429801680404));
#13195=CARTESIAN_POINT('Ctrl Pts',(0.10850943998619,0.111491706516617,0.873400276261083));
#13196=CARTESIAN_POINT('Ctrl Pts',(0.110627235799444,0.109390641089544,
0.873199097977098));
#13197=CARTESIAN_POINT('Ctrl Pts',(0.115230988208832,0.104552766152732,
0.872743580914815));
#13198=CARTESIAN_POINT('Ctrl Pts',(0.117682317588431,0.101785705819696,
0.87248817161644));
#13199=CARTESIAN_POINT('Ctrl Pts',(0.120622271904033,0.0982187836493397,
0.872163528261071));
#13200=CARTESIAN_POINT('Ctrl Pts',(0.121205489450828,0.0974981599900408,
0.872098167603466));
#13201=CARTESIAN_POINT('Ctrl Pts',(0.122116015281513,0.0963523179964739,
0.871994571084442));
#13202=CARTESIAN_POINT('Ctrl Pts',(0.122447631540451,0.0959305367885992,
0.871956507371756));
#13203=CARTESIAN_POINT('Ctrl Pts',(0.123056712850689,0.0951475452999969,
0.871885969955472));
#13204=CARTESIAN_POINT('Ctrl Pts',(0.123334787277894,0.0947868144482662,
0.871853520822379));
#13205=CARTESIAN_POINT('Ctrl Pts',(0.123948433597489,0.0939834921825097,
0.871781361880888));
#13206=CARTESIAN_POINT('Ctrl Pts',(0.124283225954363,0.0935403160443579,
0.871741622071087));
#13207=CARTESIAN_POINT('Ctrl Pts',(0.125238155691429,0.0922620657407525,
0.871627190502249));
#13208=CARTESIAN_POINT('Ctrl Pts',(0.12585228937465,0.0914225660173952,
0.87155226728676));
#13209=CARTESIAN_POINT('Ctrl Pts',(0.130196115274874,0.0853579871591274,
0.871012562893483));
#13210=CARTESIAN_POINT('Ctrl Pts',(0.133607064566514,0.0799133597275997,
0.870535776563866));
#13211=CARTESIAN_POINT('Ctrl Pts',(0.142409037449887,0.063716915419631,
0.869137732793021));
#13212=CARTESIAN_POINT('Ctrl Pts',(0.146903239258912,0.0525316376017849,
0.868193035165235));
#13213=CARTESIAN_POINT('Ctrl Pts',(0.151238106539499,0.0366427548870334,
0.866934350184584));
#13214=CARTESIAN_POINT('Ctrl Pts',(0.152225777953326,0.0322951710133692,
0.866598541750189));
#13215=CARTESIAN_POINT('Ctrl Pts',(0.153144115564801,0.0272602196725307,
0.866223647285724));
#13216=CARTESIAN_POINT('Ctrl Pts',(0.15325861341003,0.0266089677823639,
0.866175423371968));
#13217=CARTESIAN_POINT('Ctrl Pts',(0.153423390178777,0.0256353710281211,
0.866103748638998));
#13218=CARTESIAN_POINT('Ctrl Pts',(0.153476811598263,0.0253135775551344,
0.866080126758472));
#13219=CARTESIAN_POINT('Ctrl Pts',(0.153570644680489,0.024737139403579,
0.866037936839227));
#13220=CARTESIAN_POINT('Ctrl Pts',(0.153611435677005,0.0244825612680901,
0.86601934772864));
#13221=CARTESIAN_POINT('Ctrl Pts',(0.153698394706228,0.023931072844203,
0.865979173254531));
#13222=CARTESIAN_POINT('Ctrl Pts',(0.153744335359232,0.0236341306558906,
0.86595760087406));
#13223=CARTESIAN_POINT('Ctrl Pts',(0.153870212378724,0.0228046106373711,
0.865897497671507));
#13224=CARTESIAN_POINT('Ctrl Pts',(0.153948244878478,0.0222717409634943,
0.865859072501626));
#13225=CARTESIAN_POINT('Ctrl Pts',(0.154384098287754,0.019183589710003,
0.865637394767268));
#13226=CARTESIAN_POINT('Ctrl Pts',(0.1546810907192,0.0166199335255763,0.865457360307288));
#13227=CARTESIAN_POINT('Ctrl Pts',(0.156244297755291,-0.000616012416733156,
0.864266429844491));
#13228=CARTESIAN_POINT('Ctrl Pts',(0.155485289398982,-0.0153978724115204,
0.863332979896753));
#13229=CARTESIAN_POINT('Ctrl Pts',(0.152295039607863,-0.0317112821963661,
0.862216217731747));
#13230=CARTESIAN_POINT('Ctrl Pts',(0.151897940870372,-0.0335618781605787,
0.862088358726973));
#13231=CARTESIAN_POINT('Ctrl Pts',(0.150549521551592,-0.0393306370886721,
0.861685386311132));
#13232=CARTESIAN_POINT('Ctrl Pts',(0.149479646316607,-0.0432190695091235,
0.861407303034985));
#13233=CARTESIAN_POINT('Ctrl Pts',(0.147997002703635,-0.0478899312834811,
0.861063265241731));
#13234=CARTESIAN_POINT('Ctrl Pts',(0.147727035230681,-0.0487163354011653,
0.861002010965989));
#13235=CARTESIAN_POINT('Ctrl Pts',(0.147269059704246,-0.0500794358067639,
0.860900317281739));
#13236=CARTESIAN_POINT('Ctrl Pts',(0.147085008124732,-0.0506174496222945,
0.860860008109573));
#13237=CARTESIAN_POINT('Ctrl Pts',(0.14674657211634,-0.0515893218831334,
0.860786877830356));
#13238=CARTESIAN_POINT('Ctrl Pts',(0.146593202367092,-0.0520235290196553,
0.860754090590148));
#13239=CARTESIAN_POINT('Ctrl Pts',(0.146259968857814,-0.0529537762068859,
0.860683597581025));
#13240=CARTESIAN_POINT('Ctrl Pts',(0.146079505183643,-0.0534495936139159,
0.860645872240338));
#13241=CARTESIAN_POINT('Ctrl Pts',(0.145580370926055,-0.0547995363058094,
0.860542735305214));
#13242=CARTESIAN_POINT('Ctrl Pts',(0.145256713087452,-0.0556517817827719,
0.860477158328525));
#13243=CARTESIAN_POINT('Ctrl Pts',(0.143505258188574,-0.0601442705812009,
0.860128963553767));
#13244=CARTESIAN_POINT('Ctrl Pts',(0.141948190634919,-0.0637322406613657,
0.859842042628733));
#13245=CARTESIAN_POINT('Ctrl Pts',(0.133860409900367,-0.0805983812626829,
0.858448817575511));
#13246=CARTESIAN_POINT('Ctrl Pts',(0.125592608505698,-0.0929572975477284,
0.857282509017944));
#13247=CARTESIAN_POINT('Ctrl Pts',(0.112751227511238,-0.107249849862203,
0.855814390644805));
#13248=CARTESIAN_POINT('Ctrl Pts',(0.109655499419823,-0.110413088288794,
0.855481087202818));
#13249=CARTESIAN_POINT('Ctrl Pts',(0.10594733564764,-0.113892055838166,
0.855108644749989));
#13250=CARTESIAN_POINT('Ctrl Pts',(0.105463006786398,-0.114340686351543,
0.855060498596647));
#13251=CARTESIAN_POINT('Ctrl Pts',(0.104735271038529,-0.115006224893193,
0.854988916488554));
#13252=CARTESIAN_POINT('Ctrl Pts',(0.10449402326186,-0.115225465377872,
0.854965310110057));
#13253=CARTESIAN_POINT('Ctrl Pts',(0.104060748222832,-0.1156167360056,0.854923136879356));
#13254=CARTESIAN_POINT('Ctrl Pts',(0.103868981746331,-0.115789047840443,
0.854904549026821));
#13255=CARTESIAN_POINT('Ctrl Pts',(0.103452669206257,-0.116161259076944,
0.85486436474035));
#13256=CARTESIAN_POINT('Ctrl Pts',(0.10322797238731,-0.116360983999005,
0.8548427813449));
#13257=CARTESIAN_POINT('Ctrl Pts',(0.102598611931363,-0.116917142121499,
0.854782616421558));
#13258=CARTESIAN_POINT('Ctrl Pts',(0.102192666368243,-0.117272129065913,
0.854744140897477));
#13259=CARTESIAN_POINT('Ctrl Pts',(0.0998249606595039,-0.119320984493836,
0.854521589233907));
#13260=CARTESIAN_POINT('Ctrl Pts',(0.0978228074341549,-0.120967849372446,
0.854340760945773));
#13261=CARTESIAN_POINT('Ctrl Pts',(0.0841843914425153,-0.131625880267573,
0.853149841597209));
#13262=CARTESIAN_POINT('Ctrl Pts',(0.071360144898193,-0.138997204756141,
0.852216938722345));
#13263=CARTESIAN_POINT('Ctrl Pts',(0.0559194062181418,-0.145163547839768,
0.851099879710145));
#13264=CARTESIAN_POINT('Ctrl Pts',(0.0541364776695639,-0.14583784484268,
0.850971103800745));
#13265=CARTESIAN_POINT('Ctrl Pts',(0.0485591677040739,-0.147830794478288,
0.850568189566551));
#13266=CARTESIAN_POINT('Ctrl Pts',(0.0447260570270535,-0.149035269705835,
0.850291118561336));
#13267=CARTESIAN_POINT('Ctrl Pts',(0.0400130168388674,-0.150318046280951,
0.849948200853536));
#13268=CARTESIAN_POINT('Ctrl Pts',(0.0391732550245654,-0.150539073301947,
0.849887017700901));
#13269=CARTESIAN_POINT('Ctrl Pts',(0.0377809163812575,-0.150893100686792,
0.849785417690192));
#13270=CARTESIAN_POINT('Ctrl Pts',(0.0372293745907179,-0.151030126562594,
0.849745130644801));
#13271=CARTESIAN_POINT('Ctrl Pts',(0.0362296067076135,-0.151272701230479,
0.849672023996671));
#13272=CARTESIAN_POINT('Ctrl Pts',(0.0357816370948312,-0.151379288471737,
0.849639238158773));
#13273=CARTESIAN_POINT('Ctrl Pts',(0.0353320238176394,-0.15148415954951,
0.849606301747618));
#13274=CARTESIAN_POINT('Ctrl Pts',(0.0353308424402875,-0.151484435087998,
0.849606215205634));
#13275=CARTESIAN_POINT('Ctrl Pts',(0.035328486592679,-0.151484984524953,
0.849606042627233));
#13276=CARTESIAN_POINT('Ctrl Pts',(0.0353273118913456,-0.15148525847747,
0.849605956573888));
#13277=CARTESIAN_POINT('Ctrl Pts',(0.0353249690444817,-0.15148580482489,
0.849605784947035));
#13278=CARTESIAN_POINT('Ctrl Pts',(0.0353238008911775,-0.151486077221765,
0.849605699372959));
#13279=CARTESIAN_POINT('Ctrl Pts',(0.0353214710870273,-0.151486620470821,
0.849605528700742));
#13280=CARTESIAN_POINT('Ctrl Pts',(0.0353203094287292,-0.151486891324896,
0.849605443602057));
#13281=CARTESIAN_POINT('Ctrl Pts',(0.0353179925598226,-0.151487431501596,
0.849605273876617));
#13282=CARTESIAN_POINT('Ctrl Pts',(0.0353168373425601,-0.151487700825927,
0.849605189249377));
#13283=CARTESIAN_POINT('Ctrl Pts',(0.0353145333101644,-0.151488237954226,
0.849605020463495));
#13284=CARTESIAN_POINT('Ctrl Pts',(0.0353133844851565,-0.15148850576065,
0.849604936304132));
#13285=CARTESIAN_POINT('Ctrl Pts',(0.0353110931748767,-0.151489039868139,
0.84960476844944));
#13286=CARTESIAN_POINT('Ctrl Pts',(0.0353099506864661,-0.151489306170089,
0.849604684753884));
#13287=CARTESIAN_POINT('Ctrl Pts',(0.0353076720066047,-0.151489837279055,
0.849604517823679));
#13288=CARTESIAN_POINT('Ctrl Pts',(0.0353065358064704,-0.151490102088245,
0.849604434588396));
#13289=CARTESIAN_POINT('Ctrl Pts',(0.0353042696469616,-0.151490630225239,
0.849604268574626));
#13290=CARTESIAN_POINT('Ctrl Pts',(0.0353031396815149,-0.151490893554606,
0.849604185795697));
#13291=CARTESIAN_POINT('Ctrl Pts',(0.0347944456962448,-0.151609434599421,
0.849566919841226));
#13292=CARTESIAN_POINT('Ctrl Pts',(0.034286296228128,-0.151725159382405,
0.84952965508757));
#13293=CARTESIAN_POINT('Ctrl Pts',(0.0329098126447955,-0.15203136853186,
0.849428601607333));
#13294=CARTESIAN_POINT('Ctrl Pts',(0.032040423038703,-0.152216963629336,
0.849364657668824));
#13295=CARTESIAN_POINT('Ctrl Pts',(0.0301068652700983,-0.152612435957079,
0.849222161993263));
#13296=CARTESIAN_POINT('Ctrl Pts',(0.029042005195906,-0.152818653208929,
0.849143497237425));
#13297=CARTESIAN_POINT('Ctrl Pts',(0.0257974275122641,-0.153411850931766,
0.848903199282392));
#13298=CARTESIAN_POINT('Ctrl Pts',(0.0236116116832879,-0.153763435657424,
0.848740476003865));
#13299=CARTESIAN_POINT('Ctrl Pts',(0.00649163142723672,-0.156143518667789,
0.847459033540093));
#13300=CARTESIAN_POINT('Ctrl Pts',(-0.00865689128124857,-0.156037903576278,
0.846272748448176));
#13301=CARTESIAN_POINT('Ctrl Pts',(-0.0245910061659342,-0.153597515877808,
0.845038443564618));
#13302=CARTESIAN_POINT('Ctrl Pts',(-0.0256317216626494,-0.153427277235785,
0.844957943113218));
#13303=CARTESIAN_POINT('Ctrl Pts',(-0.030379704097775,-0.152600949820218,
0.844591420359134));
#13304=CARTESIAN_POINT('Ctrl Pts',(-0.0340645062244877,-0.151820919592666,
0.844309010648112));
#13305=CARTESIAN_POINT('Ctrl Pts',(-0.0383259850394866,-0.150755810720089,
0.843987435419375));
#13306=CARTESIAN_POINT('Ctrl Pts',(-0.0389333361683257,-0.150600102808235,
0.843941725396808));
#13307=CARTESIAN_POINT('Ctrl Pts',(-0.0398525381522708,-0.150358512569947,
0.843872746074385));
#13308=CARTESIAN_POINT('Ctrl Pts',(-0.0401650800514967,-0.15027532548313,
0.843849327449929));
#13309=CARTESIAN_POINT('Ctrl Pts',(-0.0407261209372963,-0.15012412180567,
0.843807355222793));
#13310=CARTESIAN_POINT('Ctrl Pts',(-0.0409747110358075,-0.150056462484769,
0.843788781487636));
#13311=CARTESIAN_POINT('Ctrl Pts',(-0.0415148857965436,-0.149907999465116,
0.843748473247666));
#13312=CARTESIAN_POINT('Ctrl Pts',(-0.0418064023507024,-0.149826962770641,
0.84372675246862));
#13313=CARTESIAN_POINT('Ctrl Pts',(-0.0426253928067726,-0.149596720798495,
0.84366581610499));
#13314=CARTESIAN_POINT('Ctrl Pts',(-0.0431523243307589,-0.149445575092002,
0.843626710963861));
#13315=CARTESIAN_POINT('Ctrl Pts',(-0.0462751467000908,-0.148531926765663,
0.843395494773945));
#13316=CARTESIAN_POINT('Ctrl Pts',(-0.048851788521746,-0.147704528110391,
0.843206926862309));
#13317=CARTESIAN_POINT('Ctrl Pts',(-0.0572192549931257,-0.144774652656276,
0.842597793534907));
#13318=CARTESIAN_POINT('Ctrl Pts',(-0.0629073052769641,-0.142395324942774,
0.842188738504685));
#13319=CARTESIAN_POINT('Ctrl Pts',(-0.0777792221583317,-0.135108701157259,
0.841096069980007));
#13320=CARTESIAN_POINT('Ctrl Pts',(-0.0866355455706651,-0.129607995757295,
0.840418448221008));
#13321=CARTESIAN_POINT('Ctrl Pts',(-0.098004429180422,-0.120857413649837,
0.839441918038446));
#13322=CARTESIAN_POINT('Ctrl Pts',(-0.10103931436128,-0.118331884902855,
0.839169537002037));
#13323=CARTESIAN_POINT('Ctrl Pts',(-0.104616937976521,-0.115116655839939,
0.838831814887102));
#13324=CARTESIAN_POINT('Ctrl Pts',(-0.105254369837748,-0.114534124783255,
0.838770969424666));
#13325=CARTESIAN_POINT('Ctrl Pts',(-0.106302116421647,-0.113560485278865,
0.838669814239373));
#13326=CARTESIAN_POINT('Ctrl Pts',(-0.106715208618646,-0.1131723818188,
0.838629632325799));
#13327=CARTESIAN_POINT('Ctrl Pts',(-0.107459962228186,-0.112464976608252,
0.838556637702664));
#13328=CARTESIAN_POINT('Ctrl Pts',(-0.10779234641724,-0.112146442168666,
0.838523858273135));
#13329=CARTESIAN_POINT('Ctrl Pts',(-0.108435155383258,-0.111524919816016,
0.838460068305689));
#13330=CARTESIAN_POINT('Ctrl Pts',(-0.108745736797507,-0.111222099352119,
0.838429065236399));
#13331=CARTESIAN_POINT('Ctrl Pts',(-0.109603790271067,-0.110378457461784,
0.838342901456648));
#13332=CARTESIAN_POINT('Ctrl Pts',(-0.110148515197611,-0.109834872757619,
0.838287619677268));
#13333=CARTESIAN_POINT('Ctrl Pts',(-0.112453922919354,-0.107499892096503,
0.83805113004833));
#13334=CARTESIAN_POINT('Ctrl Pts',(-0.114175016550804,-0.105670127320208,
0.837868217802818));
#13335=CARTESIAN_POINT('Ctrl Pts',(-0.118565873240046,-0.100769481917354,
0.83738414451957));
#13336=CARTESIAN_POINT('Ctrl Pts',(-0.121160616010215,-0.0976342900634126,
0.837080119314934));
#13337=CARTESIAN_POINT('Ctrl Pts',(-0.12655911307234,-0.0905643367086734,
0.83640666176002));
#13338=CARTESIAN_POINT('Ctrl Pts',(-0.129308509468712,-0.086593369292964,
0.836035943440676));
#13339=CARTESIAN_POINT('Ctrl Pts',(-0.137825176806334,-0.072980468047344,
0.834794437583796));
#13340=CARTESIAN_POINT('Ctrl Pts',(-0.142733522471522,-0.0628419460443651,
0.833913836437172));
#13341=CARTESIAN_POINT('Ctrl Pts',(-0.146890228136033,-0.0511894658104013,
0.83299954343689));
#13342=CARTESIAN_POINT('Ctrl Pts',(-0.147261234641557,-0.0501121692644601,
0.832915918039014));
#13343=CARTESIAN_POINT('Ctrl Pts',(-0.147752606139395,-0.0486327650302099,
0.832802400043315));
#13344=CARTESIAN_POINT('Ctrl Pts',(-0.14788321852574,-0.0482341387922267,
0.83277194296649));
#13345=CARTESIAN_POINT('Ctrl Pts',(-0.148088117217248,-0.0476001360567745,
0.832723714123265));
#13346=CARTESIAN_POINT('Ctrl Pts',(-0.148163457305142,-0.0473651067273554,
0.832705881533063));
#13347=CARTESIAN_POINT('Ctrl Pts',(-0.148317799287829,-0.0468796530098195,
0.832669144943366));
#13348=CARTESIAN_POINT('Ctrl Pts',(-0.148396726501924,-0.0466292077633217,
0.832650245770599));
#13349=CARTESIAN_POINT('Ctrl Pts',(-0.148583054959099,-0.0460327010982864,
0.83260535619198));
#13350=CARTESIAN_POINT('Ctrl Pts',(-0.14868988284744,-0.0456864590156303,
0.832579399237554));
#13351=CARTESIAN_POINT('Ctrl Pts',(-0.149045020267678,-0.0445209752363483,
0.832492348755955));
#13352=CARTESIAN_POINT('Ctrl Pts',(-0.14928778277448,-0.0437000378200648,
0.832431568301207));
#13353=CARTESIAN_POINT('Ctrl Pts',(-0.149853825699472,-0.0417260973803592,
0.832286609177381));
#13354=CARTESIAN_POINT('Ctrl Pts',(-0.150170599403682,-0.0405712653102088,
0.83220276833904));
#13355=CARTESIAN_POINT('Ctrl Pts',(-0.153833038689739,-0.0265884656197295,
0.831197937906557));
#13356=CARTESIAN_POINT('Ctrl Pts',(-0.155539178755421,-0.013386082424089,
0.830349973974934));
#13357=CARTESIAN_POINT('Ctrl Pts',(-0.155549948690716,-0.000126342057708579,
0.829469708790686));
#13358=CARTESIAN_POINT('Ctrl Pts',(-0.155549948817025,-0.00012618645330382,
0.829469698460683));
#13359=CARTESIAN_POINT('Ctrl Pts',(-0.155554514228924,0.00550159346059295,
0.829096090860219));
#13360=CARTESIAN_POINT('Ctrl Pts',(-0.155253663330696,0.0111251091990293,
0.828718226575423));
#13361=CARTESIAN_POINT('Ctrl Pts',(-0.154386614564261,0.0191448636797682,
0.828163896303848));
#13362=CARTESIAN_POINT('Ctrl Pts',(-0.154067426800833,0.021563382051133,
0.827994722731987));
#13363=CARTESIAN_POINT('Ctrl Pts',(-0.153572980556294,0.0247332517364343,
0.827769883097865));
#13364=CARTESIAN_POINT('Ctrl Pts',(-0.153448805689968,0.0254923143944479,
0.827715807379159));
#13365=CARTESIAN_POINT('Ctrl Pts',(-0.153230687766271,0.0267662609700567,
0.827624640217435));
#13366=CARTESIAN_POINT('Ctrl Pts',(-0.153139765358742,0.0272816541554971,
0.827587643867501));
#13367=CARTESIAN_POINT('Ctrl Pts',(-0.152968574006925,0.0282242233515341,
0.827519771134307));
#13368=CARTESIAN_POINT('Ctrl Pts',(-0.152889111905139,0.0286515422165518,
0.827488920516889));
#13369=CARTESIAN_POINT('Ctrl Pts',(-0.152730514015063,0.0294849754697185,
0.827428590891142));
#13370=CARTESIAN_POINT('Ctrl Pts',(-0.152651546715168,0.0298911185664314,
0.827399117465349));
#13371=CARTESIAN_POINT('Ctrl Pts',(-0.152465607102645,0.0308274833278512,
0.827330992915194));
#13372=CARTESIAN_POINT('Ctrl Pts',(-0.152357488162434,0.031357469041479,
0.827292305603255));
#13373=CARTESIAN_POINT('Ctrl Pts',(-0.152052661911768,0.0328128880619441,
0.827185704437716));
#13374=CARTESIAN_POINT('Ctrl Pts',(-0.151850275055325,0.0337370939700421,
0.827117610291581));
#13375=CARTESIAN_POINT('Ctrl Pts',(-0.150764802056544,0.0384861854608708,
0.826765580276784));
#13376=CARTESIAN_POINT('Ctrl Pts',(-0.149745663954339,0.0422781621984397,
0.826477327948062));
#13377=CARTESIAN_POINT('Ctrl Pts',(-0.147850600286118,0.0483957719252788,
0.825999963242419));
#13378=CARTESIAN_POINT('Ctrl Pts',(-0.147060404198409,0.0507463015557448,
0.825813512639377));
#13379=CARTESIAN_POINT('Ctrl Pts',(-0.145134407212981,0.0560519777310876,
0.825385821812431));
#13380=CARTESIAN_POINT('Ctrl Pts',(-0.143963907809761,0.0589933198393297,
0.825143780320487));
#13381=CARTESIAN_POINT('Ctrl Pts',(-0.138437605606369,0.0717343465129827,
0.82407504923337));
#13382=CARTESIAN_POINT('Ctrl Pts',(-0.133164900959068,0.0811042719230291,
0.8232329413188));
#13383=CARTESIAN_POINT('Ctrl Pts',(-0.125293506205099,0.0922267032027333,
0.822204733871579));
#13384=CARTESIAN_POINT('Ctrl Pts',(-0.123550617045382,0.0945487992668807,
0.821988476892715));
#13385=CARTESIAN_POINT('Ctrl Pts',(-0.121493465401088,0.0971354820417315,
0.821746930237558));
#13386=CARTESIAN_POINT('Ctrl Pts',(-0.121242097156666,0.0974490528080551,
0.8217176377196));
#13387=CARTESIAN_POINT('Ctrl Pts',(-0.120763269050626,0.0980416489744151,
0.821662264391206));
#13388=CARTESIAN_POINT('Ctrl Pts',(-0.120536050914056,0.0983208651433942,
0.821636167364445));
#13389=CARTESIAN_POINT('Ctrl Pts',(-0.120141671882216,0.098802074455135,
0.821591183339302));
#13390=CARTESIAN_POINT('Ctrl Pts',(-0.119974966776974,0.0990044372268701,
0.821572263924446));
#13391=CARTESIAN_POINT('Ctrl Pts',(-0.119649911896764,0.0993969935569465,
0.82153555961722));
#13392=CARTESIAN_POINT('Ctrl Pts',(-0.119491620056914,0.0995872305247231,
0.821517770633871));
#13393=CARTESIAN_POINT('Ctrl Pts',(-0.119061618976135,0.100101509545521,
0.821469673446606));
#13394=CARTESIAN_POINT('Ctrl Pts',(-0.118789038484718,0.100424825982833,
0.821439428020346));
#13395=CARTESIAN_POINT('Ctrl Pts',(-0.117762841439244,0.101632006807619,
0.821326452422786));
#13396=CARTESIAN_POINT('Ctrl Pts',(-0.117000625615171,0.102508562819539,
0.821244323976098));
#13397=CARTESIAN_POINT('Ctrl Pts',(-0.110154046709239,0.110206330196331,
0.820521361599731));
#13398=CARTESIAN_POINT('Ctrl Pts',(-0.103488277063102,0.116488533027217,
0.819918595295257));
#13399=CARTESIAN_POINT('Ctrl Pts',(-0.0903949159700552,0.126811937635072,
0.818820801400127));
#13400=CARTESIAN_POINT('Ctrl Pts',(-0.0841511108279415,0.131038506765125,
0.818326983037018));
#13401=CARTESIAN_POINT('Ctrl Pts',(-0.074456218456099,0.136621570717291,
0.817573901214445));
#13402=CARTESIAN_POINT('Ctrl Pts',(-0.0712232535120552,0.138334475174034,
0.817324955649504));
#13403=CARTESIAN_POINT('Ctrl Pts',(-0.0665360277114172,0.140609997373972,
0.816964938170145));
#13404=CARTESIAN_POINT('Ctrl Pts',(-0.0651289138466826,0.141267259595859,
0.816856979135929));
#13405=CARTESIAN_POINT('Ctrl Pts',(-0.0637043666304979,0.141906857644826,
0.81674771167595));
#13406=CARTESIAN_POINT('Ctrl Pts',(-0.0636964963770145,0.141910390471292,
0.816747108002534));
#13407=CARTESIAN_POINT('Ctrl Pts',(-0.0636886258329888,0.141913922641528,
0.816746504307747));
#13408=CARTESIAN_POINT('Ctrl Pts',(-0.0636886325197553,0.141913919640617,
0.802807733721352));
#13409=CARTESIAN_POINT('Ctrl Pts',(-0.0709427906615581,0.138658372804173,
0.803331020463499));
#13410=CARTESIAN_POINT('Ctrl Pts',(-0.0779386900738588,0.13485051276678,
0.803854275908225));
#13411=CARTESIAN_POINT('Ctrl Pts',(-0.0883369135816863,0.128109604884196,
0.804695024206573));
#13412=CARTESIAN_POINT('Ctrl Pts',(-0.0919539666028445,0.125538611030549,
0.805000505086495));
#13413=CARTESIAN_POINT('Ctrl Pts',(-0.0962030810829642,0.122236103760248,
0.805378425520191));
#13414=CARTESIAN_POINT('Ctrl Pts',(-0.0969448704452268,0.121648632939773,
0.805445135611587));
#13415=CARTESIAN_POINT('Ctrl Pts',(-0.0980976888416617,0.120718400825775,
0.805549993675264));
#13416=CARTESIAN_POINT('Ctrl Pts',(-0.0985123967086169,0.120380216546245,
0.805587958223667));
#13417=CARTESIAN_POINT('Ctrl Pts',(-0.0992445678226578,0.119776831509414,
0.805655423274368));
#13418=CARTESIAN_POINT('Ctrl Pts',(-0.099562735511347,0.11951249014297,
0.805684888789684));
#13419=CARTESIAN_POINT('Ctrl Pts',(-0.100293243548118,0.118900624874036,
0.805752886526086));
#13420=CARTESIAN_POINT('Ctrl Pts',(-0.100704836599187,0.118552221273332,
0.80579145442426));
#13421=CARTESIAN_POINT('Ctrl Pts',(-0.101828423077946,0.117591059006142,
0.805897449177747));
#13422=CARTESIAN_POINT('Ctrl Pts',(-0.102536680289723,0.116973988681051,
0.805965053053673));
#13423=CARTESIAN_POINT('Ctrl Pts',(-0.10611526359444,0.113798667284445,
0.806310737500681));
#13424=CARTESIAN_POINT('Ctrl Pts',(-0.108895374065997,0.111141254791816,
0.806592952223893));
#13425=CARTESIAN_POINT('Ctrl Pts',(-0.113011389155491,0.106904088324655,
0.807032961552413));
#13426=CARTESIAN_POINT('Ctrl Pts',(-0.114419155327026,0.105395988561302,
0.807187758456438));
#13427=CARTESIAN_POINT('Ctrl Pts',(-0.125546393482391,0.0929899625007461,
0.808446588180703));
#13428=CARTESIAN_POINT('Ctrl Pts',(-0.133715683730569,0.0808026459482706,
0.809603952325363));
#13429=CARTESIAN_POINT('Ctrl Pts',(-0.14125501705106,0.065194313414932,
0.810909774768515));
#13430=CARTESIAN_POINT('Ctrl Pts',(-0.142379234602237,0.0627011513930527,
0.811113217928002));
#13431=CARTESIAN_POINT('Ctrl Pts',(-0.143649058715307,0.05967453594177,
0.811353034189395));
#13432=CARTESIAN_POINT('Ctrl Pts',(-0.143858232142606,0.0591684998854224,
0.811392893765217));
#13433=CARTESIAN_POINT('Ctrl Pts',(-0.144178764846738,0.0583813129063918,
0.811454521108485));
#13434=CARTESIAN_POINT('Ctrl Pts',(-0.1442919809195,0.0581009309390728,
0.811476397570913));
#13435=CARTESIAN_POINT('Ctrl Pts',(-0.144500117926105,0.0575811145710233,
0.811516816215091));
#13436=CARTESIAN_POINT('Ctrl Pts',(-0.144595260912915,0.0573417767373752,
0.811535371262656));
#13437=CARTESIAN_POINT('Ctrl Pts',(-0.144808541586246,0.0568013502459086,
0.811577146044424));
#13438=CARTESIAN_POINT('Ctrl Pts',(-0.14492633467931,0.0565001294483033,
0.811600344949062));
#13439=CARTESIAN_POINT('Ctrl Pts',(-0.145269826322503,0.0556136095581081,
0.811668377051388));
#13440=CARTESIAN_POINT('Ctrl Pts',(-0.145492928506876,0.0550273004801538,
0.811713058462969));
#13441=CARTESIAN_POINT('Ctrl Pts',(-0.147034079437659,0.0509022748581949,
0.812025339882027));
#13442=CARTESIAN_POINT('Ctrl Pts',(-0.148226566933849,0.0473175752641455,
0.812286019783897));
#13443=CARTESIAN_POINT('Ctrl Pts',(-0.150546706777027,0.0393902057793274,
0.812846743677707));
#13444=CARTESIAN_POINT('Ctrl Pts',(-0.151619423201953,0.035035050228785,
0.813144787003368));
#13445=CARTESIAN_POINT('Ctrl Pts',(-0.154523603333601,0.0205799691305764,
0.814118814957486));
#13446=CARTESIAN_POINT('Ctrl Pts',(-0.155544297372826,0.0103459061205155,
0.814786177014324));
#13447=CARTESIAN_POINT('Ctrl Pts',(-0.155552455097302,-0.00439252726531829,
0.815785205400792));
#13448=CARTESIAN_POINT('Ctrl Pts',(-0.155361511363309,-0.00886875882136496,
0.816093330688297));
#13449=CARTESIAN_POINT('Ctrl Pts',(-0.154900791593397,-0.0142251221010313,
0.816470581476357));
#13450=CARTESIAN_POINT('Ctrl Pts',(-0.154816066085496,-0.0151193570196231,
0.816533846500607));
#13451=CARTESIAN_POINT('Ctrl Pts',(-0.154664159269177,-0.0165871566664824,
0.816638179465917));
#13452=CARTESIAN_POINT('Ctrl Pts',(-0.154601519529247,-0.0171611792037266,
0.816679104912957));
#13453=CARTESIAN_POINT('Ctrl Pts',(-0.154483115989479,-0.0181929099523547,
0.816752890858028));
#13454=CARTESIAN_POINT('Ctrl Pts',(-0.154428510129127,-0.0186507466140799,
0.816785714614313));
#13455=CARTESIAN_POINT('Ctrl Pts',(-0.154307836239588,-0.01962564367355,
0.816855783631093));
#13456=CARTESIAN_POINT('Ctrl Pts',(-0.154241203240571,-0.020142627068871,
0.816893046291902));
#13457=CARTESIAN_POINT('Ctrl Pts',(-0.154054671119672,-0.0215346432984295,
0.816993668450051));
#13458=CARTESIAN_POINT('Ctrl Pts',(-0.153929917372611,-0.0224089944816921,
0.817057180053865));
#13459=CARTESIAN_POINT('Ctrl Pts',(-0.153268283597083,-0.0267796160757041,
0.817376247106298));
#13460=CARTESIAN_POINT('Ctrl Pts',(-0.152619741702651,-0.030257647847939,
0.81763529468849));
#13461=CARTESIAN_POINT('Ctrl Pts',(-0.148587157058356,-0.0484230483110955,
0.819016926138375));
#13462=CARTESIAN_POINT('Ctrl Pts',(-0.143200185747883,-0.0625817613357571,
0.820204298025277));
#13463=CARTESIAN_POINT('Ctrl Pts',(-0.135054226686732,-0.0771940898268286,
0.821483759793902));
#13464=CARTESIAN_POINT('Ctrl Pts',(-0.134220652250412,-0.0786345251007929,
0.821610391617838));
#13465=CARTESIAN_POINT('Ctrl Pts',(-0.131812124365683,-0.0826465874672812,
0.821964030214036));
#13466=CARTESIAN_POINT('Ctrl Pts',(-0.130185166594307,-0.0851863849767095,
0.822188999421818));
#13467=CARTESIAN_POINT('Ctrl Pts',(-0.128182609646554,-0.0881209928235368,
0.822448873342377));
#13468=CARTESIAN_POINT('Ctrl Pts',(-0.127877663750674,-0.0885629376675909,
0.822488007609831));
#13469=CARTESIAN_POINT('Ctrl Pts',(-0.12738020199926,-0.0892759607469687,
0.822551131123704));
#13470=CARTESIAN_POINT('Ctrl Pts',(-0.12718909831537,-0.0895480111672114,
0.82257521207778));
#13471=CARTESIAN_POINT('Ctrl Pts',(-0.126847969571038,-0.0900303384188775,
0.82261789677546));
#13472=CARTESIAN_POINT('Ctrl Pts',(-0.126698291884646,-0.0902408558108802,
0.822636523724232));
#13473=CARTESIAN_POINT('Ctrl Pts',(-0.126375972988033,-0.090691805360956,
0.822676416878256));
#13474=CARTESIAN_POINT('Ctrl Pts',(-0.12620317014697,-0.090932117302656,
0.822697671694038));
#13475=CARTESIAN_POINT('Ctrl Pts',(-0.125725852467355,-0.0915919277272215,
0.822756022354877));
#13476=CARTESIAN_POINT('Ctrl Pts',(-0.125419921178669,-0.0920104048217402,
0.822793022270224));
#13477=CARTESIAN_POINT('Ctrl Pts',(-0.123759236309898,-0.0942583479850944,
0.8229917778906));
#13478=CARTESIAN_POINT('Ctrl Pts',(-0.122366446299144,-0.0960595598146429,
0.823151043812595));
#13479=CARTESIAN_POINT('Ctrl Pts',(-0.111982900638586,-0.108895431375117,
0.824291448241559));
#13480=CARTESIAN_POINT('Ctrl Pts',(-0.101553880412221,-0.118681529749294,
0.82519605490586));
#13481=CARTESIAN_POINT('Ctrl Pts',(-0.0846187913805061,-0.130682682624514,
0.826584003385049));
#13482=CARTESIAN_POINT('Ctrl Pts',(-0.0790686870865399,-0.134113490818743,
0.827027473250179));
#13483=CARTESIAN_POINT('Ctrl Pts',(-0.0724426566541869,-0.137654837279197,
0.827553875014385));
#13484=CARTESIAN_POINT('Ctrl Pts',(-0.0715605733508693,-0.138115448048711,
0.827623883288218));
#13485=CARTESIAN_POINT('Ctrl Pts',(-0.0701394623203017,-0.138840262839448,
0.827736594791734));
#13486=CARTESIAN_POINT('Ctrl Pts',(-0.0696032084020613,-0.139109870684167,
0.827779108678171));
#13487=CARTESIAN_POINT('Ctrl Pts',(-0.0686486856653592,-0.139582867008537,
0.827854758252922));
#13488=CARTESIAN_POINT('Ctrl Pts',(-0.0682310372095184,-0.139787497146982,
0.827887850247378));
#13489=CARTESIAN_POINT('Ctrl Pts',(-0.0673593652842269,-0.140209742529195,
0.827956902629154));
#13490=CARTESIAN_POINT('Ctrl Pts',(-0.0669051910952876,-0.140427032244889,
0.827992873825742));
#13491=CARTESIAN_POINT('Ctrl Pts',(-0.0657239834923578,-0.140985124092878,
0.828086411938883));
#13492=CARTESIAN_POINT('Ctrl Pts',(-0.0649953599545144,-0.141322504793454,
0.828144095878418));
#13493=CARTESIAN_POINT('Ctrl Pts',(-0.0618310977143198,-0.142758033364856,
0.828394570910129));
#13494=CARTESIAN_POINT('Ctrl Pts',(-0.0593701409965125,-0.143798906282152,
0.828589297226851));
#13495=CARTESIAN_POINT('Ctrl Pts',(-0.0527794287756847,-0.146388456857322,
0.829110996714711));
#13496=CARTESIAN_POINT('Ctrl Pts',(-0.0486087857251568,-0.147825666584394,
0.829441392899277));
#13497=CARTESIAN_POINT('Ctrl Pts',(-0.0324785437779717,-0.152627732754861,
0.830719496252659));
#13498=CARTESIAN_POINT('Ctrl Pts',(-0.0201937776026256,-0.154732834173996,
0.831697851186547));
#13499=CARTESIAN_POINT('Ctrl Pts',(-0.00393590476244397,-0.155548075948361,
0.832936736987945));
#13500=CARTESIAN_POINT('Ctrl Pts',(-7.53493148768674E-5,-0.155597866005134,
0.833226408301307));
#13501=CARTESIAN_POINT('Ctrl Pts',(0.0044138863096793,-0.155488642039542,
0.833555183720977));
#13502=CARTESIAN_POINT('Ctrl Pts',(0.00504424633625328,-0.155469469064192,
0.833601163124359));
#13503=CARTESIAN_POINT('Ctrl Pts',(0.00599841733932474,-0.15543463758223,
0.833670463127406));
#13504=CARTESIAN_POINT('Ctrl Pts',(0.00632231426643907,-0.155421800010246,
0.833693935148018));
#13505=CARTESIAN_POINT('Ctrl Pts',(0.00690353988906549,-0.155396943329064,
0.833735958797997));
#13506=CARTESIAN_POINT('Ctrl Pts',(0.0071608796303466,-0.155385297455609,
0.833754530829436));
#13507=CARTESIAN_POINT('Ctrl Pts',(0.00771967261606659,-0.155358618204026,
0.833794784235462));
#13508=CARTESIAN_POINT('Ctrl Pts',(0.0080211105724575,-0.155343346767629,
0.833816452121388));
#13509=CARTESIAN_POINT('Ctrl Pts',(0.00886673077742968,-0.155298038032034,
0.833877110850549));
#13510=CARTESIAN_POINT('Ctrl Pts',(0.00941080975329047,-0.155266017578841,
0.833915992814396));
#13511=CARTESIAN_POINT('Ctrl Pts',(0.0126394141179972,-0.155058972439274,
0.834145912635973));
#13512=CARTESIAN_POINT('Ctrl Pts',(0.0153194110167562,-0.154817175170915,
0.834333445651806));
#13513=CARTESIAN_POINT('Ctrl Pts',(0.032526643533326,-0.152813417442147,
0.835523968622352));
#13514=CARTESIAN_POINT('Ctrl Pts',(0.0467510858564298,-0.149078380392629,
0.836451973434921));
#13515=CARTESIAN_POINT('Ctrl Pts',(0.0620926028731287,-0.14263353916533,
0.83757012416017));
#13516=CARTESIAN_POINT('Ctrl Pts',(0.0639248085375822,-0.141821846693957,
0.837705565229497));
#13517=CARTESIAN_POINT('Ctrl Pts',(0.0692837532519598,-0.139322814073107,
0.838108170870832));
#13518=CARTESIAN_POINT('Ctrl Pts',(0.0727629080939486,-0.137537775797823,
0.838377997886358));
#13519=CARTESIAN_POINT('Ctrl Pts',(0.0769945146879745,-0.135161161205173,
0.838718771506387));
#13520=CARTESIAN_POINT('Ctrl Pts',(0.0778138720512623,-0.13469111342838,
0.838785356458359));
#13521=CARTESIAN_POINT('Ctrl Pts',(0.0790952059883833,-0.133940445661322,
0.83889045999301));
#13522=CARTESIAN_POINT('Ctrl Pts',(0.079560098018765,-0.133664824782526,
0.838928797836794));
#13523=CARTESIAN_POINT('Ctrl Pts',(0.0803782271988722,-0.133173999623865,
0.838996632307444));
#13524=CARTESIAN_POINT('Ctrl Pts',(0.0807320621206994,-0.13295979739428,
0.839026092213123));
#13525=CARTESIAN_POINT('Ctrl Pts',(0.0815407046839779,-0.132465848757613,
0.839093701593312));
#13526=CARTESIAN_POINT('Ctrl Pts',(0.0819949324661616,-0.132185168018858,
0.839131885042975));
#13527=CARTESIAN_POINT('Ctrl Pts',(0.0832455603812954,-0.131403441636436,
0.839237593024821));
#13528=CARTESIAN_POINT('Ctrl Pts',(0.0840388617350304,-0.13089750739833,
0.839305297166802));
#13529=CARTESIAN_POINT('Ctrl Pts',(0.0884737547136953,-0.128012186217781,
0.839687532650347));
#13530=CARTESIAN_POINT('Ctrl Pts',(0.0920185161390474,-0.125488289565871,
0.840007432816153));
#13531=CARTESIAN_POINT('Ctrl Pts',(0.1028726715123,-0.11705267662579,0.841034965171198));
#13532=CARTESIAN_POINT('Ctrl Pts',(0.109753981186708,-0.110626101523787,
0.841760971940625));
#13533=CARTESIAN_POINT('Ctrl Pts',(0.119829474337633,-0.099345516845188,
0.842933955167288));
#13534=CARTESIAN_POINT('Ctrl Pts',(0.123407606928729,-0.0948641356758045,
0.843378004460806));
#13535=CARTESIAN_POINT('Ctrl Pts',(0.128835816830005,-0.0872371376000215,
0.844089218141352));
#13536=CARTESIAN_POINT('Ctrl Pts',(0.130837181388826,-0.0842058382742902,
0.844361327493607));
#13537=CARTESIAN_POINT('Ctrl Pts',(0.133026188114896,-0.0806235494867982,
0.844668630867109));
#13538=CARTESIAN_POINT('Ctrl Pts',(0.133318951404708,-0.080138509338658,
0.844709945323327));
#13539=CARTESIAN_POINT('Ctrl Pts',(0.133781960304958,-0.0793618523010465,
0.844775617713906));
#13540=CARTESIAN_POINT('Ctrl Pts',(0.133953913974725,-0.0790712681092836,
0.844800082121021));
#13541=CARTESIAN_POINT('Ctrl Pts',(0.134256399066179,-0.0785562804696079,
0.844843247585486));
#13542=CARTESIAN_POINT('Ctrl Pts',(0.134387316463537,-0.0783321075256524,
0.844861973416464));
#13543=CARTESIAN_POINT('Ctrl Pts',(0.134663092547841,-0.0778571632652931,
0.844901510768642));
#13544=CARTESIAN_POINT('Ctrl Pts',(0.134807812090975,-0.0776063152665721,
0.844922313309607));
#13545=CARTESIAN_POINT('Ctrl Pts',(0.13519527533038,-0.0769303559597684,
0.844978160074161));
#13546=CARTESIAN_POINT('Ctrl Pts',(0.135436716976263,-0.0765044956311639,
0.845013121595415));
#13547=CARTESIAN_POINT('Ctrl Pts',(0.136608966385062,-0.0744139130601118,
0.845183700495456));
#13548=CARTESIAN_POINT('Ctrl Pts',(0.137511166073088,-0.0727332128514912,
0.845317589070989));
#13549=CARTESIAN_POINT('Ctrl Pts',(0.14000720524231,-0.0678707992849482,
0.845696979603526));
#13550=CARTESIAN_POINT('Ctrl Pts',(0.141523173141172,-0.0646502775005473,
0.845938695814096));
#13551=CARTESIAN_POINT('Ctrl Pts',(0.148684157789354,-0.0479755392683395,
0.847156338429439));
#13552=CARTESIAN_POINT('Ctrl Pts',(0.152526471659468,-0.0338279864847041,
0.848086812223037));
#13553=CARTESIAN_POINT('Ctrl Pts',(0.15446835579267,-0.0183403555419018,
0.849154448954754));
#13554=CARTESIAN_POINT('Ctrl Pts',(0.154585224745113,-0.0173277176048889,
0.849224433192257));
#13555=CARTESIAN_POINT('Ctrl Pts',(0.154919424531863,-0.014158782569299,
0.849444090304843));
#13556=CARTESIAN_POINT('Ctrl Pts',(0.155101642279014,-0.0119991245545318,
0.849594730634901));
#13557=CARTESIAN_POINT('Ctrl Pts',(0.15529624999085,-0.00892783001396077,
0.849810637341172));
#13558=CARTESIAN_POINT('Ctrl Pts',(0.155345843864133,-0.00801873690103627,
0.849874752560793));
#13559=CARTESIAN_POINT('Ctrl Pts',(0.155414015532305,-0.00652870903575065,
0.849980203060855));
#13560=CARTESIAN_POINT('Ctrl Pts',(0.155437323399908,-0.00594800329527819,
0.850021390534172));
#13561=CARTESIAN_POINT('Ctrl Pts',(0.155473298004804,-0.00490602040753982,
0.850095463174784));
#13562=CARTESIAN_POINT('Ctrl Pts',(0.155487167538701,-0.00444478920921299,
0.850128310394621));
#13563=CARTESIAN_POINT('Ctrl Pts',(0.15551227255689,-0.00346479740739736,
0.850198230833581));
#13564=CARTESIAN_POINT('Ctrl Pts',(0.155522964970464,-0.0029460298091664,
0.850235320609249));
#13565=CARTESIAN_POINT('Ctrl Pts',(0.155544675222567,-0.00155488572332244,
0.850334992998728));
#13566=CARTESIAN_POINT('Ctrl Pts',(0.155550949349555,-0.00068246506152315,
0.85039772280156));
#13567=CARTESIAN_POINT('Ctrl Pts',(0.155545725178648,0.00359569501132507,
0.850706469466919));
#13568=CARTESIAN_POINT('Ctrl Pts',(0.15542971592967,0.00700011914161767,
0.850955712691444));
#13569=CARTESIAN_POINT('Ctrl Pts',(0.154187477041494,0.0255423929228684,
0.852334013408533));
#13570=CARTESIAN_POINT('Ctrl Pts',(0.150961455966671,0.0404556384175158,
0.853529659254922));
#13571=CARTESIAN_POINT('Ctrl Pts',(0.145139469463207,0.0559667988643988,
0.854797088651043));
#13572=CARTESIAN_POINT('Ctrl Pts',(0.144631747907989,0.0572660971600335,
0.854903354439001));
#13573=CARTESIAN_POINT('Ctrl Pts',(0.142863363931482,0.0616179186166481,
0.8552592567934));
#13574=CARTESIAN_POINT('Ctrl Pts',(0.141522883046087,0.0646373450244673,
0.855506170260098));
#13575=CARTESIAN_POINT('Ctrl Pts',(0.13984744555462,0.0681087263205664,
0.855788219469132));
#13576=CARTESIAN_POINT('Ctrl Pts',(0.139605092773141,0.0686041159511367,
0.855828425231567));
#13577=CARTESIAN_POINT('Ctrl Pts',(0.139212079184579,0.0693967618156155,
0.855892672430234));
#13578=CARTESIAN_POINT('Ctrl Pts',(0.1390630919076,0.0696948349315154,0.855916813346368));
#13579=CARTESIAN_POINT('Ctrl Pts',(0.138796597856358,0.0702237425100022,
0.855959612467863));
#13580=CARTESIAN_POINT('Ctrl Pts',(0.138679471242554,0.0704547645557252,
0.855978293998204));
#13581=CARTESIAN_POINT('Ctrl Pts',(0.138429029649834,0.0709456945210096,
0.856017964958107));
#13582=CARTESIAN_POINT('Ctrl Pts',(0.138295559756299,0.0712055192832181,
0.856038944448093));
#13583=CARTESIAN_POINT('Ctrl Pts',(0.137931281503052,0.0719097689075282,
0.856095768671674));
#13584=CARTESIAN_POINT('Ctrl Pts',(0.137699054842487,0.0723534629124167,
0.856131525639183));
#13585=CARTESIAN_POINT('Ctrl Pts',(0.136508579364141,0.0746015020393035,
0.856312511341029));
#13586=CARTESIAN_POINT('Ctrl Pts',(0.135516934222805,0.0763880747952177,
0.856455747372342));
#13587=CARTESIAN_POINT('Ctrl Pts',(0.132510650857198,0.0815613524984651,
0.856870307278052));
#13588=CARTESIAN_POINT('Ctrl Pts',(0.130402097041442,0.0848918432503784,
0.857136953144764));
#13589=CARTESIAN_POINT('Ctrl Pts',(0.1222134458951,0.0967995525154898,0.858103081685175));
#13590=CARTESIAN_POINT('Ctrl Pts',(0.115395229838299,0.104834312919997,
0.858782169934589));
#13591=CARTESIAN_POINT('Ctrl Pts',(0.103094447859705,0.116663161575551,
0.859923095134347));
#13592=CARTESIAN_POINT('Ctrl Pts',(0.0980884836985785,0.120902398137326,
0.860368849358707));
#13593=CARTESIAN_POINT('Ctrl Pts',(0.092031441662467,0.125407368982369,
0.860897742754843));
#13594=CARTESIAN_POINT('Ctrl Pts',(0.0912266068626585,0.125994049733277,
0.860967811126981));
#13595=CARTESIAN_POINT('Ctrl Pts',(0.0899275998023373,0.126921983353701,
0.861080600919101));
#13596=CARTESIAN_POINT('Ctrl Pts',(0.089436979016023,0.1272681807477,0.861123132572274));
#13597=CARTESIAN_POINT('Ctrl Pts',(0.0885627884640505,0.127877485668954,
0.861198802598185));
#13598=CARTESIAN_POINT('Ctrl Pts',(0.0881800175851144,0.128141731421221,
0.861231897196103));
#13599=CARTESIAN_POINT('Ctrl Pts',(0.0877948238505663,0.128405106624818,
0.861265164810487));
#13600=CARTESIAN_POINT('Ctrl Pts',(0.0877935766114245,0.128405959394635,
0.86126527252907));
#13601=CARTESIAN_POINT('Ctrl Pts',(0.0877910927589434,0.128407657616026,
0.861265487047772));
#13602=CARTESIAN_POINT('Ctrl Pts',(0.0877898561428815,0.128408503069914,
0.861265593848131));
#13603=CARTESIAN_POINT('Ctrl Pts',(0.0877873934459118,0.128410186722777,
0.861265806538233));
#13604=CARTESIAN_POINT('Ctrl Pts',(0.0877861673595772,0.128411024925908,
0.861265912428451));
#13605=CARTESIAN_POINT('Ctrl Pts',(0.0877837256161923,0.128412694150966,
0.861266123307431));
#13606=CARTESIAN_POINT('Ctrl Pts',(0.0877825099604475,0.128413525172438,
0.861266228296087));
#13607=CARTESIAN_POINT('Ctrl Pts',(0.0877800889905027,0.128415180095466,
0.861266437379541));
#13608=CARTESIAN_POINT('Ctrl Pts',(0.0877788836737805,0.128416003999176,
0.861266541474563));
#13609=CARTESIAN_POINT('Ctrl Pts',(0.087776483278764,0.128417644758453,
0.861266748779673));
#13610=CARTESIAN_POINT('Ctrl Pts',(0.0877752882036578,0.128418461612263,
0.861266851989492));
#13611=CARTESIAN_POINT('Ctrl Pts',(0.0877729082047907,0.128420088332524,
0.861267057531733));
#13612=CARTESIAN_POINT('Ctrl Pts',(0.0877717232793406,0.128420898200545,
0.861267159864309));
#13613=CARTESIAN_POINT('Ctrl Pts',(0.0877693634909101,0.128422511011214,
0.861267363659757));
#13614=CARTESIAN_POINT('Ctrl Pts',(0.0877681886245434,0.128423313956585,
0.861267465122928));
#13615=CARTESIAN_POINT('Ctrl Pts',(0.087765848859657,0.128424912987841,
0.861267667187758));
#13616=CARTESIAN_POINT('Ctrl Pts',(0.0877646839608254,0.128425709074341,
0.861267767789449));
#13617=CARTESIAN_POINT('Ctrl Pts',(0.0877623640347443,0.128427294454839,
0.86126796813965));
#13618=CARTESIAN_POINT('Ctrl Pts',(0.0877612090095433,0.128428083747832,
0.861268067887988));
#13619=CARTESIAN_POINT('Ctrl Pts',(0.0877589087537019,0.128429655595129,
0.861268266538151));
#13620=CARTESIAN_POINT('Ctrl Pts',(0.0877577635171766,0.12843043815384,
0.86126836544049));
#13621=CARTESIAN_POINT('Ctrl Pts',(0.0877554827392267,0.128431996601691,
0.861268562407259));
#13622=CARTESIAN_POINT('Ctrl Pts',(0.0877543471980134,0.128432772491066,
0.861268660471678));
#13623=CARTESIAN_POINT('Ctrl Pts',(0.0877520857370583,0.128434317651691,
0.861268855768982));
#13624=CARTESIAN_POINT('Ctrl Pts',(0.0877509598099265,0.128435086928363,
0.861268953002512));
#13625=CARTESIAN_POINT('Ctrl Pts',(0.0877487174695555,0.128436618938199,
0.861269146647345));
#13626=CARTESIAN_POINT('Ctrl Pts',(0.0877476010615809,0.128437381668133,
0.861269243058199));
#13627=CARTESIAN_POINT('Ctrl Pts',(0.0877453776883554,0.128438900634212,
0.861269435063842));
#13628=CARTESIAN_POINT('Ctrl Pts',(0.0877442707177036,0.128439656874407,
0.861269530659104));
#13629=CARTESIAN_POINT('Ctrl Pts',(0.0877420661286834,0.128441162923872,
0.861269721041388));
#13630=CARTESIAN_POINT('Ctrl Pts',(0.0877409685077732,0.128441912735231,
0.861269815828635));
#13631=CARTESIAN_POINT('Ctrl Pts',(0.0877387825411712,0.128443405980728,
0.861270004601562));
#13632=CARTESIAN_POINT('Ctrl Pts',(0.0877376941896687,0.128444149419183,
0.861270098587747));
#13633=CARTESIAN_POINT('Ctrl Pts',(0.0877355266612734,0.128445629988633,
0.861270285767254));
#13634=CARTESIAN_POINT('Ctrl Pts',(0.0877344474885076,0.128446367117152,
0.861270378960224));
#13635=CARTESIAN_POINT('Ctrl Pts',(0.0877322982490207,0.128447835114586,
0.861270564559233));
#13636=CARTESIAN_POINT('Ctrl Pts',(0.0877312281761717,0.128448565988023,
0.861270656965807));
#13637=CARTESIAN_POINT('Ctrl Pts',(0.0877290970522117,0.128450021533881,
0.86127084099932));
#13638=CARTESIAN_POINT('Ctrl Pts',(0.0877280359977181,0.128450746208942,
0.861270932626556));
#13639=CARTESIAN_POINT('Ctrl Pts',(0.0877259228208885,0.128452189420214,
0.861271115109143));
#13640=CARTESIAN_POINT('Ctrl Pts',(0.0877248707003412,0.128452907955529,
0.861271205964345));
#13641=CARTESIAN_POINT('Ctrl Pts',(0.0877227753123451,0.12845433894227,
0.861271386909705));
#13642=CARTESIAN_POINT('Ctrl Pts',(0.0877217320434193,0.128455051395024,
0.861271476999995));
#13643=CARTESIAN_POINT('Ctrl Pts',(0.0877196542919911,0.128456470263131,
0.861271656421302));
#13644=CARTESIAN_POINT('Ctrl Pts',(0.0877186198002404,0.128457176685111,
0.861271745753123));
#13645=CARTESIAN_POINT('Ctrl Pts',(0.0877165595105252,0.128458583555865,
0.861271923665505));
#13646=CARTESIAN_POINT('Ctrl Pts',(0.0877155337124031,0.128459284005053,
0.861272012246084));
#13647=CARTESIAN_POINT('Ctrl Pts',(0.0877134907367074,0.128460678981151,
0.861272188662321));
#13648=CARTESIAN_POINT('Ctrl Pts',(0.0877124735553404,0.128461373510953,
0.86127227649831));
#13649=CARTESIAN_POINT('Ctrl Pts',(0.0877104477309279,0.128462756705325,
0.86127245143248));
#13650=CARTESIAN_POINT('Ctrl Pts',(0.0877094390854991,0.12846344537182,
0.861272538530871));
#13651=CARTESIAN_POINT('Ctrl Pts',(0.0877074302697687,0.128464816883613,
0.861272711995315));
#13652=CARTESIAN_POINT('Ctrl Pts',(0.0877064300894679,0.128465499736029,
0.861272798362234));
#13653=CARTESIAN_POINT('Ctrl Pts',(0.0877044381113941,0.128466859683759,
0.861272970371744));
#13654=CARTESIAN_POINT('Ctrl Pts',(0.087703446314811,0.128467536778546,
0.861273056014235));
#13655=CARTESIAN_POINT('Ctrl Pts',(0.0877014710344858,0.128468885259447,
0.861273226580917));
#13656=CARTESIAN_POINT('Ctrl Pts',(0.0877004875479138,0.128469556647775,
0.861273311505356));
#13657=CARTESIAN_POINT('Ctrl Pts',(0.0876985288094731,0.128470893769944,
0.861273480642693));
#13658=CARTESIAN_POINT('Ctrl Pts',(0.0876975535564825,0.128471559504826,
0.861273564855692));
#13659=CARTESIAN_POINT('Ctrl Pts',(0.087695611214741,0.12847288536903,0.861273732576245));
#13660=CARTESIAN_POINT('Ctrl Pts',(0.0876946441219777,0.128473545501362,
0.86127381608415));
#13661=CARTESIAN_POINT('Ctrl Pts',(0.087692718027213,0.128474860211434,
0.861273982400871));
#13662=CARTESIAN_POINT('Ctrl Pts',(0.0876917590208031,0.128475514792451,
0.861274065210072));
#13663=CARTESIAN_POINT('Ctrl Pts',(0.0876898490282865,0.128476818448784,
0.861274230135481));
#13664=CARTESIAN_POINT('Ctrl Pts',(0.0876888980361884,0.128477467528452,
0.861274312252211));
#13665=CARTESIAN_POINT('Ctrl Pts',(0.0876870040011461,0.128478760231434,
0.861274475798832));
#13666=CARTESIAN_POINT('Ctrl Pts',(0.0876860609528391,0.128479403858666,
0.86127455722919));
#13667=CARTESIAN_POINT('Ctrl Pts',(0.0876841827247945,0.128480685712548,
0.861274719410038));
#13668=CARTESIAN_POINT('Ctrl Pts',(0.0876832475450118,0.128481323939481,
0.861274800160536));
#13669=CARTESIAN_POINT('Ctrl Pts',(0.0876813849900348,0.128482595037186,
0.861274960987198));
#13670=CARTESIAN_POINT('Ctrl Pts',(0.0876804576085012,0.128483227912534,
0.861275041063914));
#13671=CARTESIAN_POINT('Ctrl Pts',(0.0876786105905786,0.12848448834838,
0.861275200548155));
#13672=CARTESIAN_POINT('Ctrl Pts',(0.087677690942862,0.128485115916853,
0.861275279956663));
#13673=CARTESIAN_POINT('Ctrl Pts',(0.0876758593060191,0.128486365798749,
0.861275438111973));
#13674=CARTESIAN_POINT('Ctrl Pts',(0.0876749473174137,0.128486988112055,
0.861275516858734));
#13675=CARTESIAN_POINT('Ctrl Pts',(0.0876731309353678,0.128488227527615,
0.861275673696038));
#13676=CARTESIAN_POINT('Ctrl Pts',(0.0876722265382817,0.128488844632593,
0.861275751786898));
#13677=CARTESIAN_POINT('Ctrl Pts',(0.0876704252715704,0.128490073678399,
0.861275907318257));
#13678=CARTESIAN_POINT('Ctrl Pts',(0.0876695283974716,0.128490685622513,
0.861275984759145));
#13679=CARTESIAN_POINT('Ctrl Pts',(0.087667943279937,0.128491767136107,
0.861276121626291));
#13680=CARTESIAN_POINT('Ctrl Pts',(0.0876672550322583,0.128492236714143,
0.861276181052995));
#13681=CARTESIAN_POINT('Ctrl Pts',(0.0876658796485813,0.128493175095536,
0.861276299810186));
#13682=CARTESIAN_POINT('Ctrl Pts',(0.0876651926736389,0.128493643789042,
0.861276359126766));
#13683=CARTESIAN_POINT('Ctrl Pts',(0.0876638200525214,0.128494580253363,
0.861276477644964));
#13684=CARTESIAN_POINT('Ctrl Pts',(0.0876631344019249,0.128495048027225,
0.861276536846963));
#13685=CARTESIAN_POINT('Ctrl Pts',(0.0876617644256033,0.128495982655008,
0.861276655136339));
#13686=CARTESIAN_POINT('Ctrl Pts',(0.087661080096343,0.128496449511373,
0.86127671422402));
#13687=CARTESIAN_POINT('Ctrl Pts',(0.087659712755036,0.128497382309478,
0.861276832285421));
#13688=CARTESIAN_POINT('Ctrl Pts',(0.0876590297427072,0.128497848251442,
0.861276891259165));
#13689=CARTESIAN_POINT('Ctrl Pts',(0.0876576650304796,0.128498779224104,
0.861277009093106));
#13690=CARTESIAN_POINT('Ctrl Pts',(0.0876569833317044,0.128499244254066,
0.861277067953206));
#13691=CARTESIAN_POINT('Ctrl Pts',(0.0876556212358863,0.128500173410113,
0.861277185560784));
#13692=CARTESIAN_POINT('Ctrl Pts',(0.0876549408425665,0.128500637533689,
0.861277244307941));
#13693=CARTESIAN_POINT('Ctrl Pts',(0.0876535813695065,0.128501564868973,
0.86127736168861));
#13694=CARTESIAN_POINT('Ctrl Pts',(0.0876529022830971,0.128502028085262,
0.861277420322699));
#13695=CARTESIAN_POINT('Ctrl Pts',(0.0876515454120886,0.128502953614093,
0.861277537478251));
#13696=CARTESIAN_POINT('Ctrl Pts',(0.0876508676260698,0.128503415927633,
0.861277595999836));
#13697=CARTESIAN_POINT('Ctrl Pts',(0.0876495133582066,0.128504339649445,
0.861277712930177));
#13698=CARTESIAN_POINT('Ctrl Pts',(0.0876488368718639,0.128504801060816,
0.861277771339322));
#13699=CARTESIAN_POINT('Ctrl Pts',(0.0876474851919838,0.128505722986133,
0.861277888045766));
#13700=CARTESIAN_POINT('Ctrl Pts',(0.0876468099999454,0.128506183499088,
0.861277946342935));
#13701=CARTESIAN_POINT('Ctrl Pts',(0.0876454609008248,0.128507103633018,
0.861278062826107));
#13702=CARTESIAN_POINT('Ctrl Pts',(0.0876447869963007,0.128507563252279,
0.861278121011888));
#13703=CARTESIAN_POINT('Ctrl Pts',(0.087643440482064,0.128508481592188,
0.861278237271435));
#13704=CARTESIAN_POINT('Ctrl Pts',(0.0876427678667361,0.128508940316696,
0.861278295345685));
#13705=CARTESIAN_POINT('Ctrl Pts',(0.0876414239146435,0.128509856878272,
0.861278411383572));
#13706=CARTESIAN_POINT('Ctrl Pts',(0.0876407525802623,0.128510314713744,
0.861278469347003));
#13707=CARTESIAN_POINT('Ctrl Pts',(0.0876394111951554,0.128511229493862,
0.861278585162816));
#13708=CARTESIAN_POINT('Ctrl Pts',(0.08763874114114,0.128511686440782,0.861278643015481));
#13709=CARTESIAN_POINT('Ctrl Pts',(0.087637402309562,0.128512599448798,
0.861278758610382));
#13710=CARTESIAN_POINT('Ctrl Pts',(0.0876367335323633,0.128513055509675,
0.861278816352588));
#13711=CARTESIAN_POINT('Ctrl Pts',(0.087635397241258,0.128513966754667,
0.86127893172771));
#13712=CARTESIAN_POINT('Ctrl Pts',(0.0876347297317331,0.128514421935823,
0.861278989360247));
#13713=CARTESIAN_POINT('Ctrl Pts',(0.0876333959916878,0.128515331410747,
0.861279104514676));
#13714=CARTESIAN_POINT('Ctrl Pts',(0.0876327297531324,0.128515785710023,
0.861279162037262));
#13715=CARTESIAN_POINT('Ctrl Pts',(0.0876313985378597,0.12851669343298,
0.861279276973271));
#13716=CARTESIAN_POINT('Ctrl Pts',(0.0876307335615464,0.128517146856413,
0.86127933438666));
#13717=CARTESIAN_POINT('Ctrl Pts',(0.0876294048798295,0.128518052821587,
0.861279449103494));
#13718=CARTESIAN_POINT('Ctrl Pts',(0.0876287411680163,0.128518505367725,
0.861279506407492));
#13719=CARTESIAN_POINT('Ctrl Pts',(0.0876274149972206,0.128519409590722,
0.861279620907107));
#13720=CARTESIAN_POINT('Ctrl Pts',(0.0876267525426929,0.12851986126457,
0.861279678102338));
#13721=CARTESIAN_POINT('Ctrl Pts',(0.0876254288821741,0.128520763746001,
0.861279792384792));
#13722=CARTESIAN_POINT('Ctrl Pts',(0.0876247676807267,0.128521214550513,
0.861279849471622));
#13723=CARTESIAN_POINT('Ctrl Pts',(0.0876234465214615,0.128522115296701,
0.861279963537696));
#13724=CARTESIAN_POINT('Ctrl Pts',(0.0876227865665,0.128522565236457,0.861280020516694));
#13725=CARTESIAN_POINT('Ctrl Pts',(0.0876214679117838,0.128523464245327,
0.861280134366106));
#13726=CARTESIAN_POINT('Ctrl Pts',(0.0876208092042186,0.128523913319792,
0.861280191237196));
#13727=CARTESIAN_POINT('Ctrl Pts',(0.0876194930407674,0.128524810600568,
0.861280304871096));
#13728=CARTESIAN_POINT('Ctrl Pts',(0.0876188355799287,0.128525258810284,
0.861280361634335));
#13729=CARTESIAN_POINT('Ctrl Pts',(0.0876175218870788,0.128526154377224,
0.86128047505451));
#13730=CARTESIAN_POINT('Ctrl Pts',(0.087616865661705,0.128526601729951,
0.861280531710873));
#13731=CARTESIAN_POINT('Ctrl Pts',(0.0876155544518105,0.128527495574799,
0.861280644916258));
#13732=CARTESIAN_POINT('Ctrl Pts',(0.0876148994624468,0.12852794207025,
0.861280701465699));
#13733=CARTESIAN_POINT('Ctrl Pts',(0.0876135907205038,0.128528834203403,
0.861280814457592));
#13734=CARTESIAN_POINT('Ctrl Pts',(0.0876129369639253,0.128529279843859,
0.86128087090039));
#13735=CARTESIAN_POINT('Ctrl Pts',(0.0876116306808378,0.128530170271684,
0.861280983679579));
#13736=CARTESIAN_POINT('Ctrl Pts',(0.0876109781521583,0.128530615060559,
0.861281040016157));
#13737=CARTESIAN_POINT('Ctrl Pts',(0.0876096743280367,0.128531503783145,
0.861281152582634));
#13738=CARTESIAN_POINT('Ctrl Pts',(0.0876090230282226,0.128531947719863,
0.861281208812911));
#13739=CARTESIAN_POINT('Ctrl Pts',(0.0871812073418933,0.128823549200173,
0.861318144414142));
#13740=CARTESIAN_POINT('Ctrl Pts',(0.0867525989968188,0.129112572189949,
0.861355104045547));
#13741=CARTESIAN_POINT('Ctrl Pts',(0.0855910672287118,0.129887431733229,
0.861455150813779));
#13742=CARTESIAN_POINT('Ctrl Pts',(0.0848554614192455,0.130369192372853,
0.861518389363862));
#13743=CARTESIAN_POINT('Ctrl Pts',(0.0832204400110838,0.131420294888535,
0.861658700150327));
#13744=CARTESIAN_POINT('Ctrl Pts',(0.0823191920591894,0.13198668894343,
0.861735877643107));
#13745=CARTESIAN_POINT('Ctrl Pts',(0.0795743140512054,0.13367267244437,
0.8619704756261));
#13746=CARTESIAN_POINT('Ctrl Pts',(0.0777132127266061,0.134763164587089,
0.862128927159207));
#13747=CARTESIAN_POINT('Ctrl Pts',(0.0628779988512285,0.143046194644541,
0.863387624077439));
#13748=CARTESIAN_POINT('Ctrl Pts',(0.0489592455952193,0.148386933290451,
0.86455338930693));
#13749=CARTESIAN_POINT('Ctrl Pts',(0.0332946637113915,0.151949977996143,
0.865785739690024));
#13750=CARTESIAN_POINT('Ctrl Pts',(0.0320860979303089,0.152209766104469,
0.865880255471062));
#13751=CARTESIAN_POINT('Ctrl Pts',(0.0270405618503047,0.153231565775232,
0.866272203081998));
#13752=CARTESIAN_POINT('Ctrl Pts',(0.0231782342824295,0.153863188342659,
0.866565935525092));
#13753=CARTESIAN_POINT('Ctrl Pts',(0.0186680098006594,0.154427031980521,
0.866898735600778));
#13754=CARTESIAN_POINT('Ctrl Pts',(0.0180397194148179,0.154501687228857,
0.866944866603948));
#13755=CARTESIAN_POINT('Ctrl Pts',(0.0170884270230544,0.154608840368648,
0.86701434948501));
#13756=CARTESIAN_POINT('Ctrl Pts',(0.0167657604544999,0.154644162967363,
0.867037853957583));
#13757=CARTESIAN_POINT('Ctrl Pts',(0.0161867927283748,0.154705709706023,
0.867079912319031));
#13758=CARTESIAN_POINT('Ctrl Pts',(0.0159305361579924,0.154732307213625,
0.867098486759973));
#13759=CARTESIAN_POINT('Ctrl Pts',(0.0153742592741097,0.154788647982125,
0.867138718601952));
#13760=CARTESIAN_POINT('Ctrl Pts',(0.0150742190333812,0.154818155644297,
0.867160362633513));
#13761=CARTESIAN_POINT('Ctrl Pts',(0.0142330908995031,0.154898408543729,
0.867220887374982));
#13762=CARTESIAN_POINT('Ctrl Pts',(0.013691812799435,0.15494719142898,0.867259659977492));
#13763=CARTESIAN_POINT('Ctrl Pts',(0.0105339611448528,0.155215117043182,
0.86748489524559));
#13764=CARTESIAN_POINT('Ctrl Pts',(0.00791223073821961,0.155370832859545,
0.867668025095678));
#13765=CARTESIAN_POINT('Ctrl Pts',(-0.00938443492379959,0.155959138381236,
0.868858253106924));
#13766=CARTESIAN_POINT('Ctrl Pts',(-0.0240546187594827,0.154378764784856,
0.869789041449628));
#13767=CARTESIAN_POINT('Ctrl Pts',(-0.0401545510479763,0.150290142989394,
0.870905093455021));
#13768=CARTESIAN_POINT('Ctrl Pts',(-0.0420130401465986,0.149781237418863,
0.871035281904662));
#13769=CARTESIAN_POINT('Ctrl Pts',(-0.0476935630183817,0.148111712342661,
0.871438140633943));
#13770=CARTESIAN_POINT('Ctrl Pts',(-0.0514804665691437,0.146838387871464,
0.871713687029259));
#13771=CARTESIAN_POINT('Ctrl Pts',(-0.0560241298396049,0.145113233177457,
0.872054905275818));
#13772=CARTESIAN_POINT('Ctrl Pts',(-0.056831737219131,0.144798850679256,
0.872115968445238));
#13773=CARTESIAN_POINT('Ctrl Pts',(-0.0581639338038398,0.144267396061234,
0.872217403594079));
#13774=CARTESIAN_POINT('Ctrl Pts',(-0.0586900447208019,0.144054168273587,
0.872257646441696));
#13775=CARTESIAN_POINT('Ctrl Pts',(-0.0596406100690489,0.143662841417161,
0.872330696129825));
#13776=CARTESIAN_POINT('Ctrl Pts',(-0.0600654656211035,0.143485728226998,
0.872363469371213));
#13777=CARTESIAN_POINT('Ctrl Pts',(-0.0604930733683425,0.143305235735787,
0.87239658139186));
#13778=CARTESIAN_POINT('Ctrl Pts',(-0.0604966220396954,0.143303737692402,
0.87239685619382));
#13779=CARTESIAN_POINT('Ctrl Pts',(-0.0605035930545927,0.143300794628937,
0.872397396032431));
#13780=CARTESIAN_POINT('Ctrl Pts',(-0.0605070160446262,0.143299349346655,
0.872397661118549));
#13781=CARTESIAN_POINT('Ctrl Pts',(-0.0605137412126719,0.143296509508395,
0.872398181950845));
#13782=CARTESIAN_POINT('Ctrl Pts',(-0.0605170434629638,0.143295114931893,
0.872398437702057));
#13783=CARTESIAN_POINT('Ctrl Pts',(-0.0605235317047551,0.143292374611977,
0.872398940215497));
#13784=CARTESIAN_POINT('Ctrl Pts',(-0.0605267177710916,0.143291028846237,
0.872399186982998));
#13785=CARTESIAN_POINT('Ctrl Pts',(-0.0605329780071209,0.143288384332856,
0.872399671865314));
#13786=CARTESIAN_POINT('Ctrl Pts',(-0.0605360522575128,0.143287085559744,
0.872399909985893));
#13787=CARTESIAN_POINT('Ctrl Pts',(-0.0605420926507131,0.143284533456456,
0.872400377866405));
#13788=CARTESIAN_POINT('Ctrl Pts',(-0.0605450588802291,0.143283280097737,
0.872400607632582));
#13789=CARTESIAN_POINT('Ctrl Pts',(-0.0605508891893127,0.143280816329487,
0.872401059264462));
#13790=CARTESIAN_POINT('Ctrl Pts',(-0.0605537521743916,0.143279606389964,
0.872401281044945));
#13791=CARTESIAN_POINT('Ctrl Pts',(-0.0605593783858018,0.143277228471676,
0.872401716889391));
#13792=CARTESIAN_POINT('Ctrl Pts',(-0.0605621416162174,0.143276060498106,
0.872401930953278));
#13793=CARTESIAN_POINT('Ctrl Pts',(-0.0605675720198831,0.143273764967636,
0.872402351650126));
#13794=CARTESIAN_POINT('Ctrl Pts',(-0.0605702391954167,0.143272637416204,
0.872402558282899));
#13795=CARTESIAN_POINT('Ctrl Pts',(-0.0610598249756475,0.143065648366848,
0.872440488634159));
#13796=CARTESIAN_POINT('Ctrl Pts',(-0.0615456853657312,0.142857308419279,
0.872478296295375));
#13797=CARTESIAN_POINT('Ctrl Pts',(-0.0625846159187864,0.142405524813775,
0.872559502527816));
#13798=CARTESIAN_POINT('Ctrl Pts',(-0.0631373441878761,0.142161328743564,
0.872602926138957));
#13799=CARTESIAN_POINT('Ctrl Pts',(-0.0636886258347646,0.141913922640731,
0.87264646002013));
#13800=CARTESIAN_POINT('Origin',(0.,0.,-0.129405622560373));
#13801=CARTESIAN_POINT('',(-0.0636886228436576,0.14191392398309,0.956529730343417));
#13802=CARTESIAN_POINT('',(-0.0636886279045103,0.141913921711863,0.942835077379979));
#13803=CARTESIAN_POINT('',(-0.0636886258329924,0.141913922641526,-0.129405622560373));
#13804=CARTESIAN_POINT('Ctrl Pts',(-0.0636886228436577,0.14191392398309,
0.956529730343417));
#13805=CARTESIAN_POINT('Ctrl Pts',(-0.0605616421227201,0.143317261232781,
0.95626580888382));
#13806=CARTESIAN_POINT('Ctrl Pts',(-0.0573883432362314,0.144617218288781,
0.956003754733755));
#13807=CARTESIAN_POINT('Ctrl Pts',(-0.0516595524775657,0.146745655762337,
0.955543579904026));
#13808=CARTESIAN_POINT('Ctrl Pts',(-0.0491212969258761,0.147614692335739,
0.955344073949756));
#13809=CARTESIAN_POINT('Ctrl Pts',(-0.0460398608689767,0.148581401105557,
0.955108111206096));
#13810=CARTESIAN_POINT('Ctrl Pts',(-0.0455172163110459,0.148742342951681,
0.95506830310435));
#13811=CARTESIAN_POINT('Ctrl Pts',(-0.0447043650646508,0.148987964673378,
0.955006733736637));
#13812=CARTESIAN_POINT('Ctrl Pts',(-0.0444147490985092,0.149074558326085,
0.954984864139642));
#13813=CARTESIAN_POINT('Ctrl Pts',(-0.0438778053492266,0.149233398022506,
0.954944445212162));
#13814=CARTESIAN_POINT('Ctrl Pts',(-0.0436305527662352,0.149305873142629,
0.954925883076122));
#13815=CARTESIAN_POINT('Ctrl Pts',(-0.0430721755460429,0.149468040169477,
0.954884075616488));
#13816=CARTESIAN_POINT('Ctrl Pts',(-0.0427609509344645,0.149557375006153,
0.954860851219839));
#13817=CARTESIAN_POINT('Ctrl Pts',(-0.0418446251520368,0.149817305706711,
0.954792695463313));
#13818=CARTESIAN_POINT('Ctrl Pts',(-0.0412387561642388,0.149985208501964,
0.954747916666911));
#13819=CARTESIAN_POINT('Ctrl Pts',(-0.0369572440978493,0.151143826569018,
0.954433376674147));
#13820=CARTESIAN_POINT('Ctrl Pts',(-0.0332469560861469,0.152003092786986,
0.954170649527741));
#13821=CARTESIAN_POINT('Ctrl Pts',(-0.028501874617075,0.152919903096122,
0.953842670361788));
#13822=CARTESIAN_POINT('Ctrl Pts',(-0.027493332379588,0.153104442705289,
0.953773415504164));
#13823=CARTESIAN_POINT('Ctrl Pts',(-0.0116456296118653,0.155842554439753,
0.95269128757154));
#13824=CARTESIAN_POINT('Ctrl Pts',(0.00348505447402093,0.156238328516161,
0.951733510985633));
#13825=CARTESIAN_POINT('Ctrl Pts',(0.0206331190770367,0.154191331757608,
0.950551500627717));
#13826=CARTESIAN_POINT('Ctrl Pts',(0.0228229056783667,0.153882443979089,
0.950398919571636));
#13827=CARTESIAN_POINT('Ctrl Pts',(0.0260749588618998,0.153352774974058,
0.950169449389325));
#13828=CARTESIAN_POINT('Ctrl Pts',(0.0271427664052125,0.153167382954111,
0.950093639526612));
#13829=CARTESIAN_POINT('Ctrl Pts',(0.0290814589951995,0.152809879150505,
0.949955105425714));
#13830=CARTESIAN_POINT('Ctrl Pts',(0.029952981008281,0.152641440289458,
0.949892497992219));
#13831=CARTESIAN_POINT('Ctrl Pts',(0.0313338949610883,0.152362269641473,
0.949792750707262));
#13832=CARTESIAN_POINT('Ctrl Pts',(0.0318442640754913,0.152256418640378,
0.949755766364858));
#13833=CARTESIAN_POINT('Ctrl Pts',(0.0323552245392878,0.152147763527324,
0.949718617420224));
#13834=CARTESIAN_POINT('Ctrl Pts',(0.0323563631412977,0.152147521391651,
0.94971853463853));
#13835=CARTESIAN_POINT('Ctrl Pts',(0.0323586466220602,0.152147035758696,
0.949718368617576));
#13836=CARTESIAN_POINT('Ctrl Pts',(0.0323597914947508,0.152146792262557,
0.949718285378751));
#13837=CARTESIAN_POINT('Ctrl Pts',(0.0323620875712343,0.152146303896665,
0.949718118439563));
#13838=CARTESIAN_POINT('Ctrl Pts',(0.0323632387665168,0.152146059028573,
0.949718034739813));
#13839=CARTESIAN_POINT('Ctrl Pts',(0.0323655475365981,0.152145567908027,
0.949717866875234));
#13840=CARTESIAN_POINT('Ctrl Pts',(0.0323667051044633,0.152145321656897,
0.949717782710902));
#13841=CARTESIAN_POINT('Ctrl Pts',(0.0323690266744545,0.152144827758173,
0.949717613913161));
#13842=CARTESIAN_POINT('Ctrl Pts',(0.0323701906679437,0.152144580112262,
0.949717529280371));
#13843=CARTESIAN_POINT('Ctrl Pts',(0.0323725251373474,0.152144083413267,
0.94971735954219));
#13844=CARTESIAN_POINT('Ctrl Pts',(0.032373695607215,0.152143834361314,
0.949717274437232));
#13845=CARTESIAN_POINT('Ctrl Pts',(0.0323760430834124,0.152143334838265,
0.949717103750761));
#13846=CARTESIAN_POINT('Ctrl Pts',(0.0323772200821449,0.152143084368629,
0.949717018169795));
#13847=CARTESIAN_POINT('Ctrl Pts',(0.032379580671995,0.15214258199784,0.949716846527222));
#13848=CARTESIAN_POINT('Ctrl Pts',(0.0323807642534029,0.152142330098593,
0.949716760466315));
#13849=CARTESIAN_POINT('Ctrl Pts',(0.0323831379893035,0.152141824872209,
0.94971658786524));
#13850=CARTESIAN_POINT('Ctrl Pts',(0.0323843281337768,0.152141571547047,
0.949716501325796));
#13851=CARTESIAN_POINT('Ctrl Pts',(0.032835900190565,0.152045447789354,
0.949683665736758));
#13852=CARTESIAN_POINT('Ctrl Pts',(0.0332858494498373,0.151947578963342,
0.949650853196147));
#13853=CARTESIAN_POINT('Ctrl Pts',(0.0342900624437464,0.151724477285312,
0.949577405257927));
#13854=CARTESIAN_POINT('Ctrl Pts',(0.0348440854145153,0.15159820277853,
0.949536736920863));
#13855=CARTESIAN_POINT('Ctrl Pts',(0.0362427354886735,0.151271346418091,
0.949433689187789));
#13856=CARTESIAN_POINT('Ctrl Pts',(0.0370863887693582,0.151066726429398,
0.949371181116677));
#13857=CARTESIAN_POINT('Ctrl Pts',(0.0418202506969962,0.149876529749583,
0.949018419431836));
#13858=CARTESIAN_POINT('Ctrl Pts',(0.0456725421758692,0.148747843499238,
0.948723599568112));
#13859=CARTESIAN_POINT('Ctrl Pts',(0.0512867919273554,0.14686426783951,
0.948281889444133));
#13860=CARTESIAN_POINT('Ctrl Pts',(0.0530855958110184,0.146223688864191,
0.948138504818793));
#13861=CARTESIAN_POINT('Ctrl Pts',(0.0686437175628241,0.140358312249086,
0.946882244898241));
#13862=CARTESIAN_POINT('Ctrl Pts',(0.0816067039213671,0.133239197660704,
0.945715106069722));
#13863=CARTESIAN_POINT('Ctrl Pts',(0.0954507241606839,0.122848255642365,
0.944412915170613));
#13864=CARTESIAN_POINT('Ctrl Pts',(0.0974867403277383,0.121238905752293,
0.944220062472617));
#13865=CARTESIAN_POINT('Ctrl Pts',(0.0998963733384406,0.11923425711897,
0.94399108415196));
#13866=CARTESIAN_POINT('Ctrl Pts',(0.100309266152085,0.118887108738101,
0.943951821827424));
#13867=CARTESIAN_POINT('Ctrl Pts',(0.100949475516749,0.118343129465159,
0.943890913112717));
#13868=CARTESIAN_POINT('Ctrl Pts',(0.10117803588526,0.118147780162392,0.943869162023602));
#13869=CARTESIAN_POINT('Ctrl Pts',(0.101601523124038,0.11778369778257,0.943828851465));
#13870=CARTESIAN_POINT('Ctrl Pts',(0.101796594989769,0.117615144495934,
0.943810279769402));
#13871=CARTESIAN_POINT('Ctrl Pts',(0.102237341433666,0.117232396321224,
0.943768310169039));
#13872=CARTESIAN_POINT('Ctrl Pts',(0.102482761931622,0.11701791419601,0.943744933900112));
#13873=CARTESIAN_POINT('Ctrl Pts',(0.103223036059529,0.116366845823294,
0.943674396979351));
#13874=CARTESIAN_POINT('Ctrl Pts',(0.103715796035067,0.115927872724899,
0.943627409198699));
#13875=CARTESIAN_POINT('Ctrl Pts',(0.107484211303136,0.112527535302619,
0.94326765534566));
#13876=CARTESIAN_POINT('Ctrl Pts',(0.110635599865423,0.109430685989414,
0.942964381326475));
#13877=CARTESIAN_POINT('Ctrl Pts',(0.1237422794111,0.0954048800150995,0.941668841431201));
#13878=CARTESIAN_POINT('Ctrl Pts',(0.132242906875762,0.0832232246797103,
0.940729093471332));
#13879=CARTESIAN_POINT('Ctrl Pts',(0.140665790789191,0.0665159729279089,
0.939454608411167));
#13880=CARTESIAN_POINT('Ctrl Pts',(0.142300806178678,0.062942159239021,
0.939183276244309));
#13881=CARTESIAN_POINT('Ctrl Pts',(0.144146801727768,0.0584665337771078,
0.938843120661047));
#13882=CARTESIAN_POINT('Ctrl Pts',(0.144487470350992,0.0576195007644558,
0.938778732039682));
#13883=CARTESIAN_POINT('Ctrl Pts',(0.145013331761929,0.056278013709661,
0.938676714027132));
#13884=CARTESIAN_POINT('Ctrl Pts',(0.145203501328331,0.0557855214665347,
0.938639251786081));
#13885=CARTESIAN_POINT('Ctrl Pts',(0.145554838070132,0.0548616774134873,
0.938568956608212));
#13886=CARTESIAN_POINT('Ctrl Pts',(0.145716604577305,0.0544305582952572,
0.938536144114774));
#13887=CARTESIAN_POINT('Ctrl Pts',(0.146073710701386,0.0534658435094093,
0.938462696836499));
#13888=CARTESIAN_POINT('Ctrl Pts',(0.146268044641094,0.0529318852986887,
0.93842202911494));
#13889=CARTESIAN_POINT('Ctrl Pts',(0.146751860597336,0.0515795258457461,
0.938318983980847));
#13890=CARTESIAN_POINT('Ctrl Pts',(0.147037422034294,0.0507597531511795,
0.938256477904554));
#13891=CARTESIAN_POINT('Ctrl Pts',(0.148604337422754,0.0461373515406115,
0.937903747445434));
#13892=CARTESIAN_POINT('Ctrl Pts',(0.149744918301528,0.0422889851955426,
0.937608957759007));
#13893=CARTESIAN_POINT('Ctrl Pts',(0.15120684129218,0.0365505228376165,
0.93716725216043));
#13894=CARTESIAN_POINT('Ctrl Pts',(0.151644164357749,0.0346914465339953,
0.93702384068137));
#13895=CARTESIAN_POINT('Ctrl Pts',(0.155152896367734,0.0184387429981322,
0.935767572922593));
#13896=CARTESIAN_POINT('Ctrl Pts',(0.156200950457405,0.00368696476256723,
0.93460045507406));
#13897=CARTESIAN_POINT('Ctrl Pts',(0.154977838413255,-0.0135796118118842,
0.933298255529385));
#13898=CARTESIAN_POINT('Ctrl Pts',(0.154729720408327,-0.0161632926673331,
0.933105379469176));
#13899=CARTESIAN_POINT('Ctrl Pts',(0.154352057576583,-0.0192752644350223,
0.932876377157122));
#13900=CARTESIAN_POINT('Ctrl Pts',(0.154284282256396,-0.0198104459562377,
0.932837113451182));
#13901=CARTESIAN_POINT('Ctrl Pts',(0.154174396726348,-0.0206433595920402,
0.932776203063593));
#13902=CARTESIAN_POINT('Ctrl Pts',(0.154134206010954,-0.0209413333562646,
0.932754451673873));
#13903=CARTESIAN_POINT('Ctrl Pts',(0.154057949533934,-0.0214945841933946,
0.932714140842873));
#13904=CARTESIAN_POINT('Ctrl Pts',(0.154022113485362,-0.0217498855996991,
0.932695569174006));
#13905=CARTESIAN_POINT('Ctrl Pts',(0.153939534570932,-0.0223277500680519,
0.932653599996227));
#13906=CARTESIAN_POINT('Ctrl Pts',(0.153892412619383,-0.0226502554175331,
0.932630224121317));
#13907=CARTESIAN_POINT('Ctrl Pts',(0.153746821260097,-0.0236252597032322,
0.932559689564563));
#13908=CARTESIAN_POINT('Ctrl Pts',(0.153645211395646,-0.0242772939247841,
0.932512703736852));
#13909=CARTESIAN_POINT('Ctrl Pts',(0.15283190250593,-0.029286585055981,
0.932153010964684));
#13910=CARTESIAN_POINT('Ctrl Pts',(0.15193905196086,-0.0336129154550012,
0.931849792433107));
#13911=CARTESIAN_POINT('Ctrl Pts',(0.147262842354895,-0.052228877496125,
0.930554396683378));
#13912=CARTESIAN_POINT('Ctrl Pts',(0.141638449781161,-0.0659757428550496,
0.929614738110709));
#13913=CARTESIAN_POINT('Ctrl Pts',(0.13216892268605,-0.0821135268963821,
0.928340232676168));
#13914=CARTESIAN_POINT('Ctrl Pts',(0.130051807652998,-0.0854270345897545,
0.928068762459612));
#13915=CARTESIAN_POINT('Ctrl Pts',(0.127291190612526,-0.089406873773799,
0.927728453812722));
#13916=CARTESIAN_POINT('Ctrl Pts',(0.126764167278465,-0.0901525491389225,
0.92766405505106));
#13917=CARTESIAN_POINT('Ctrl Pts',(0.125922108611989,-0.0913219788017271,
0.927562024593833));
#13918=CARTESIAN_POINT('Ctrl Pts',(0.125611422188316,-0.0917488520521021,
0.927524560117915));
#13919=CARTESIAN_POINT('Ctrl Pts',(0.125025712463918,-0.0925450471626755,
0.927454262935369));
#13920=CARTESIAN_POINT('Ctrl Pts',(0.124751209957878,-0.0929147466074473,
0.927421450683122));
#13921=CARTESIAN_POINT('Ctrl Pts',(0.12413433430201,-0.0937378919021104,
0.927348006781666));
#13922=CARTESIAN_POINT('Ctrl Pts',(0.123791111546934,-0.0941906896513171,
0.927307342209724));
#13923=CARTESIAN_POINT('Ctrl Pts',(0.122917333295667,-0.0953303991769037,
0.927204310374685));
#13924=CARTESIAN_POINT('Ctrl Pts',(0.122383500943652,-0.0960147617387886,
0.927141814505881));
#13925=CARTESIAN_POINT('Ctrl Pts',(0.119350839044903,-0.0998361908755614,
0.926789243787177));
#13926=CARTESIAN_POINT('Ctrl Pts',(0.116737363938768,-0.102879882271182,
0.926494608473505));
#13927=CARTESIAN_POINT('Ctrl Pts',(0.112709002933879,-0.107220041460402,
0.926052926001055));
#13928=CARTESIAN_POINT('Ctrl Pts',(0.111382909454409,-0.108596977794657,
0.925909377126475));
#13929=CARTESIAN_POINT('Ctrl Pts',(0.0996297614469436,-0.120358971129495,
0.92465306908851));
#13930=CARTESIAN_POINT('Ctrl Pts',(0.0878048483710721,-0.129238546997106,
0.923486058390957));
#13931=CARTESIAN_POINT('Ctrl Pts',(0.0726341946255662,-0.137574773123402,
0.922183814643931));
#13932=CARTESIAN_POINT('Ctrl Pts',(0.0703274574803643,-0.138768135060366,
0.921990819221544));
#13933=CARTESIAN_POINT('Ctrl Pts',(0.0675064796765401,-0.140139105186311,
0.921761694337139));
#13934=CARTESIAN_POINT('Ctrl Pts',(0.0670199806256607,-0.140372418305302,
0.921722423576472));
#13935=CARTESIAN_POINT('Ctrl Pts',(0.0662604721912255,-0.140731811395884,
0.921661504645653));
#13936=CARTESIAN_POINT('Ctrl Pts',(0.0659883010491051,-0.140859635959385,
0.921639751720815));
#13937=CARTESIAN_POINT('Ctrl Pts',(0.065482090202286,-0.141095587549365,
0.921599439498538));
#13938=CARTESIAN_POINT('Ctrl Pts',(0.0652481546746922,-0.141203920896554,
0.921580867965983));
#13939=CARTESIAN_POINT('Ctrl Pts',(0.0647178797071554,-0.141447887063497,
0.921538900945333));
#13940=CARTESIAN_POINT('Ctrl Pts',(0.0644213832595874,-0.141583170231193,
0.92151552708186));
#13941=CARTESIAN_POINT('Ctrl Pts',(0.0635233883146044,-0.141989495716967,
0.921445004592581));
#13942=CARTESIAN_POINT('Ctrl Pts',(0.0629205779461682,-0.142257648895638,
0.921398028733891));
#13943=CARTESIAN_POINT('Ctrl Pts',(0.05827477706551,-0.144288971096523,
0.921038647351752));
#13944=CARTESIAN_POINT('Ctrl Pts',(0.054159676708548,-0.145883499154976,
0.920735711694544));
#13945=CARTESIAN_POINT('Ctrl Pts',(0.035994210136798,-0.152047367186302,
0.919441048389864));
#13946=CARTESIAN_POINT('Ctrl Pts',(0.0214018054862157,-0.154777248216127,
0.918501843308454));
#13947=CARTESIAN_POINT('Ctrl Pts',(0.00270480659069758,-0.155576416194499,
0.917227233169775));
#13948=CARTESIAN_POINT('Ctrl Pts',(-0.00123766647162131,-0.155594989931657,
0.916955061156382));
#13949=CARTESIAN_POINT('Ctrl Pts',(-0.00608967229243966,-0.155433437599074,
0.916613974435584));
#13950=CARTESIAN_POINT('Ctrl Pts',(-0.00700271842718297,-0.155394979016254,
0.91654952421732));
#13951=CARTESIAN_POINT('Ctrl Pts',(-0.00844280089516923,-0.155321603564634,
0.916447430610745));
#13952=CARTESIAN_POINT('Ctrl Pts',(-0.00897009996397641,-0.155292043308623,
0.916409954795012));
#13953=CARTESIAN_POINT('Ctrl Pts',(-0.00995682681477347,-0.155231685287383,
0.916339647433335));
#13954=CARTESIAN_POINT('Ctrl Pts',(-0.0104162895345085,-0.155201531633367,
0.916306836397572));
#13955=CARTESIAN_POINT('Ctrl Pts',(-0.011442179105327,-0.155129628433983,
0.91623340959511));
#13956=CARTESIAN_POINT('Ctrl Pts',(-0.0120085223198687,-0.155086815869748,
0.916192760976546));
#13957=CARTESIAN_POINT('Ctrl Pts',(-0.013439009589307,-0.154970796024108,
0.916089796497695));
#13958=CARTESIAN_POINT('Ctrl Pts',(-0.0143027896319657,-0.154893462583821,
0.916027352325525));
#13959=CARTESIAN_POINT('Ctrl Pts',(-0.0191470381299152,-0.154418895567225,
0.915675589544445));
#13960=CARTESIAN_POINT('Ctrl Pts',(-0.02311131681086,-0.153875488563329,
0.9153817349092));
#13961=CARTESIAN_POINT('Ctrl Pts',(-0.0289415957922071,-0.152845924076965,
0.914940168790301));
#13962=CARTESIAN_POINT('Ctrl Pts',(-0.0308268360618294,-0.152476877315448,
0.914795924471245));
#13963=CARTESIAN_POINT('Ctrl Pts',(-0.0470858212228406,-0.148980234222072,
0.913539408146966));
#13964=CARTESIAN_POINT('Ctrl Pts',(-0.0609533191626043,-0.143863823529639,
0.912372934983359));
#13965=CARTESIAN_POINT('Ctrl Pts',(-0.0761868591312057,-0.135639773197008,
0.911070468307069));
#13966=CARTESIAN_POINT('Ctrl Pts',(-0.0784473977661218,-0.134345053999845,
0.910876872969576));
#13967=CARTESIAN_POINT('Ctrl Pts',(-0.0811362380198341,-0.132713997002593,
0.910647132148336));
#13968=CARTESIAN_POINT('Ctrl Pts',(-0.0815964977205298,-0.132431513256563,
0.910607826009885));
#13969=CARTESIAN_POINT('Ctrl Pts',(-0.0823108237584191,-0.131987958803547,
0.910546864238203));
#13970=CARTESIAN_POINT('Ctrl Pts',(-0.0825659036352816,-0.131828542197799,
0.910525103616403));
#13971=CARTESIAN_POINT('Ctrl Pts',(-0.0830387372779375,-0.13153112585634,
0.910484784413295));
#13972=CARTESIAN_POINT('Ctrl Pts',(-0.0832566082599744,-0.131393326088713,
0.910466213559127));
#13973=CARTESIAN_POINT('Ctrl Pts',(-0.0837490165790518,-0.131080169507045,
0.910424257331071));
#13974=CARTESIAN_POINT('Ctrl Pts',(-0.0840233457276077,-0.130904491878477,
0.910400893534863));
#13975=CARTESIAN_POINT('Ctrl Pts',(-0.0848509908067295,-0.130370802645779,
0.910330431426925));
#13976=CARTESIAN_POINT('Ctrl Pts',(-0.0854025950839007,-0.130010128904104,
0.910283505447237));
#13977=CARTESIAN_POINT('Ctrl Pts',(-0.0896104064106475,-0.127220459128954,
0.909925672045913));
#13978=CARTESIAN_POINT('Ctrl Pts',(-0.0931650377193367,-0.124640903690957,
0.909624142582147));
#13979=CARTESIAN_POINT('Ctrl Pts',(-0.108155378818288,-0.112762384688307,
0.908333062392606));
#13980=CARTESIAN_POINT('Ctrl Pts',(-0.11834572893592,-0.102016072679374,
0.907396058604052));
#13981=CARTESIAN_POINT('Ctrl Pts',(-0.129182080549085,-0.0867394478478589,
0.906120907876402));
#13982=CARTESIAN_POINT('Ctrl Pts',(-0.131365529719357,-0.083395651189083,
0.905845294811318));
#13983=CARTESIAN_POINT('Ctrl Pts',(-0.133889486022727,-0.0791849084518531,
0.905500394190824));
#13984=CARTESIAN_POINT('Ctrl Pts',(-0.134354182049451,-0.0783938638885485,
0.90543569390499));
#13985=CARTESIAN_POINT('Ctrl Pts',(-0.135075704019467,-0.0771403684027894,
0.905333293424861));
#13986=CARTESIAN_POINT('Ctrl Pts',(-0.135337220731513,-0.0766806294038661,
0.90529576252288));
#13987=CARTESIAN_POINT('Ctrl Pts',(-0.135821971898118,-0.0758182458312662,
0.905225405541033));
#13988=CARTESIAN_POINT('Ctrl Pts',(-0.136045774026821,-0.0754159254554385,
0.905192600241969));
#13989=CARTESIAN_POINT('Ctrl Pts',(-0.136541167955571,-0.0745159937917177,
0.905119255675079));
#13990=CARTESIAN_POINT('Ctrl Pts',(-0.136811830904436,-0.0740178815306377,
0.905078683896796));
#13991=CARTESIAN_POINT('Ctrl Pts',(-0.137488031273642,-0.0727570610716043,
0.904976043704369));
#13992=CARTESIAN_POINT('Ctrl Pts',(-0.13788994484764,-0.0719924421952539,
0.904913848388818));
#13993=CARTESIAN_POINT('Ctrl Pts',(-0.140094706927866,-0.0677118025913985,
0.904565890159978));
#13994=CARTESIAN_POINT('Ctrl Pts',(-0.14176928475754,-0.0641317376980251,
0.904275705197761));
#13995=CARTESIAN_POINT('Ctrl Pts',(-0.144252364957401,-0.0582493262404351,
0.903799684121174));
#13996=CARTESIAN_POINT('Ctrl Pts',(-0.145146257010626,-0.0559847461395491,
0.903616622534871));
#13997=CARTESIAN_POINT('Ctrl Pts',(-0.151003890944027,-0.0400604906779335,
0.902331084345073));
#13998=CARTESIAN_POINT('Ctrl Pts',(-0.154084384812384,-0.0257868058292971,
0.901178461611881));
#13999=CARTESIAN_POINT('Ctrl Pts',(-0.155310168662362,-0.008948893428367,
0.899911655934367));
#14000=CARTESIAN_POINT('Ctrl Pts',(-0.155427707712362,-0.00660003721258554,
0.899737223210819));
#14001=CARTESIAN_POINT('Ctrl Pts',(-0.155506255650117,-0.00372575001372523,
0.899527253607195));
#14002=CARTESIAN_POINT('Ctrl Pts',(-0.155517918253579,-0.00320216845602306,
0.899489146753876));
#14003=CARTESIAN_POINT('Ctrl Pts',(-0.155532054575551,-0.00238135235045557,
0.899429638536462));
#14004=CARTESIAN_POINT('Ctrl Pts',(-0.155536320914119,-0.00208415931666893,
0.899408139988824));
#14005=CARTESIAN_POINT('Ctrl Pts',(-0.155542701881444,-0.00152874781286528,
0.899368053463317));
#14006=CARTESIAN_POINT('Ctrl Pts',(-0.155545025346779,-0.00127053923554435,
0.899349454507506));
#14007=CARTESIAN_POINT('Ctrl Pts',(-0.155548858987973,-0.000681486019007851,
0.899307107999714));
#14008=CARTESIAN_POINT('Ctrl Pts',(-0.155549956642077,-0.000350642004559851,
0.899283383702997));
#14009=CARTESIAN_POINT('Ctrl Pts',(-0.155550085855824,0.00066483591721158,
0.899210741903766));
#14010=CARTESIAN_POINT('Ctrl Pts',(-0.155545653043982,0.00134947466596592,
0.899162012788569));
#14011=CARTESIAN_POINT('Ctrl Pts',(-0.155524923765982,0.00293454784667604,
0.899049718708714));
#14012=CARTESIAN_POINT('Ctrl Pts',(-0.155505327669386,0.00383492449214596,
0.898986322870997));
#14013=CARTESIAN_POINT('Ctrl Pts',(-0.155191940176796,0.0141250482928698,
0.898265738327592));
#14014=CARTESIAN_POINT('Ctrl Pts',(-0.154055860259594,0.0234712885827232,
0.897648125621407));
#14015=CARTESIAN_POINT('Ctrl Pts',(-0.149678020877209,0.0438575256198832,
0.896275750927973));
#14016=CARTESIAN_POINT('Ctrl Pts',(-0.1460441175715,0.0547545526085629,
0.895522902063312));
#14017=CARTESIAN_POINT('Ctrl Pts',(-0.14051488865648,0.066741497240731,
0.894605550974665));
#14018=CARTESIAN_POINT('Ctrl Pts',(-0.13975561378378,0.0683171235622771,
0.894483158627786));
#14019=CARTESIAN_POINT('Ctrl Pts',(-0.138653280561385,0.0705093412341997,
0.894310148075968));
#14020=CARTESIAN_POINT('Ctrl Pts',(-0.138332328586955,0.0711369541796008,
0.894260299051709));
#14021=CARTESIAN_POINT('Ctrl Pts',(-0.137806804231475,0.07214759696694,
0.894179502113146));
#14022=CARTESIAN_POINT('Ctrl Pts',(-0.137604871688499,0.0725319951553056,
0.894148647228026));
#14023=CARTESIAN_POINT('Ctrl Pts',(-0.137181139545749,0.0733304718904287,
0.894084294067337));
#14024=CARTESIAN_POINT('Ctrl Pts',(-0.136959068744773,0.0737444006986513,
0.894050786450422));
#14025=CARTESIAN_POINT('Ctrl Pts',(-0.13643058577915,0.0747188452038213,
0.893971553365648));
#14026=CARTESIAN_POINT('Ctrl Pts',(-0.136122590990758,0.0752784880563611,
0.893925771983588));
#14027=CARTESIAN_POINT('Ctrl Pts',(-0.135093488069912,0.0771214554592928,
0.893774081035787));
#14028=CARTESIAN_POINT('Ctrl Pts',(-0.134357629866733,0.0783964057253749,
0.893667645576543));
#14029=CARTESIAN_POINT('Ctrl Pts',(-0.130391362333879,0.0850484761478511,
0.89310419930309));
#14030=CARTESIAN_POINT('Ctrl Pts',(-0.126856409538407,0.0902362580492424,
0.892636177407088));
#14031=CARTESIAN_POINT('Ctrl Pts',(-0.117609748200653,0.102185401155856,
0.891486857489979));
#14032=CARTESIAN_POINT('Ctrl Pts',(-0.111615500045129,0.108700817805921,
0.890798062324915));
#14033=CARTESIAN_POINT('Ctrl Pts',(-0.0999139986189095,0.119425730706921,
0.889570868028963));
#14034=CARTESIAN_POINT('Ctrl Pts',(-0.0944094498375184,0.123823243297438,
0.889032161706746));
#14035=CARTESIAN_POINT('Ctrl Pts',(-0.0880468611393628,0.128234348516339,
0.888464555949552));
#14036=CARTESIAN_POINT('Ctrl Pts',(-0.0874657018089413,0.128631446207753,
0.88841319069226));
#14037=CARTESIAN_POINT('Ctrl Pts',(-0.0866043173201996,0.129211480423492,
0.888337785972354));
#14038=CARTESIAN_POINT('Ctrl Pts',(-0.086326176412109,0.129397471859048,
0.888313548788249));
#14039=CARTESIAN_POINT('Ctrl Pts',(-0.0858320072469462,0.12972561776396,
0.888270686291535));
#14040=CARTESIAN_POINT('Ctrl Pts',(-0.0856162228560454,0.129868132196046,
0.888252037078596));
#14041=CARTESIAN_POINT('Ctrl Pts',(-0.0851536755377225,0.130171966852737,
0.888212205495706));
#14042=CARTESIAN_POINT('Ctrl Pts',(-0.0849068096903753,0.130333123510633,
0.888191034051918));
#14043=CARTESIAN_POINT('Ctrl Pts',(-0.0842293227602283,0.130772652371244,
0.888133165738373));
#14044=CARTESIAN_POINT('Ctrl Pts',(-0.0837977757505891,0.131049602135839,
0.888096562143742));
#14045=CARTESIAN_POINT('Ctrl Pts',(-0.0815096338915462,0.132502116651127,
0.88790379493374));
#14046=CARTESIAN_POINT('Ctrl Pts',(-0.0796295319257737,0.133640451638179,
0.887749946698035));
#14047=CARTESIAN_POINT('Ctrl Pts',(-0.0731663819296115,0.137368807356439,
0.887234032347461));
#14048=CARTESIAN_POINT('Ctrl Pts',(-0.0684810578985275,0.139763159764089,
0.886881593895257));
#14049=CARTESIAN_POINT('Ctrl Pts',(-0.0636885883104107,0.141913939481036,
0.886533246392299));
#14050=CARTESIAN_POINT('',(-0.155549945051201,-0.000130746198511629,0.885519163677599));
#14051=CARTESIAN_POINT('Ctrl Pts',(-0.0636886258347646,0.141913922640731,
0.87264646002013));
#14052=CARTESIAN_POINT('Ctrl Pts',(-0.0639839808243548,0.14178137219698,
0.872669783758718));
#14053=CARTESIAN_POINT('Ctrl Pts',(-0.0642789205766795,0.141647900346939,
0.87269313914274));
#14054=CARTESIAN_POINT('Ctrl Pts',(-0.0656103611131948,0.141040356252537,
0.872798865345358));
#14055=CARTESIAN_POINT('Ctrl Pts',(-0.0666420232472574,0.140555832985705,
0.872881593105514));
#14056=CARTESIAN_POINT('Ctrl Pts',(-0.0698040541603743,0.139028137482075,
0.873137691865879));
#14057=CARTESIAN_POINT('Ctrl Pts',(-0.0719158695679871,0.137947582673369,
0.873312326119224));
#14058=CARTESIAN_POINT('Ctrl Pts',(-0.0800256953822378,0.133561183197557,
0.873997314592906));
#14059=CARTESIAN_POINT('Ctrl Pts',(-0.0858268567636554,0.129909317770408,
0.874518923921789));
#14060=CARTESIAN_POINT('Ctrl Pts',(-0.101196557961316,0.118754146378466,
0.875984139080918));
#14061=CARTESIAN_POINT('Ctrl Pts',(-0.110156432495108,0.110493846410477,
0.876939696515992));
#14062=CARTESIAN_POINT('Ctrl Pts',(-0.118736569029378,0.100491270105243,
0.877911926478186));
#14063=CARTESIAN_POINT('Ctrl Pts',(-0.119400897564014,0.0997010230989174,
0.877987607296685));
#14064=CARTESIAN_POINT('Ctrl Pts',(-0.120313412303396,0.098593344214222,
0.878092062446794));
#14065=CARTESIAN_POINT('Ctrl Pts',(-0.120568287415644,0.098281497663267,
0.878121293353105));
#14066=CARTESIAN_POINT('Ctrl Pts',(-0.120975316662894,0.0977795201094749,
0.878168059052301));
#14067=CARTESIAN_POINT('Ctrl Pts',(-0.121128238137576,0.0975900185595753,
0.87818564837152));
#14068=CARTESIAN_POINT('Ctrl Pts',(-0.121446543938576,0.0971936705813331,
0.878222299705275));
#14069=CARTESIAN_POINT('Ctrl Pts',(-0.121611845556675,0.0969867602178439,
0.878241355464605));
#14070=CARTESIAN_POINT('Ctrl Pts',(-0.122009978867162,0.0964857929167504,
0.878287307996225));
#14071=CARTESIAN_POINT('Ctrl Pts',(-0.122242279153235,0.0961913113192382,
0.878314166957051));
#14072=CARTESIAN_POINT('Ctrl Pts',(-0.123048706878283,0.0951613825374254,
0.878407583331032));
#14073=CARTESIAN_POINT('Ctrl Pts',(-0.123617296309055,0.0944215926465238,
0.878473761932663));
#14074=CARTESIAN_POINT('Ctrl Pts',(-0.126620195467169,0.0904409056087231,
0.878825239610829));
#14075=CARTESIAN_POINT('Ctrl Pts',(-0.128934029129705,0.0871105864426254,
0.879103107677789));
#14076=CARTESIAN_POINT('Ctrl Pts',(-0.136585451272144,0.075123745866676,
0.880062527809272));
#14077=CARTESIAN_POINT('Ctrl Pts',(-0.1412025418034,0.0660380972084901,
0.880720022333444));
#14078=CARTESIAN_POINT('Ctrl Pts',(-0.145990188285565,0.0537740880269545,
0.88159360466118));
#14079=CARTESIAN_POINT('Ctrl Pts',(-0.146999267897609,0.0509509727517754,
0.88179367257103));
#14080=CARTESIAN_POINT('Ctrl Pts',(-0.148330356843338,0.0468574069364056,
0.882083811666845));
#14081=CARTESIAN_POINT('Ctrl Pts',(-0.148718894265833,0.0456092282163969,
0.882172281006354));
#14082=CARTESIAN_POINT('Ctrl Pts',(-0.15025511847033,0.040445631031379,
0.88253858622068));
#14083=CARTESIAN_POINT('Ctrl Pts',(-0.151264177651802,0.0364910025913579,
0.882819927379395));
#14084=CARTESIAN_POINT('Ctrl Pts',(-0.152298897269656,0.0316482199489744,
0.88316756658446));
#14085=CARTESIAN_POINT('Ctrl Pts',(-0.152474036970631,0.0307933747767094,
0.883229045223125));
#14086=CARTESIAN_POINT('Ctrl Pts',(-0.152751582879789,0.0293782366564353,
0.883331027541352));
#14087=CARTESIAN_POINT('Ctrl Pts',(-0.152858122392891,0.0288187658339247,
0.883371399611584));
#14088=CARTESIAN_POINT('Ctrl Pts',(-0.153045231729836,0.0278059622976841,
0.883444587415596));
#14089=CARTESIAN_POINT('Ctrl Pts',(-0.153126866151747,0.0273528307260728,
0.883477368954808));
#14090=CARTESIAN_POINT('Ctrl Pts',(-0.153281414580556,0.0264725929609248,
0.883541124167507));
#14091=CARTESIAN_POINT('Ctrl Pts',(-0.153354558281646,0.0260455309241754,
0.88357209022907));
#14092=CARTESIAN_POINT('Ctrl Pts',(-0.153510990332421,0.0251086674382806,
0.883640099179537));
#14093=CARTESIAN_POINT('Ctrl Pts',(-0.153593525114088,0.0245987472131566,
0.883677165569534));
#14094=CARTESIAN_POINT('Ctrl Pts',(-0.153790103046173,0.0233446670990093,
0.883768453066955));
#14095=CARTESIAN_POINT('Ctrl Pts',(-0.153901285466897,0.0226000790149197,
0.883822763757642));
#14096=CARTESIAN_POINT('Ctrl Pts',(-0.154331458681031,0.0195687112015811,
0.884044341677169));
#14097=CARTESIAN_POINT('Ctrl Pts',(-0.154604904771191,0.017275877942892,
0.88421302417564));
#14098=CARTESIAN_POINT('Ctrl Pts',(-0.155313044927032,0.00995581101386103,
0.884755291129623));
#14099=CARTESIAN_POINT('Ctrl Pts',(-0.155554185082819,0.00491365809576992,
0.88513451871578));
#14100=CARTESIAN_POINT('Ctrl Pts',(-0.155549945051201,-0.000130746198511629,
0.885519163677599));
#14101=CARTESIAN_POINT('Ctrl Pts',(-0.155549945196739,-0.000130572935765169,
0.885519150466002));
#14102=CARTESIAN_POINT('Ctrl Pts',(-0.155538152527638,-0.0141790357481969,
0.886590370869597));
#14103=CARTESIAN_POINT('Ctrl Pts',(-0.153623404595727,-0.02816081303895,
0.88770398506701));
#14104=CARTESIAN_POINT('Ctrl Pts',(-0.149541044889883,-0.0428330689818887,
0.888839113490999));
#14105=CARTESIAN_POINT('Ctrl Pts',(-0.14921167976298,-0.0439667003155691,
0.888926541329305));
#14106=CARTESIAN_POINT('Ctrl Pts',(-0.148624005230768,-0.0459066900059983,
0.889075557530823));
#14107=CARTESIAN_POINT('Ctrl Pts',(-0.148371964239863,-0.0467148737807904,
0.88913745624345));
#14108=CARTESIAN_POINT('Ctrl Pts',(-0.148003154703567,-0.0478643787865776,
0.889225200174473));
#14109=CARTESIAN_POINT('Ctrl Pts',(-0.147891783724052,-0.0482073943796404,
0.889251345374466));
#14110=CARTESIAN_POINT('Ctrl Pts',(-0.147697373281028,-0.0487991515199586,
0.889296380933229));
#14111=CARTESIAN_POINT('Ctrl Pts',(-0.147614896387343,-0.0490480747041561,
0.889315303948344));
#14112=CARTESIAN_POINT('Ctrl Pts',(-0.147453455386157,-0.0495312233690396,
0.889351990095693));
#14113=CARTESIAN_POINT('Ctrl Pts',(-0.147374562564733,-0.0497654690015451,
0.889369757414952));
#14114=CARTESIAN_POINT('Ctrl Pts',(-0.147159594330047,-0.0503987503815633,
0.889417741607176));
#14115=CARTESIAN_POINT('Ctrl Pts',(-0.147022453058591,-0.0507974266202238,
0.889447896192181));
#14116=CARTESIAN_POINT('Ctrl Pts',(-0.146503960123012,-0.052285019992407,
0.889560230750206));
#14117=CARTESIAN_POINT('Ctrl Pts',(-0.146112105248525,-0.0533702778440294,
0.889641817552013));
#14118=CARTESIAN_POINT('Ctrl Pts',(-0.141836509487951,-0.0648115369460556,
0.890499077902331));
#14119=CARTESIAN_POINT('Ctrl Pts',(-0.136870190233698,-0.0747312810406909,
0.891218827987436));
#14120=CARTESIAN_POINT('Ctrl Pts',(-0.128452526781656,-0.0878415956347108,
0.892244842947308));
#14121=CARTESIAN_POINT('Ctrl Pts',(-0.125848290294038,-0.0915336157035162,
0.892542982466153));
#14122=CARTESIAN_POINT('Ctrl Pts',(-0.120416653634604,-0.0985632261996008,
0.893137154663758));
#14123=CARTESIAN_POINT('Ctrl Pts',(-0.117601898405325,-0.10190519367907,
0.893432662166524));
#14124=CARTESIAN_POINT('Ctrl Pts',(-0.112862942599354,-0.107073593066328,
0.893915666907023));
#14125=CARTESIAN_POINT('Ctrl Pts',(-0.111026109819991,-0.108977060128182,
0.894099700781088));
#14126=CARTESIAN_POINT('Ctrl Pts',(-0.108583291972478,-0.111382608533483,
0.894340998330812));
#14127=CARTESIAN_POINT('Ctrl Pts',(-0.108020707526251,-0.111928296174413,
0.894396340733983));
#14128=CARTESIAN_POINT('Ctrl Pts',(-0.107139837867773,-0.112769882812272,
0.894482654388813));
#14129=CARTESIAN_POINT('Ctrl Pts',(-0.106824389843949,-0.113068744820656,
0.894513497571105));
#14130=CARTESIAN_POINT('Ctrl Pts',(-0.106206245705339,-0.113649491664343,
0.89457381038687));
#14131=CARTESIAN_POINT('Ctrl Pts',(-0.105903669113949,-0.113931498912837,
0.894603274432736));
#14132=CARTESIAN_POINT('Ctrl Pts',(-0.105203102553521,-0.114579238383775,
0.894671361523234));
#14133=CARTESIAN_POINT('Ctrl Pts',(-0.104804325864619,-0.114944107817372,
0.894710020661181));
#14134=CARTESIAN_POINT('Ctrl Pts',(-0.103703250385203,-0.115941067435139,
0.894816503521015));
#14135=CARTESIAN_POINT('Ctrl Pts',(-0.102997091527054,-0.116568839413521,
0.894884506956097));
#14136=CARTESIAN_POINT('Ctrl Pts',(-0.0993377146315612,-0.119762797563676,
0.895235492625419));
#14137=CARTESIAN_POINT('Ctrl Pts',(-0.0962944153694092,-0.122223114463218,
0.895522761485409));
#14138=CARTESIAN_POINT('Ctrl Pts',(-0.0915594053831049,-0.125764390743432,
0.895963432868851));
#14139=CARTESIAN_POINT('Ctrl Pts',(-0.0899340338873895,-0.126931775506413,
0.896113632875983));
#14140=CARTESIAN_POINT('Ctrl Pts',(-0.0762350741093716,-0.136375513611164,
0.897370590085317));
#14141=CARTESIAN_POINT('Ctrl Pts',(-0.0630731348671237,-0.142939738315851,
0.898530964540429));
#14142=CARTESIAN_POINT('Ctrl Pts',(-0.0466421964116437,-0.148416694220697,
0.89983512805926));
#14143=CARTESIAN_POINT('Ctrl Pts',(-0.0440735887868415,-0.149199633862116,
0.900034814035675));
#14144=CARTESIAN_POINT('Ctrl Pts',(-0.0409587490884475,-0.150061595442215,
0.900270951339052));
#14145=CARTESIAN_POINT('Ctrl Pts',(-0.0404309230539648,-0.150204667166823,
0.900310760132925));
#14146=CARTESIAN_POINT('Ctrl Pts',(-0.039610233016664,-0.150422482624979,
0.900372326036213));
#14147=CARTESIAN_POINT('Ctrl Pts',(-0.0393178944033794,-0.150499159541276,
0.900394191499956));
#14148=CARTESIAN_POINT('Ctrl Pts',(-0.0387759987737597,-0.150639605553741,
0.900434599984482));
#14149=CARTESIAN_POINT('Ctrl Pts',(-0.0385265091388475,-0.150703606253555,
0.900453155817519));
#14150=CARTESIAN_POINT('Ctrl Pts',(-0.037963184115895,-0.150846623705276,
0.900494945184646));
#14151=CARTESIAN_POINT('Ctrl Pts',(-0.0376492611025511,-0.150925280768664,
0.900518157824987));
#14152=CARTESIAN_POINT('Ctrl Pts',(-0.0367252543927661,-0.151153739038354,
0.900586267489426));
#14153=CARTESIAN_POINT('Ctrl Pts',(-0.0361144960830717,-0.151300827308021,
0.900631012208815));
#14154=CARTESIAN_POINT('Ctrl Pts',(-0.0318048501361557,-0.152311131412774,
0.900944915754908));
#14155=CARTESIAN_POINT('Ctrl Pts',(-0.0280759420180833,-0.15304240194071,
0.901207072237295));
#14156=CARTESIAN_POINT('Ctrl Pts',(-0.0233044485662321,-0.153797821599284,
0.901534949012357));
#14157=CARTESIAN_POINT('Ctrl Pts',(-0.0222836737543572,-0.153949034486008,
0.901604654843597));
#14158=CARTESIAN_POINT('Ctrl Pts',(-0.00634423143215172,-0.156148369163235,
0.902687340657683));
#14159=CARTESIAN_POINT('Ctrl Pts',(0.00879251396618733,-0.156029781423452,
0.903645188548648));
#14160=CARTESIAN_POINT('Ctrl Pts',(0.0258633314586502,-0.153400732166274,
0.90482734189002));
#14161=CARTESIAN_POINT('Ctrl Pts',(0.0280422740574947,-0.153017406214281,
0.904979986524117));
#14162=CARTESIAN_POINT('Ctrl Pts',(0.0312755885443407,-0.152377213371051,
0.905209537944045));
#14163=CARTESIAN_POINT('Ctrl Pts',(0.0323367082795656,-0.152155561148261,
0.905285364420942));
#14164=CARTESIAN_POINT('Ctrl Pts',(0.0342636527589544,-0.151731983727192,
0.905424008634687));
#14165=CARTESIAN_POINT('Ctrl Pts',(0.0351302350894301,-0.151533690346781,
0.905486710100899));
#14166=CARTESIAN_POINT('Ctrl Pts',(0.0365017470432344,-0.151207460880876,
0.905586523910935));
#14167=CARTESIAN_POINT('Ctrl Pts',(0.0370078256185217,-0.151084395601389,
0.905623479907294));
#14168=CARTESIAN_POINT('Ctrl Pts',(0.0375143946125529,-0.150958513168994,
0.905660599930424));
#14169=CARTESIAN_POINT('Ctrl Pts',(0.0375155181777817,-0.150958233949633,
0.905660682262917));
#14170=CARTESIAN_POINT('Ctrl Pts',(0.0375177715377327,-0.150957673936097,
0.905660847385655));
#14171=CARTESIAN_POINT('Ctrl Pts',(0.0375189013217255,-0.150957393144441,
0.905660930175122));
#14172=CARTESIAN_POINT('Ctrl Pts',(0.0375211671584859,-0.150956829976105,
0.905661096214708));
#14173=CARTESIAN_POINT('Ctrl Pts',(0.0375223032079665,-0.150956547600093,
0.905661179464594));
#14174=CARTESIAN_POINT('Ctrl Pts',(0.0375245816304175,-0.150955981248996,
0.90566134642905));
#14175=CARTESIAN_POINT('Ctrl Pts',(0.0375257239959067,-0.150955697275618,
0.90566143014308));
#14176=CARTESIAN_POINT('Ctrl Pts',(0.0375280151120727,-0.150955127713995,
0.905661598040365));
#14177=CARTESIAN_POINT('Ctrl Pts',(0.0375291638492502,-0.150954842128952,
0.90566168222264));
#14178=CARTESIAN_POINT('Ctrl Pts',(0.0375314677528195,-0.150954269332587,
0.905661851059665));
#14179=CARTESIAN_POINT('Ctrl Pts',(0.0375326229117475,-0.150953982122966,
0.905661935713875));
#14180=CARTESIAN_POINT('Ctrl Pts',(0.0375349397125162,-0.150953406063626,
0.90566210549873));
#14181=CARTESIAN_POINT('Ctrl Pts',(0.0375361013465343,-0.150953117215694,
0.905662190628808));
#14182=CARTESIAN_POINT('Ctrl Pts',(0.0375384311483642,-0.150952537866602,
0.90566236136915));
#14183=CARTESIAN_POINT('Ctrl Pts',(0.0375395993097859,-0.150952247366872,
0.905662446978952));
#14184=CARTESIAN_POINT('Ctrl Pts',(0.0375419422235694,-0.150951664699489,
0.905662618682953));
#14185=CARTESIAN_POINT('Ctrl Pts',(0.0375431169680617,-0.150951372533632,
0.905662704776582));
#14186=CARTESIAN_POINT('Ctrl Pts',(0.0375454730244149,-0.150950786539369,
0.905662877446533));
#14187=CARTESIAN_POINT('Ctrl Pts',(0.0375466543323981,-0.150950492711769,
0.905662964022576));
#14188=CARTESIAN_POINT('Ctrl Pts',(0.0379946072117565,-0.150839067478026,
0.905695793989544));
#14189=CARTESIAN_POINT('Ctrl Pts',(0.0384408785224315,-0.150725954317339,
0.905728600849246));
#14190=CARTESIAN_POINT('Ctrl Pts',(0.039437506318027,-0.15046863222028,
0.905802093732532));
#14191=CARTESIAN_POINT('Ctrl Pts',(0.0399875845606474,-0.150323382252826,
0.905842812959197));
#14192=CARTESIAN_POINT('Ctrl Pts',(0.041377450014223,-0.14994821515961,
0.905946097830702));
#14193=CARTESIAN_POINT('Ctrl Pts',(0.0422161169291542,-0.14971426122234,
0.906008793251438));
#14194=CARTESIAN_POINT('Ctrl Pts',(0.0469481021403496,-0.148351308466123,
0.906364689873562));
#14195=CARTESIAN_POINT('Ctrl Pts',(0.0507977291912003,-0.147077598833341,
0.906662553400032));
#14196=CARTESIAN_POINT('Ctrl Pts',(0.0563472049523658,-0.144997602950568,
0.907104757222454));
#14197=CARTESIAN_POINT('Ctrl Pts',(0.0580894069109226,-0.144308463630955,
0.907245471279747));
#14198=CARTESIAN_POINT('Ctrl Pts',(0.0734068482554405,-0.137927228729949,
0.908499274335655));
#14199=CARTESIAN_POINT('Ctrl Pts',(0.0861206404782316,-0.130367340786665,
0.909666635362832));
#14200=CARTESIAN_POINT('Ctrl Pts',(0.0995941270883413,-0.119513551085416,
0.910968053158101));
#14201=CARTESIAN_POINT('Ctrl Pts',(0.101565801392122,-0.117842560889508,
0.911160091223221));
#14202=CARTESIAN_POINT('Ctrl Pts',(0.103897190805273,-0.115764702664121,
0.911388223901601));
#14203=CARTESIAN_POINT('Ctrl Pts',(0.104297451607449,-0.115404221116141,
0.91142742919177));
#14204=CARTESIAN_POINT('Ctrl Pts',(0.104918035565521,-0.114839446944071,
0.911488264545976));
#14205=CARTESIAN_POINT('Ctrl Pts',(0.105139647727574,-0.114636587707616,
0.911509998950918));
#14206=CARTESIAN_POINT('Ctrl Pts',(0.105550281072221,-0.114258509937979,
0.911550287647352));
#14207=CARTESIAN_POINT('Ctrl Pts',(0.105739452623241,-0.11408346544723,
0.911568854110377));
#14208=CARTESIAN_POINT('Ctrl Pts',(0.106166916390006,-0.113685947403785,
0.911610823054837));
#14209=CARTESIAN_POINT('Ctrl Pts',(0.106404944387432,-0.113463194860919,
0.911634203857901));
#14210=CARTESIAN_POINT('Ctrl Pts',(0.107123146368127,-0.112786835803873,
0.911704790470792));
#14211=CARTESIAN_POINT('Ctrl Pts',(0.107601141438976,-0.112330909464413,
0.911751822997039));
#14212=CARTESIAN_POINT('Ctrl Pts',(0.11126914501455,-0.10878735788026,0.912113297600198));
#14213=CARTESIAN_POINT('Ctrl Pts',(0.114328926059272,-0.105567124513092,
0.912418143880914));
#14214=CARTESIAN_POINT('Ctrl Pts',(0.126976025685611,-0.0910608150511777,
0.913716712003752));
#14215=CARTESIAN_POINT('Ctrl Pts',(0.135062192365374,-0.0785699397450294,
0.914658043892356));
#14216=CARTESIAN_POINT('Ctrl Pts',(0.142887838763237,-0.061595167144369,
0.915931718983082));
#14217=CARTESIAN_POINT('Ctrl Pts',(0.144381634668728,-0.0580072261681909,
0.916200111106546));
#14218=CARTESIAN_POINT('Ctrl Pts',(0.14605740588081,-0.0535150836206767,
0.916536992617766));
#14219=CARTESIAN_POINT('Ctrl Pts',(0.146367860098708,-0.052660036601624,
0.91660115020794));
#14220=CARTESIAN_POINT('Ctrl Pts',(0.146846329847733,-0.0513053188852416,
0.916702877184828));
#14221=CARTESIAN_POINT('Ctrl Pts',(0.147019339300464,-0.0508074226356638,
0.916740280968632));
#14222=CARTESIAN_POINT('Ctrl Pts',(0.147338713021705,-0.0498730197670068,
0.916810511878994));
#14223=CARTESIAN_POINT('Ctrl Pts',(0.147485676886321,-0.0494367227937805,
0.916843318803807));
#14224=CARTESIAN_POINT('Ctrl Pts',(0.147809923926955,-0.0484598038430126,
0.916916812574511));
#14225=CARTESIAN_POINT('Ctrl Pts',(0.147986181431481,-0.0479188510841113,
0.916957532627149));
#14226=CARTESIAN_POINT('Ctrl Pts',(0.148424668123391,-0.046547594522173,
0.917060820988422));
#14227=CARTESIAN_POINT('Ctrl Pts',(0.148682897596839,-0.0457160427884443,
0.917123519088245));
#14228=CARTESIAN_POINT('Ctrl Pts',(0.150103940030121,-0.0410005686224286,
0.917479458000172));
#14229=CARTESIAN_POINT('Ctrl Pts',(0.151121433621259,-0.0370748713999017,
0.917777362433376));
#14230=CARTESIAN_POINT('Ctrl Pts',(0.152383102129157,-0.0312841929979406,
0.918219572617918));
#14231=CARTESIAN_POINT('Ctrl Pts',(0.152748730191014,-0.0294471641232828,
0.918360250509824));
#14232=CARTESIAN_POINT('Ctrl Pts',(0.155693402670874,-0.0131171781642028,
0.919614044045814));
#14233=CARTESIAN_POINT('Ctrl Pts',(0.156235868854734,0.00166485672163923,
0.920781434448465));
#14234=CARTESIAN_POINT('Ctrl Pts',(0.154422681920322,0.0188709335403455,
0.922082840303305));
#14235=CARTESIAN_POINT('Ctrl Pts',(0.15408794558242,0.0214332446269605,
0.922274845808125));
#14236=CARTESIAN_POINT('Ctrl Pts',(0.153606447379172,0.0245183999341052,
0.922502945035628));
#14237=CARTESIAN_POINT('Ctrl Pts',(0.153520625463669,0.0250501535346767,
0.922542148391032));
#14238=CARTESIAN_POINT('Ctrl Pts',(0.153382633387528,0.0258778000031592,
0.922602981402059));
#14239=CARTESIAN_POINT('Ctrl Pts',(0.153332366319068,0.0261739985685697,
0.922624715385827));
#14240=CARTESIAN_POINT('Ctrl Pts',(0.153237381674115,0.0267240301159189,
0.922665003701198));
#14241=CARTESIAN_POINT('Ctrl Pts',(0.153192891833672,0.0269778950522651,
0.922683570202268));
#14242=CARTESIAN_POINT('Ctrl Pts',(0.153090697794654,0.0275526228643031,
0.922725539741502));
#14243=CARTESIAN_POINT('Ctrl Pts',(0.153032615863719,0.0278734150248027,
0.922748921098714));
#14244=CARTESIAN_POINT('Ctrl Pts',(0.152853791936818,0.0288436675983817,
0.92281951103822));
#14245=CARTESIAN_POINT('Ctrl Pts',(0.152729918811505,0.0294925551867561,
0.922866546312915));
#14246=CARTESIAN_POINT('Ctrl Pts',(0.151741442733016,0.0344972031778821,
0.923228107995185));
#14247=CARTESIAN_POINT('Ctrl Pts',(0.150694703707889,0.0388154350206104,
0.923533033384837));
#14248=CARTESIAN_POINT('Ctrl Pts',(0.145363318004187,0.0573110100873105,
0.924831812301412));
#14249=CARTESIAN_POINT('Ctrl Pts',(0.139251900616261,0.0708801971536447,
0.925773276471871));
#14250=CARTESIAN_POINT('Ctrl Pts',(0.129232756085471,0.0866589332077304,
0.927046924325926));
#14251=CARTESIAN_POINT('Ctrl Pts',(0.127029785747986,0.0898571373224586,
0.927315115286679));
#14252=CARTESIAN_POINT('Ctrl Pts',(0.12416608844301,0.0936985169473646,
0.927651773656477));
#14253=CARTESIAN_POINT('Ctrl Pts',(0.123616153997182,0.0944228574316695,
0.927715916275253));
#14254=CARTESIAN_POINT('Ctrl Pts',(0.122737536594645,0.0955592873380829,
0.927817624876976));
#14255=CARTESIAN_POINT('Ctrl Pts',(0.122413049996471,0.0959746084337265,
0.927855025359208));
#14256=CARTESIAN_POINT('Ctrl Pts',(0.121801176163229,0.0967496147028431,
0.927925253323625));
#14257=CARTESIAN_POINT('Ctrl Pts',(0.121514289808375,0.0971096896498648,
0.927958060620348));
#14258=CARTESIAN_POINT('Ctrl Pts',(0.120869266403979,0.0979119334542896,
0.928031559454399));
#14259=CARTESIAN_POINT('Ctrl Pts',(0.12051029471596,0.0983534194899055,
0.928072284219391));
#14260=CARTESIAN_POINT('Ctrl Pts',(0.119595764393611,0.0994656431550907,
0.928175592491053));
#14261=CARTESIAN_POINT('Ctrl Pts',(0.119036986151855,0.100133695126451,
0.928238305876175));
#14262=CARTESIAN_POINT('Ctrl Pts',(0.115843451124629,0.103887244260346,
0.928594486152816));
#14263=CARTESIAN_POINT('Ctrl Pts',(0.113094612837865,0.106873137746962,
0.92889262406594));
#14264=CARTESIAN_POINT('Ctrl Pts',(0.10891292461344,0.111073286686013,0.9293348706252));
#14265=CARTESIAN_POINT('Ctrl Pts',(0.107569660273376,0.112374676230265,
0.929475342163363));
#14266=CARTESIAN_POINT('Ctrl Pts',(0.0954464200580246,0.123703416634404,
0.930729081834463));
#14267=CARTESIAN_POINT('Ctrl Pts',(0.0833187671933404,0.132175867318789,
0.931896640345904));
#14268=CARTESIAN_POINT('Ctrl Pts',(0.0678789658641286,0.139981820714347,
0.93319797798148));
#14269=CARTESIAN_POINT('Ctrl Pts',(0.0655467783845755,0.14108892975694,
0.933389797258561));
#14270=CARTESIAN_POINT('Ctrl Pts',(0.0626958992149843,0.14235630183139,
0.933617705153987));
#14271=CARTESIAN_POINT('Ctrl Pts',(0.0622027173212019,0.14257248833633,
0.933656897435981));
#14272=CARTESIAN_POINT('Ctrl Pts',(0.0614326658553099,0.142905284381127,
0.933717717035966));
#14273=CARTESIAN_POINT('Ctrl Pts',(0.061156570877564,0.143023657416573,
0.933739448609067));
#14274=CARTESIAN_POINT('Ctrl Pts',(0.0606429527111171,0.143242106994375,
0.933779734743845));
#14275=CARTESIAN_POINT('Ctrl Pts',(0.0604055260906377,0.14334239201737,
0.933798301463162));
#14276=CARTESIAN_POINT('Ctrl Pts',(0.05986717704097,0.143568206509304,0.933840274408923));
#14277=CARTESIAN_POINT('Ctrl Pts',(0.0595661090887147,0.143693380016156,
0.933863658939628));
#14278=CARTESIAN_POINT('Ctrl Pts',(0.0586536810408798,0.14406937518277,
0.933934267931659));
#14279=CARTESIAN_POINT('Ctrl Pts',(0.058041103329471,0.144317253061305,
0.933981318947773));
#14280=CARTESIAN_POINT('Ctrl Pts',(0.0532935766457031,0.146203208140537,
0.934343380401504));
#14281=CARTESIAN_POINT('Ctrl Pts',(0.0490911842966859,0.147667356909277,
0.93464875982257));
#14282=CARTESIAN_POINT('Ctrl Pts',(0.0306409878440384,0.153220561271546,
0.935948755156329));
#14283=CARTESIAN_POINT('Ctrl Pts',(0.0159131608208337,0.155442046342665,
0.936890984581909));
#14284=CARTESIAN_POINT('Ctrl Pts',(-0.00277245758209385,0.15557331520756,
0.938164478424675));
#14285=CARTESIAN_POINT('Ctrl Pts',(-0.00663700638285604,0.15545638864657,
0.938431509426429));
#14286=CARTESIAN_POINT('Ctrl Pts',(-0.0113990712733975,0.155134420799282,
0.938766880965891));
#14287=CARTESIAN_POINT('Ctrl Pts',(-0.0123046394880982,0.1550652221718,
0.938830937000372));
#14288=CARTESIAN_POINT('Ctrl Pts',(-0.0137344108026052,0.154943363710533,
0.93893253933082));
#14289=CARTESIAN_POINT('Ctrl Pts',(-0.0142590521131872,0.154895963208998,
0.938969920716547));
#14290=CARTESIAN_POINT('Ctrl Pts',(-0.0152417710738129,0.154802141134066,
0.939040131662229));
#14291=CARTESIAN_POINT('Ctrl Pts',(-0.0156999043182575,0.1547563487589,
0.939072941130983));
#14292=CARTESIAN_POINT('Ctrl Pts',(-0.0167241312670081,0.154649378067233,
0.93914646935182));
#14293=CARTESIAN_POINT('Ctrl Pts',(-0.017290103427844,0.154587124336835,
0.939187221452907));
#14294=CARTESIAN_POINT('Ctrl Pts',(-0.018722103348753,0.154421650034999,
0.939290645241007));
#14295=CARTESIAN_POINT('Ctrl Pts',(-0.0195876184459121,0.154314251770064,
0.939353447313268));
#14296=CARTESIAN_POINT('Ctrl Pts',(-0.0244901941423557,0.153664001605169,
0.93971088110266));
#14297=CARTESIAN_POINT('Ctrl Pts',(-0.0285052403014864,0.152970064208931,
0.940010221954393));
#14298=CARTESIAN_POINT('Ctrl Pts',(-0.0432248145238853,0.149826409029404,
0.941133473445246));
#14299=CARTESIAN_POINT('Ctrl Pts',(-0.0536831418144325,0.146404218878681,
0.941985602790749));
#14300=CARTESIAN_POINT('Ctrl Pts',(-0.0636886279045124,0.141913921711862,
0.942835077379979));
#14301=CARTESIAN_POINT('Origin',(0.,0.,-0.129405622560373));
#14302=CARTESIAN_POINT('',(-0.0636886257384703,0.141913922683946,1.02674653231234));
#14303=CARTESIAN_POINT('',(-0.0636886260608369,0.141913922539273,1.01289638536134));
#14304=CARTESIAN_POINT('',(-0.0636886258329924,0.141913922641526,-0.129405622560373));
#14305=CARTESIAN_POINT('',(-0.155549936890276,0.00014011934593126,0.969453892031266));
#14306=CARTESIAN_POINT('Ctrl Pts',(-0.0636886257384703,0.141913922683946,
1.02674653231234));
#14307=CARTESIAN_POINT('Ctrl Pts',(-0.0630352306679285,0.142207155605143,
1.02669405911617));
#14308=CARTESIAN_POINT('Ctrl Pts',(-0.0623798065897889,0.142495877757158,
1.0266414348019));
#14309=CARTESIAN_POINT('Ctrl Pts',(-0.0576415668584197,0.144544171545589,
1.02626107071648));
#14310=CARTESIAN_POINT('Ctrl Pts',(-0.0534873655959961,0.146132346438471,
1.02592788080371));
#14311=CARTESIAN_POINT('Ctrl Pts',(-0.0376529200786634,0.151420271184699,
1.02465969010187));
#14312=CARTESIAN_POINT('Ctrl Pts',(-0.0256183551010184,0.153913939049909,
1.02369533159991));
#14313=CARTESIAN_POINT('Ctrl Pts',(-0.0126319359965695,0.155038243789787,
1.02270248284392));
#14314=CARTESIAN_POINT('Ctrl Pts',(-0.0118467337456412,0.155100218522508,
1.02264265376301));
#14315=CARTESIAN_POINT('Ctrl Pts',(-0.00783342961095387,0.155386326824878,
1.02233798649972));
#14316=CARTESIAN_POINT('Ctrl Pts',(-0.00459907048430397,0.155515676572398,
1.02209616941057));
#14317=CARTESIAN_POINT('Ctrl Pts',(-0.000814431946987157,0.155548834359067,
1.02181924660198));
#14318=CARTESIAN_POINT('Ctrl Pts',(-0.000266086682487207,0.155550738962588,
1.0217792724826));
#14319=CARTESIAN_POINT('Ctrl Pts',(0.000614623215861104,0.155549140783889,
1.0217153194843));
#14320=CARTESIAN_POINT('Ctrl Pts',(0.000946979797115376,0.155547472480817,
1.02169124257916));
#14321=CARTESIAN_POINT('Ctrl Pts',(0.00153830136032678,0.155542608947653,
1.02164851034128));
#14322=CARTESIAN_POINT('Ctrl Pts',(0.00179726617478012,0.155539832222134,
1.02162983199114));
#14323=CARTESIAN_POINT('Ctrl Pts',(0.00234898534973309,0.155532538361492,
1.02159011544398));
#14324=CARTESIAN_POINT('Ctrl Pts',(0.00264173362726414,0.155527841458206,
1.02156908741561));
#14325=CARTESIAN_POINT('Ctrl Pts',(0.00343798422600656,0.155512817417418,
1.02151201381604));
#14326=CARTESIAN_POINT('Ctrl Pts',(0.0039414584958467,0.155500871510094,
1.02147605728297));
#14327=CARTESIAN_POINT('Ctrl Pts',(0.00652129801348688,0.155427121916947,
1.0212924459474));
#14328=CARTESIAN_POINT('Ctrl Pts',(0.00859646117933128,0.155326171485528,
1.02114685331092));
#14329=CARTESIAN_POINT('Ctrl Pts',(0.0146989950671047,0.154906613003737,
1.02072323300142));
#14330=CARTESIAN_POINT('Ctrl Pts',(0.0187169036301496,0.154472658424671,
1.02045012918477));
#14331=CARTESIAN_POINT('Ctrl Pts',(0.0330399681741005,0.152358519906227,
1.01948306500855));
#14332=CARTESIAN_POINT('Ctrl Pts',(0.0431866612744261,0.149798802724692,
1.01880841875851));
#14333=CARTESIAN_POINT('Ctrl Pts',(0.0591025861724015,0.144030586955267,
1.01767622026813));
#14334=CARTESIAN_POINT('Ctrl Pts',(0.065059301505784,0.141439723788827,
1.01723465794199));
#14335=CARTESIAN_POINT('Ctrl Pts',(0.0717217606801996,0.138031810554476,
1.01671032275089));
#14336=CARTESIAN_POINT('Ctrl Pts',(0.0726028389250547,0.137570416073688,
1.01664035119534));
#14337=CARTESIAN_POINT('Ctrl Pts',(0.0740083912343247,0.136817106823851,
1.01652768053613));
#14338=CARTESIAN_POINT('Ctrl Pts',(0.0745357162886557,0.136530544830826,
1.01648517048202));
#14339=CARTESIAN_POINT('Ctrl Pts',(0.0754688162561447,0.136016457402152,
1.01640951661746));
#14340=CARTESIAN_POINT('Ctrl Pts',(0.0758752561609753,0.135790148410093,
1.01637641644931));
#14341=CARTESIAN_POINT('Ctrl Pts',(0.0767196976671625,0.13531498166623,
1.01630733577342));
#14342=CARTESIAN_POINT('Ctrl Pts',(0.077157517068472,0.135065812929438,
1.01627134440373));
#14343=CARTESIAN_POINT('Ctrl Pts',(0.0782907064869744,0.134413592192337,
1.01617772922887));
#14344=CARTESIAN_POINT('Ctrl Pts',(0.0789841689900054,0.134007274027301,
1.01611998810601));
#14345=CARTESIAN_POINT('Ctrl Pts',(0.0819741119203691,0.132224116386185,
1.01586903200626));
#14346=CARTESIAN_POINT('Ctrl Pts',(0.0842378465335957,0.130793560755221,
1.0156738728988));
#14347=CARTESIAN_POINT('Ctrl Pts',(0.090140015025796,0.126846921983579,
1.01515074952546));
#14348=CARTESIAN_POINT('Ctrl Pts',(0.0937097478716353,0.124233008385915,
1.01481933954105));
#14349=CARTESIAN_POINT('Ctrl Pts',(0.106822161809964,0.113744550049465,
1.01354402700956));
#14350=CARTESIAN_POINT('Ctrl Pts',(0.115524243844455,0.104894731285634,
1.01256988475825));
#14351=CARTESIAN_POINT('Ctrl Pts',(0.125463452194823,0.0920317474293646,
1.01133245658215));
#14352=CARTESIAN_POINT('Ctrl Pts',(0.127724876853017,0.0888666564937184,
1.011040545508));
#14353=CARTESIAN_POINT('Ctrl Pts',(0.130213332602004,0.0850922430263657,
1.01070953922736));
#14354=CARTESIAN_POINT('Ctrl Pts',(0.130557946694873,0.0845625472781061,
1.0106634656141));
#14355=CARTESIAN_POINT('Ctrl Pts',(0.131074622092326,0.0837576935708865,
1.01059404753511));
#14356=CARTESIAN_POINT('Ctrl Pts',(0.131249060443669,0.0834840818769859,
1.01057055094043));
#14357=CARTESIAN_POINT('Ctrl Pts',(0.131560498636436,0.0829921930598325,
1.01052849549684));
#14358=CARTESIAN_POINT('Ctrl Pts',(0.131697812672667,0.0827741206599731,
1.01050991615471));
#14359=CARTESIAN_POINT('Ctrl Pts',(0.131994735435516,0.0822999597150525,
1.01046966055638));
#14360=CARTESIAN_POINT('Ctrl Pts',(0.132154140707772,0.0820437483894939,
1.0104479977369));
#14361=CARTESIAN_POINT('Ctrl Pts',(0.132599042640065,0.0813239986832844,
1.01038738720437));
#14362=CARTESIAN_POINT('Ctrl Pts',(0.132882856741106,0.0808594167606562,
1.01034854804946));
#14363=CARTESIAN_POINT('Ctrl Pts',(0.134548197872611,0.0781009313201563,
1.01011955087143));
#14364=CARTESIAN_POINT('Ctrl Pts',(0.135872851223409,0.0757729744201464,
1.00993286457653));
#14365=CARTESIAN_POINT('Ctrl Pts',(0.144050328767804,0.06049704387074,1.00874192826109));
#14366=CARTESIAN_POINT('Ctrl Pts',(0.149105563105364,0.0466693227503142,
1.00781299064504));
#14367=CARTESIAN_POINT('Ctrl Pts',(0.152570019515499,0.030368440483885,
1.00669316346403));
#14368=CARTESIAN_POINT('Ctrl Pts',(0.152950155307709,0.028391944930931,
1.00655712433383));
#14369=CARTESIAN_POINT('Ctrl Pts',(0.15395382947274,0.0225660196310106,
1.00615457127069));
#14370=CARTESIAN_POINT('Ctrl Pts',(0.154471057883322,0.0187001267212292,
1.00588542005788));
#14371=CARTESIAN_POINT('Ctrl Pts',(0.154932419211424,0.0138794487615835,
1.0055453891294));
#14372=CARTESIAN_POINT('Ctrl Pts',(0.155013794859819,0.0129389703509694,
1.00547884737501));
#14373=CARTESIAN_POINT('Ctrl Pts',(0.155128287171852,0.0114590171259123,
1.00537378983941));
#14374=CARTESIAN_POINT('Ctrl Pts',(0.155167161982236,0.0109199992374513,
1.00533545445845));
#14375=CARTESIAN_POINT('Ctrl Pts',(0.155230839539519,0.00996795639691497,
1.00526761242679));
#14376=CARTESIAN_POINT('Ctrl Pts',(0.155256804798304,0.00955501212076111,
1.00523814245089));
#14377=CARTESIAN_POINT('Ctrl Pts',(0.155312525769058,0.00860856270042894,
1.00517049571296));
#14378=CARTESIAN_POINT('Ctrl Pts',(0.155341180519754,0.00807500056360406,
1.00513228488903));
#14379=CARTESIAN_POINT('Ctrl Pts',(0.155412762250503,0.00660026360220895,
1.00502645929071));
#14380=CARTESIAN_POINT('Ctrl Pts',(0.155449887627298,0.00565884387846968,
1.00495866432382));
#14381=CARTESIAN_POINT('Ctrl Pts',(0.155610880917971,0.000352479944241274,
1.00457512625096));
#14382=CARTESIAN_POINT('Ctrl Pts',(0.155559442127116,-0.00401539858204799,
1.00425397169674));
#14383=CARTESIAN_POINT('Ctrl Pts',(0.154814887628769,-0.0178241302734176,
1.00322016677576));
#14384=CARTESIAN_POINT('Ctrl Pts',(0.15344426084606,-0.027205923441768,
1.0024888594306));
#14385=CARTESIAN_POINT('Ctrl Pts',(0.150503608444309,-0.0394221428117864,
1.00151441813805));
#14386=CARTESIAN_POINT('Ctrl Pts',(0.149686795644279,-0.0424182200064618,
1.00127377356817));
#14387=CARTESIAN_POINT('Ctrl Pts',(0.147962610875359,-0.0480700728279184,
1.00081840104725));
#14388=CARTESIAN_POINT('Ctrl Pts',(0.147071949488602,-0.0507297669582083,
1.00060349993731));
#14389=CARTESIAN_POINT('Ctrl Pts',(0.144948043181759,-0.0565449858653637,
1.00013409988177));
#14390=CARTESIAN_POINT('Ctrl Pts',(0.143682574022113,-0.0596874610987846,
0.999880749735729));
#14391=CARTESIAN_POINT('Ctrl Pts',(0.142091102582054,-0.0632947851830865,
0.999592214849562));
#14392=CARTESIAN_POINT('Ctrl Pts',(0.141864085888583,-0.0638019782167183,
0.999551700719325));
#14393=CARTESIAN_POINT('Ctrl Pts',(0.141496054848492,-0.0646125441648346,
0.999487052780408));
#14394=CARTESIAN_POINT('Ctrl Pts',(0.141356774152863,-0.0649166912892718,
0.99946281758712));
#14395=CARTESIAN_POINT('Ctrl Pts',(0.141107811279407,-0.0654557507488711,
0.999419907080047));
#14396=CARTESIAN_POINT('Ctrl Pts',(0.140998521862669,-0.0656908406618156,
0.999401208039142));
#14397=CARTESIAN_POINT('Ctrl Pts',(0.140765094829428,-0.0661896937195439,
0.99936156143802));
#14398=CARTESIAN_POINT('Ctrl Pts',(0.140640803609722,-0.0664533809587728,
0.999340623563209));
#14399=CARTESIAN_POINT('Ctrl Pts',(0.140302232723181,-0.06716646380878,
0.999284048552469));
#14400=CARTESIAN_POINT('Ctrl Pts',(0.140086533082748,-0.0676151879000025,
0.999248497839715));
#14401=CARTESIAN_POINT('Ctrl Pts',(0.138991126633436,-0.0698662395727306,
0.999070370663153));
#14402=CARTESIAN_POINT('Ctrl Pts',(0.138078723254914,-0.0716525779654174,
0.998929712154224));
#14403=CARTESIAN_POINT('Ctrl Pts',(0.135323120697832,-0.0767993589792354,
0.99852501722293));
#14404=CARTESIAN_POINT('Ctrl Pts',(0.133389886847989,-0.0801101206653924,
0.998265397545028));
#14405=CARTESIAN_POINT('Ctrl Pts',(0.125778548189099,-0.0921039779726331,
0.99731481138957));
#14406=CARTESIAN_POINT('Ctrl Pts',(0.119358859612558,-0.100283910033483,
0.996644490199267));
#14407=CARTESIAN_POINT('Ctrl Pts',(0.107440462666309,-0.112689859593906,
0.995496083866646));
#14408=CARTESIAN_POINT('Ctrl Pts',(0.102389696044359,-0.117297858863065,
0.995032228321061));
#14409=CARTESIAN_POINT('Ctrl Pts',(0.096269161267774,-0.122184520909687,
0.994483542016292));
#14410=CARTESIAN_POINT('Ctrl Pts',(0.0954793016760473,-0.122802733801713,
0.994412982603241));
#14411=CARTESIAN_POINT('Ctrl Pts',(0.0942053998639343,-0.123780080434601,
0.994299546310084));
#14412=CARTESIAN_POINT('Ctrl Pts',(0.09372514356311,-0.12414412237997,0.994256862638636));
#14413=CARTESIAN_POINT('Ctrl Pts',(0.0928701324047044,-0.124784445222554,
0.994181008723361));
#14414=CARTESIAN_POINT('Ctrl Pts',(0.0924962274448928,-0.12506185334547,
0.994147882913742));
#14415=CARTESIAN_POINT('Ctrl Pts',(0.0917160795285165,-0.125635249416698,
0.994078858015699));
#14416=CARTESIAN_POINT('Ctrl Pts',(0.0913096366509977,-0.125930954827646,
0.994042948511566));
#14417=CARTESIAN_POINT('Ctrl Pts',(0.0902537015299882,-0.126691395434084,
0.993949783181154));
#14418=CARTESIAN_POINT('Ctrl Pts',(0.0896020577111059,-0.127153102701747,
0.993892412146157));
#14419=CARTESIAN_POINT('Ctrl Pts',(0.0867890177829316,-0.129113855311558,
0.993645250250577));
#14420=CARTESIAN_POINT('Ctrl Pts',(0.084593463939754,-0.130562879600856,
0.993453587361467));
#14421=CARTESIAN_POINT('Ctrl Pts',(0.0787024285672941,-0.134239874011988,
0.992942167061363));
#14422=CARTESIAN_POINT('Ctrl Pts',(0.0749493885211219,-0.136370814095713,
0.992619152581192));
#14423=CARTESIAN_POINT('Ctrl Pts',(0.0582705078776675,-0.144944326988716,
0.991196164483745));
#14424=CARTESIAN_POINT('Ctrl Pts',(0.0445730419396786,-0.149724754493238,
0.990050930265348));
#14425=CARTESIAN_POINT('Ctrl Pts',(0.030168111211927,-0.152596691593575,
0.988950502576982));
#14426=CARTESIAN_POINT('Ctrl Pts',(0.0299223868857948,-0.15264506537789,
0.988931763350734));
#14427=CARTESIAN_POINT('Ctrl Pts',(0.0290873360485386,-0.152807361284316,
0.988868193157962));
#14428=CARTESIAN_POINT('Ctrl Pts',(0.0284974585208203,-0.152918467376053,
0.988823476261369));
#14429=CARTESIAN_POINT('Ctrl Pts',(0.0264779803126232,-0.153286753833623,
0.988671062692387));
#14430=CARTESIAN_POINT('Ctrl Pts',(0.0250453674192803,-0.153527334131997,
0.988564098787129));
#14431=CARTESIAN_POINT('Ctrl Pts',(0.0231521718021301,-0.15381805338242,
0.988424448638687));
#14432=CARTESIAN_POINT('Ctrl Pts',(0.022694498350447,-0.153886244885385,
0.988390819451182));
#14433=CARTESIAN_POINT('Ctrl Pts',(0.0219557574399018,-0.153992946874617,
0.988336755862827));
#14434=CARTESIAN_POINT('Ctrl Pts',(0.021674881811729,-0.154032731826293,
0.988316251189596));
#14435=CARTESIAN_POINT('Ctrl Pts',(0.0211347852625754,-0.15410772785524,
0.988276922248808));
#14436=CARTESIAN_POINT('Ctrl Pts',(0.0208755842678257,-0.154143053412833,
0.988258091934976));
#14437=CARTESIAN_POINT('Ctrl Pts',(0.0202630193151008,-0.154224964199205,
0.98821369298856));
#14438=CARTESIAN_POINT('Ctrl Pts',(0.0199095792797009,-0.154270989475555,
0.988188155824479));
#14439=CARTESIAN_POINT('Ctrl Pts',(0.018792791402094,-0.154412516660218,
0.988107708892055));
#14440=CARTESIAN_POINT('Ctrl Pts',(0.0180288755335209,-0.154503572844977,
0.988053041332966));
#14441=CARTESIAN_POINT('Ctrl Pts',(0.0116014473685904,-0.155221379692399,
0.987595867133344));
#14442=CARTESIAN_POINT('Ctrl Pts',(0.00590733513091148,-0.155542248908363,
0.987208968863565));
#14443=CARTESIAN_POINT('Ctrl Pts',(-0.0137828839692928,-0.155568547137174,
0.985894090575662));
#14444=CARTESIAN_POINT('Ctrl Pts',(-0.0277114019557472,-0.153699792994551,
0.984997969551863));
#14445=CARTESIAN_POINT('Ctrl Pts',(-0.042777412245691,-0.149561234221445,
0.983928331536351));
#14446=CARTESIAN_POINT('Ctrl Pts',(-0.044345296853919,-0.149103870196441,
0.983815848658988));
#14447=CARTESIAN_POINT('Ctrl Pts',(-0.046750282563141,-0.148361029444013,
0.983641321803609));
#14448=CARTESIAN_POINT('Ctrl Pts',(-0.0475926670679483,-0.148092950421283,
0.983579811398731));
#14449=CARTESIAN_POINT('Ctrl Pts',(-0.0495926861862118,-0.147437640996896,
0.983432826465254));
#14450=CARTESIAN_POINT('Ctrl Pts',(-0.0507481220980271,-0.147043940577151,
0.983347152450299));
#14451=CARTESIAN_POINT('Ctrl Pts',(-0.0524684626897892,-0.146435064513183,
0.983218396428757));
#14452=CARTESIAN_POINT('Ctrl Pts',(-0.0530369616348882,-0.146230121308723,
0.983175651419479));
#14453=CARTESIAN_POINT('Ctrl Pts',(-0.0540150689540782,-0.145871060689959,
0.983101761635701));
#14454=CARTESIAN_POINT('Ctrl Pts',(-0.0544252509966532,-0.145718516557564,
0.9830706693382));
#14455=CARTESIAN_POINT('Ctrl Pts',(-0.0552722627075692,-0.145399443004196,
0.983006243090929));
#14456=CARTESIAN_POINT('Ctrl Pts',(-0.0557089957467054,-0.145232671375499,
0.9829729013307));
#14457=CARTESIAN_POINT('Ctrl Pts',(-0.0567165572734705,-0.144842708786945,
0.982895693200521));
#14458=CARTESIAN_POINT('Ctrl Pts',(-0.0572868283126382,-0.144618108961725,
0.982851780008853));
#14459=CARTESIAN_POINT('Ctrl Pts',(-0.0590973254702236,-0.143892660086581,
0.982711671492993));
#14460=CARTESIAN_POINT('Ctrl Pts',(-0.0603323957121858,-0.14337919418218,
0.982615053426657));
#14461=CARTESIAN_POINT('Ctrl Pts',(-0.0632071085482083,-0.142140346744301,
0.982387659790866));
#14462=CARTESIAN_POINT('Ctrl Pts',(-0.0648411051055526,-0.141402430452105,
0.98225647098647));
#14463=CARTESIAN_POINT('Ctrl Pts',(-0.0705242220952803,-0.13871670541187,
0.981793213513812));
#14464=CARTESIAN_POINT('Ctrl Pts',(-0.0745010504269431,-0.136622021439553,
0.981456361686497));
#14465=CARTESIAN_POINT('Ctrl Pts',(-0.0845558187773673,-0.130756319092542,
0.980571701250823));
#14466=CARTESIAN_POINT('Ctrl Pts',(-0.0904742448205335,-0.126733177547743,
0.980017594534704));
#14467=CARTESIAN_POINT('Ctrl Pts',(-0.103106691198302,-0.116808940856877,
0.978771907112906));
#14468=CARTESIAN_POINT('Ctrl Pts',(-0.109633067609805,-0.110706604689759,
0.978082237452275));
#14469=CARTESIAN_POINT('Ctrl Pts',(-0.116061570381856,-0.103566345555614,
0.97737807830484));
#14470=CARTESIAN_POINT('Ctrl Pts',(-0.11651862141399,-0.103051865399575,
0.977327869846842));
#14471=CARTESIAN_POINT('Ctrl Pts',(-0.117190791718214,-0.102285046562854,
0.977253836011245));
#14472=CARTESIAN_POINT('Ctrl Pts',(-0.117408534255182,-0.102035035666798,
0.977229822934923));
#14473=CARTESIAN_POINT('Ctrl Pts',(-0.117794487531771,-0.101589014751518,
0.977187207578976));
#14474=CARTESIAN_POINT('Ctrl Pts',(-0.117963010565243,-0.101393280611942,
0.977168582427088));
#14475=CARTESIAN_POINT('Ctrl Pts',(-0.118324115173727,-0.100971750186091,
0.977128635918741));
#14476=CARTESIAN_POINT('Ctrl Pts',(-0.118516537873616,-0.100745822850169,
0.977107326207094));
#14477=CARTESIAN_POINT('Ctrl Pts',(-0.119045392234047,-0.10012127231349,
0.977048689559062));
#14478=CARTESIAN_POINT('Ctrl Pts',(-0.11938047146774,-0.0997215003639668,
0.977011460075556));
#14479=CARTESIAN_POINT('Ctrl Pts',(-0.12117147603577,-0.0975627467969924,
0.976811999801817));
#14480=CARTESIAN_POINT('Ctrl Pts',(-0.122590646726793,-0.0957734357162094,
0.976652271643523));
#14481=CARTESIAN_POINT('Ctrl Pts',(-0.12795122684845,-0.0887002363019829,
0.976039328255174));
#14482=CARTESIAN_POINT('Ctrl Pts',(-0.131594973069662,-0.0831987388151121,
0.975601336925232));
#14483=CARTESIAN_POINT('Ctrl Pts',(-0.137842295687083,-0.0723235505690146,
0.974773767496741));
#14484=CARTESIAN_POINT('Ctrl Pts',(-0.140507236782163,-0.0669993277992513,
0.974384313582742));
#14485=CARTESIAN_POINT('Ctrl Pts',(-0.146072524104153,-0.0540789901738317,
0.973450940480724));
#14486=CARTESIAN_POINT('Ctrl Pts',(-0.148695198689844,-0.0463834788812116,
0.9729034867842));
#14487=CARTESIAN_POINT('Ctrl Pts',(-0.15096062193687,-0.0375200830573085,
0.972262854614899));
#14488=CARTESIAN_POINT('Ctrl Pts',(-0.151206048609356,-0.036518444402699,
0.972190331305487));
#14489=CARTESIAN_POINT('Ctrl Pts',(-0.151580964764115,-0.0349197192255328,
0.972074340434997));
#14490=CARTESIAN_POINT('Ctrl Pts',(-0.15171693064462,-0.0343241694163665,
0.972031080281636));
#14491=CARTESIAN_POINT('Ctrl Pts',(-0.15195061745934,-0.0332720653735112,
0.971954558171104));
#14492=CARTESIAN_POINT('Ctrl Pts',(-0.152049798125487,-0.0328158401049746,
0.971921343288194));
#14493=CARTESIAN_POINT('Ctrl Pts',(-0.152236568023895,-0.0319376823317655,
0.971857344567772));
#14494=CARTESIAN_POINT('Ctrl Pts',(-0.152324460921639,-0.0315158181626794,
0.971826570757795));
#14495=CARTESIAN_POINT('Ctrl Pts',(-0.15250846787461,-0.0306138765536068,
0.971760712137446));
#14496=CARTESIAN_POINT('Ctrl Pts',(-0.152604070325346,-0.0301337007531674,
0.971725611364373));
#14497=CARTESIAN_POINT('Ctrl Pts',(-0.152828228193531,-0.0289794086288356,
0.971641135507136));
#14498=CARTESIAN_POINT('Ctrl Pts',(-0.152954591495778,-0.0283048824329136,
0.971591691354873));
#14499=CARTESIAN_POINT('Ctrl Pts',(-0.153522877886142,-0.0251563955149873,
0.971360512478664));
#14500=CARTESIAN_POINT('Ctrl Pts',(-0.15390924373343,-0.0226729265187878,
0.971177038246144));
#14501=CARTESIAN_POINT('Ctrl Pts',(-0.155117025923269,-0.0134424784721329,
0.970490528255298));
#14502=CARTESIAN_POINT('Ctrl Pts',(-0.155556057183704,-0.00665416912435971,
0.969976199532121));
#14503=CARTESIAN_POINT('Ctrl Pts',(-0.155549936890276,0.00014011934593126,
0.969453892031266));
#14504=CARTESIAN_POINT('Ctrl Pts',(-0.155549937001753,0.00013999553845127,
0.969453901548902));
#14505=CARTESIAN_POINT('Ctrl Pts',(-0.155538063581429,0.0133326287020923,
0.968439724690961));
#14506=CARTESIAN_POINT('Ctrl Pts',(-0.153847975061747,0.0264709038583835,
0.96739735679523));
#14507=CARTESIAN_POINT('Ctrl Pts',(-0.150341752135942,0.0399206228266964,
0.966372199424086));
#14508=CARTESIAN_POINT('Ctrl Pts',(-0.150159449777708,0.0406009636922113,
0.966320474541299));
#14509=CARTESIAN_POINT('Ctrl Pts',(-0.149865254441721,0.0416697901246329,
0.966239446105639));
#14510=CARTESIAN_POINT('Ctrl Pts',(-0.149756460307496,0.0420591072626695,
0.966209980399501));
#14511=CARTESIAN_POINT('Ctrl Pts',(-0.14954746175416,0.0427959105822705,
0.966154312981632));
#14512=CARTESIAN_POINT('Ctrl Pts',(-0.149447561013226,0.0431434791603147,
0.966128094706468));
#14513=CARTESIAN_POINT('Ctrl Pts',(-0.149273064956088,0.0437426961357795,
0.966082969047862));
#14514=CARTESIAN_POINT('Ctrl Pts',(-0.14919904359982,0.043994508520487,
0.966064028690258));
#14515=CARTESIAN_POINT('Ctrl Pts',(-0.149054123432694,0.0444829382910349,
0.966027336978042));
#14516=CARTESIAN_POINT('Ctrl Pts',(-0.148983298445989,0.0447195739892545,
0.966009581323496));
#14517=CARTESIAN_POINT('Ctrl Pts',(-0.148790385769705,0.0453585758574079,
0.96596168843626));
#14518=CARTESIAN_POINT('Ctrl Pts',(-0.148667228541293,0.0457606213929604,
0.965931613040074));
#14519=CARTESIAN_POINT('Ctrl Pts',(-0.148202364632928,0.0472564787402857,
0.965819911902308));
#14520=CARTESIAN_POINT('Ctrl Pts',(-0.147850193040741,0.0483470401309401,
0.965738870691897));
#14521=CARTESIAN_POINT('Ctrl Pts',(-0.143937089513277,0.0600218388052825,
0.964874540776392));
#14522=CARTESIAN_POINT('Ctrl Pts',(-0.139257682058014,0.0701989279265626,
0.964148331841343));
#14523=CARTESIAN_POINT('Ctrl Pts',(-0.130476418450045,0.0848945881474805,
0.963020807890539));
#14524=CARTESIAN_POINT('Ctrl Pts',(-0.127134947714255,0.0898214061625449,
0.962627603067687));
#14525=CARTESIAN_POINT('Ctrl Pts',(-0.121456318897918,0.0972403748156322,
0.961997027651078));
#14526=CARTESIAN_POINT('Ctrl Pts',(-0.11930529405679,0.099867773011555,
0.961765440021246));
#14527=CARTESIAN_POINT('Ctrl Pts',(-0.115625740977078,0.104073544230565,
0.961378831861088));
#14528=CARTESIAN_POINT('Ctrl Pts',(-0.114146629132364,0.105693712220032,
0.961225760216138));
#14529=CARTESIAN_POINT('Ctrl Pts',(-0.112128227808992,0.10781280260133,
0.961019606789338));
#14530=CARTESIAN_POINT('Ctrl Pts',(-0.111618902524712,0.108340022348401,
0.960967809708947));
#14531=CARTESIAN_POINT('Ctrl Pts',(-0.110803574142548,0.109172144043803,
0.96088523450927));
#14532=CARTESIAN_POINT('Ctrl Pts',(-0.110499989881001,0.109479410426454,
0.960854562077295));
#14533=CARTESIAN_POINT('Ctrl Pts',(-0.109869009262583,0.110112745909587,
0.960790961315572));
#14534=CARTESIAN_POINT('Ctrl Pts',(-0.109541432329764,0.110438628218438,
0.960758025198734));
#14535=CARTESIAN_POINT('Ctrl Pts',(-0.108795167077099,0.111174446102175,
0.960683175131711));
#14536=CARTESIAN_POINT('Ctrl Pts',(-0.108375606736996,0.111583483062982,
0.960641222543674));
#14537=CARTESIAN_POINT('Ctrl Pts',(-0.107287225097557,0.112632636905629,
0.960532717301163));
#14538=CARTESIAN_POINT('Ctrl Pts',(-0.106614990726881,0.113269162832774,
0.96046601116039));
#14539=CARTESIAN_POINT('Ctrl Pts',(-0.102321723565499,0.11726229574931,
0.960041885322198));
#14540=CARTESIAN_POINT('Ctrl Pts',(-0.0985486826696047,0.120450521752605,
0.959677465052248));
#14541=CARTESIAN_POINT('Ctrl Pts',(-0.0871678471949762,0.129174262363729,
0.958600134462228));
#14542=CARTESIAN_POINT('Ctrl Pts',(-0.0792023049743255,0.134205732013114,
0.957871163454998));
#14543=CARTESIAN_POINT('Ctrl Pts',(-0.0684802489422896,0.139689793109977,
0.956937584580619));
#14544=CARTESIAN_POINT('Ctrl Pts',(-0.066098187521275,0.140832551192719,
0.956733100905458));
#14545=CARTESIAN_POINT('Ctrl Pts',(-0.0636886228436577,0.14191392398309,
0.956529730343417));
#14546=CARTESIAN_POINT('Ctrl Pts',(-0.0636886279045123,0.141913921711862,
0.942835077379979));
#14547=CARTESIAN_POINT('Ctrl Pts',(-0.0651754685424693,0.141246652151541,
0.942961311460843));
#14548=CARTESIAN_POINT('Ctrl Pts',(-0.066652314796618,0.14055579521858,
0.943087417724883));
#14549=CARTESIAN_POINT('Ctrl Pts',(-0.072064565846341,0.137919418819438,
0.943551732415686));
#14550=CARTESIAN_POINT('Ctrl Pts',(-0.0759277422258973,0.135830968303831,
0.943887488150879));
#14551=CARTESIAN_POINT('Ctrl Pts',(-0.0815815806014431,0.132457769055618,
0.944380644775852));
#14552=CARTESIAN_POINT('Ctrl Pts',(-0.0834416230631961,0.131293989808811,
0.944543177869038));
#14553=CARTESIAN_POINT('Ctrl Pts',(-0.0857050585164088,0.129810276820697,
0.944740753488416));
#14554=CARTESIAN_POINT('Ctrl Pts',(-0.086132187189012,0.129527261121152,
0.944778028232698));
#14555=CARTESIAN_POINT('Ctrl Pts',(-0.0868027456224855,0.129078164997774,
0.944836522224598));
#14556=CARTESIAN_POINT('Ctrl Pts',(-0.0870471099441541,0.128913498056301,
0.944857833407518));
#14557=CARTESIAN_POINT('Ctrl Pts',(-0.0875049863599552,0.128603058658927,
0.94489775325352));
#14558=CARTESIAN_POINT('Ctrl Pts',(-0.087718600383088,0.128457450085994,
0.94491637198416));
#14559=CARTESIAN_POINT('Ctrl Pts',(-0.0882078249401503,0.128122184049715,
0.944959002633468));
#14560=CARTESIAN_POINT('Ctrl Pts',(-0.0884831870764194,0.127932169671416,
0.944982990055015));
#14561=CARTESIAN_POINT('Ctrl Pts',(-0.0893360607912009,0.127339570942061,
0.945057270049096));
#14562=CARTESIAN_POINT('Ctrl Pts',(-0.0899114650685197,0.126933945754263,
0.945107361632916));
#14563=CARTESIAN_POINT('Ctrl Pts',(-0.0962832704591434,0.122377140429815,
0.945662048960674));
#14564=CARTESIAN_POINT('Ctrl Pts',(-0.101791385661413,0.11783538614154,
0.946141636405166));
#14565=CARTESIAN_POINT('Ctrl Pts',(-0.11327216640534,0.106960701624341,
0.947190343089342));
#14566=CARTESIAN_POINT('Ctrl Pts',(-0.119064248156573,0.100473284690167,
0.947754939511273));
#14567=CARTESIAN_POINT('Ctrl Pts',(-0.128088442724773,0.0884825577143471,
0.948756471065218));
#14568=CARTESIAN_POINT('Ctrl Pts',(-0.131579780562707,0.0832019109009361,
0.94918528971279));
#14569=CARTESIAN_POINT('Ctrl Pts',(-0.135478504404585,0.0764432028338188,
0.949729402576262));
#14570=CARTESIAN_POINT('Ctrl Pts',(-0.136198940769557,0.0751520903527141,
0.949833123954001));
#14571=CARTESIAN_POINT('Ctrl Pts',(-0.137204603257862,0.0732878481805892,
0.949982670777034));
#14572=CARTESIAN_POINT('Ctrl Pts',(-0.137504882587856,0.072722892465042,
0.950027962413833));
#14573=CARTESIAN_POINT('Ctrl Pts',(-0.138019591791376,0.0717399155998343,
0.950106725343007));
#14574=CARTESIAN_POINT('Ctrl Pts',(-0.138235630771024,0.0713227424108879,
0.950140139493161));
#14575=CARTESIAN_POINT('Ctrl Pts',(-0.138647508029358,0.0705185024513608,
0.950204535318532));
#14576=CARTESIAN_POINT('Ctrl Pts',(-0.138843623797926,0.0701315820039001,
0.950235506885803));
#14577=CARTESIAN_POINT('Ctrl Pts',(-0.139353389066908,0.0691153375162837,
0.950316832390534));
#14578=CARTESIAN_POINT('Ctrl Pts',(-0.139664391166885,0.0684847043821068,
0.950367278017445));
#14579=CARTESIAN_POINT('Ctrl Pts',(-0.140729801554834,0.0662868814749985,
0.950543029360024));
#14580=CARTESIAN_POINT('Ctrl Pts',(-0.141462166834518,0.0647092157217563,
0.950669090923648));
#14581=CARTESIAN_POINT('Ctrl Pts',(-0.146953411502017,0.0523409818694037,
0.95165700755847));
#14582=CARTESIAN_POINT('Ctrl Pts',(-0.150496627030119,0.0410552769420669,
0.952560821658465));
#14583=CARTESIAN_POINT('Ctrl Pts',(-0.154606588493676,0.0197626040760926,
0.95424235999968));
#14584=CARTESIAN_POINT('Ctrl Pts',(-0.155550828322176,0.00988668057949216,
0.955011981534242));
#14585=CARTESIAN_POINT('Ctrl Pts',(-0.155549938049739,-0.000746640964265864,
0.955792014344006));
#14586=CARTESIAN_POINT('Ctrl Pts',(-0.155544686718657,-0.00148026240623606,
0.955845574819193));
#14587=CARTESIAN_POINT('Ctrl Pts',(-0.155529454776193,-0.00255038945730868,
0.955923303393528));
#14588=CARTESIAN_POINT('Ctrl Pts',(-0.155523571979401,-0.00288692811582805,
0.95594769018274));
#14589=CARTESIAN_POINT('Ctrl Pts',(-0.155511220153815,-0.0034828468616109,
0.955990767375515));
#14590=CARTESIAN_POINT('Ctrl Pts',(-0.155505194491466,-0.00374223280619009,
0.956009482205337));
#14591=CARTESIAN_POINT('Ctrl Pts',(-0.155491054726831,-0.004291689999359,
0.956049049889402));
#14592=CARTESIAN_POINT('Ctrl Pts',(-0.155482777959434,-0.00458175347388352,
0.956069893538374));
#14593=CARTESIAN_POINT('Ctrl Pts',(-0.155458275685357,-0.00536369497479437,
0.956125967191308));
#14594=CARTESIAN_POINT('Ctrl Pts',(-0.155440527265389,-0.0058555276371858,
0.956161113328801));
#14595=CARTESIAN_POINT('Ctrl Pts',(-0.155341367983861,-0.00828355785472875,
0.956334046009413));
#14596=CARTESIAN_POINT('Ctrl Pts',(-0.155226109101509,-0.0102183132283127,
0.956470045809172));
#14597=CARTESIAN_POINT('Ctrl Pts',(-0.154790182263663,-0.0157819589500135,
0.95685725921668));
#14598=CARTESIAN_POINT('Ctrl Pts',(-0.154378156275497,-0.0194025735734962,
0.95710449747206));
#14599=CARTESIAN_POINT('Ctrl Pts',(-0.15279598079913,-0.0299826185236076,
0.957821678177203));
#14600=CARTESIAN_POINT('Ctrl Pts',(-0.151279154900507,-0.0368808282153937,
0.958282782973249));
#14601=CARTESIAN_POINT('Ctrl Pts',(-0.146393928955871,-0.053589158847619,
0.959430151307216));
#14602=CARTESIAN_POINT('Ctrl Pts',(-0.142504435665996,-0.0632093065583088,
0.960119472663025));
#14603=CARTESIAN_POINT('Ctrl Pts',(-0.13715870772068,-0.0733797647467837,
0.960923981128279));
#14604=CARTESIAN_POINT('Ctrl Pts',(-0.136617486203173,-0.0743825471406965,
0.961004142971918));
#14605=CARTESIAN_POINT('Ctrl Pts',(-0.135782475356866,-0.0758898051601302,
0.961125953140414));
#14606=CARTESIAN_POINT('Ctrl Pts',(-0.13549677444249,-0.0763987384721141,
0.961167313439395));
#14607=CARTESIAN_POINT('Ctrl Pts',(-0.134979951949463,-0.0773073620862803,
0.961241576296655));
#14608=CARTESIAN_POINT('Ctrl Pts',(-0.134749900974497,-0.0777076562505997,
0.961274440111972));
#14609=CARTESIAN_POINT('Ctrl Pts',(-0.134258285270607,-0.0785543315578226,
0.961344267949642));
#14610=CARTESIAN_POINT('Ctrl Pts',(-0.133996269340237,-0.0790004427915584,
0.961381247987981));
#14611=CARTESIAN_POINT('Ctrl Pts',(-0.13328993072773,-0.0801894392379389,
0.961480318075936));
#14612=CARTESIAN_POINT('Ctrl Pts',(-0.132841629884341,-0.0809299271723088,
0.961542552231131));
#14613=CARTESIAN_POINT('Ctrl Pts',(-0.130641410828768,-0.0844966327945511,
0.961844957377596));
#14614=CARTESIAN_POINT('Ctrl Pts',(-0.128805481071348,-0.0872697202501926,
0.96208819702262));
#14615=CARTESIAN_POINT('Ctrl Pts',(-0.118224401331525,-0.102189993479413,
0.963443850940698));
#14616=CARTESIAN_POINT('Ctrl Pts',(-0.10785057381332,-0.11308354743713,
0.964621104832272));
#14617=CARTESIAN_POINT('Ctrl Pts',(-0.0953028372259867,-0.122939665508869,
0.965843841327429));
#14618=CARTESIAN_POINT('Ctrl Pts',(-0.0945146265885371,-0.123546661509761,
0.965919867220125));
#14619=CARTESIAN_POINT('Ctrl Pts',(-0.0930565935277422,-0.124647363189706,
0.966059004665618));
#14620=CARTESIAN_POINT('Ctrl Pts',(-0.0923885302816992,-0.125143334904367,
0.966122191268034));
#14621=CARTESIAN_POINT('Ctrl Pts',(-0.0891437560344951,-0.127512116654156,
0.96642626333075));
#14622=CARTESIAN_POINT('Ctrl Pts',(-0.0865136716872677,-0.129311010767833,
0.966664220660414));
#14623=CARTESIAN_POINT('Ctrl Pts',(-0.0833702842405818,-0.13132210781512,
0.966937240046204));
#14624=CARTESIAN_POINT('Ctrl Pts',(-0.0829090532376879,-0.131613788070727,
0.96697702066885));
#14625=CARTESIAN_POINT('Ctrl Pts',(-0.0821651622539671,-0.132078758777087,
0.967040720479944));
#14626=CARTESIAN_POINT('Ctrl Pts',(-0.0818834722534007,-0.132253579859319,
0.967064736522244));
#14627=CARTESIAN_POINT('Ctrl Pts',(-0.0813808878923997,-0.132563270049107,
0.9671073953741));
#14628=CARTESIAN_POINT('Ctrl Pts',(-0.0811602138422337,-0.132698489717835,
0.967126060948625));
#14629=CARTESIAN_POINT('Ctrl Pts',(-0.0806888852063093,-0.132985684282409,
0.967165788784842));
#14630=CARTESIAN_POINT('Ctrl Pts',(-0.0804381387799087,-0.133137501303722,
0.96718684072077));
#14631=CARTESIAN_POINT('Ctrl Pts',(-0.0797538940055538,-0.133549145700793,
0.967244065849));
#14632=CARTESIAN_POINT('Ctrl Pts',(-0.0793195508828488,-0.133807573751385,
0.967280149161536));
#14633=CARTESIAN_POINT('Ctrl Pts',(-0.0770726073458707,-0.135129688030806,
0.967465612986509));
#14634=CARTESIAN_POINT('Ctrl Pts',(-0.0752397313942165,-0.136158743334439,
0.967612881071657));
#14635=CARTESIAN_POINT('Ctrl Pts',(-0.069761205089701,-0.139090193404506,
0.968043050445934));
#14636=CARTESIAN_POINT('Ctrl Pts',(-0.0660601664104152,-0.140885654933273,
0.968320844720841));
#14637=CARTESIAN_POINT('Ctrl Pts',(-0.0527289265985237,-0.146711906241544,
0.969292022268375));
#14638=CARTESIAN_POINT('Ctrl Pts',(-0.0427694867708225,-0.149918324311593,
0.969966649056215));
#14639=CARTESIAN_POINT('Ctrl Pts',(-0.0296467473691113,-0.152727770702798,
0.9708646569596));
#14640=CARTESIAN_POINT('Ctrl Pts',(-0.0267124924318142,-0.153268205414237,
0.971065866025252));
#14641=CARTESIAN_POINT('Ctrl Pts',(-0.0201146065116749,-0.154288192067154,
0.971521255039313));
#14642=CARTESIAN_POINT('Ctrl Pts',(-0.0164459180903311,-0.154722240224255,
0.971776500787789));
#14643=CARTESIAN_POINT('Ctrl Pts',(-0.0118419564899607,-0.155101351632126,
0.972100947891838));
#14644=CARTESIAN_POINT('Ctrl Pts',(-0.0109177724930156,-0.155169144449239,
0.972166281098758));
#14645=CARTESIAN_POINT('Ctrl Pts',(-0.00945782179957791,-0.155263130746387,
0.972269836249907));
#14646=CARTESIAN_POINT('Ctrl Pts',(-0.00892241964447542,-0.155294818255313,
0.972307886201858));
#14647=CARTESIAN_POINT('Ctrl Pts',(-0.00793220838357111,-0.155348285765796,
0.972378399363978));
#14648=CARTESIAN_POINT('Ctrl Pts',(-0.00747744529648016,-0.155370839039889,
0.972410838026622));
#14649=CARTESIAN_POINT('Ctrl Pts',(-0.00646789566210372,-0.15541646355692,
0.972482975184194));
#14650=CARTESIAN_POINT('Ctrl Pts',(-0.00591307366941867,-0.155438561379853,
0.972522703668489));
#14651=CARTESIAN_POINT('Ctrl Pts',(-0.00431885141996092,-0.155493509353143,
0.97263710694313));
#14652=CARTESIAN_POINT('Ctrl Pts',(-0.003279242013222,-0.155518906897948,
0.972712013097095));
#14653=CARTESIAN_POINT('Ctrl Pts',(0.00417961038448302,-0.155626304365034,
0.973251706253133));
#14654=CARTESIAN_POINT('Ctrl Pts',(0.0105973077003786,-0.155321251546523,
0.97372849901456));
#14655=CARTESIAN_POINT('Ctrl Pts',(0.0289198148856911,-0.153309478670649,
0.975126461956969));
#14656=CARTESIAN_POINT('Ctrl Pts',(0.04066898390607,-0.150619192295392,
0.976071065891629));
#14657=CARTESIAN_POINT('Ctrl Pts',(0.0561918459608765,-0.145114255809288,
0.977329798968758));
#14658=CARTESIAN_POINT('Ctrl Pts',(0.0603274096331646,-0.143444357283329,
0.977665732262299));
#14659=CARTESIAN_POINT('Ctrl Pts',(0.0649877866080395,-0.141325253149211,
0.978040737765118));
#14660=CARTESIAN_POINT('Ctrl Pts',(0.0655878796580297,-0.141047756699409,
0.978088954821194));
#14661=CARTESIAN_POINT('Ctrl Pts',(0.0664813172160623,-0.140627676187754,
0.978160616839568));
#14662=CARTESIAN_POINT('Ctrl Pts',(0.0667760015370219,-0.140487986934058,
0.978184232828689));
#14663=CARTESIAN_POINT('Ctrl Pts',(0.0673027998977323,-0.140236236604451,
0.978226410944971));
#14664=CARTESIAN_POINT('Ctrl Pts',(0.0675350756757461,-0.140124524934311,
0.97824499413902));
#14665=CARTESIAN_POINT('Ctrl Pts',(0.0680374265608438,-0.139881382953603,
0.978285154038826));
#14666=CARTESIAN_POINT('Ctrl Pts',(0.0683073982668438,-0.139749747964746,
0.978306717777954));
#14667=CARTESIAN_POINT('Ctrl Pts',(0.0690601129544049,-0.13938003091338,
0.978366792196688));
#14668=CARTESIAN_POINT('Ctrl Pts',(0.0695420103728628,-0.139140220766205,
0.978405197345101));
#14669=CARTESIAN_POINT('Ctrl Pts',(0.0723242573724227,-0.137737605389497,
0.978626666634669));
#14670=CARTESIAN_POINT('Ctrl Pts',(0.074596839239336,-0.136520180964435,
0.978806519351657));
#14671=CARTESIAN_POINT('Ctrl Pts',(0.0896386722774296,-0.127974402577677,
0.979997024779159));
#14672=CARTESIAN_POINT('Ctrl Pts',(0.101343105035339,-0.118921083136701,
0.980930233407886));
#14673=CARTESIAN_POINT('Ctrl Pts',(0.112901056904835,-0.107016993056017,
0.982044901681032));
#14674=CARTESIAN_POINT('Ctrl Pts',(0.114176856439393,-0.105654770467335,
0.982170964815923));
#14675=CARTESIAN_POINT('Ctrl Pts',(0.118150500277885,-0.10125591023318,
0.98257408841126));
#14676=CARTESIAN_POINT('Ctrl Pts',(0.120753871774969,-0.0981366272187767,
0.982854192280061));
#14677=CARTESIAN_POINT('Ctrl Pts',(0.123763674068294,-0.0942290535155104,
0.983200453310723));
#14678=CARTESIAN_POINT('Ctrl Pts',(0.124289496702211,-0.0935343920696952,
0.983261836424757));
#14679=CARTESIAN_POINT('Ctrl Pts',(0.125149098781142,-0.0923787283553328,
0.983363692952847));
#14680=CARTESIAN_POINT('Ctrl Pts',(0.125486238194224,-0.0919202392649491,
0.983404035329012));
#14681=CARTESIAN_POINT('Ctrl Pts',(0.126091553489631,-0.0910875106948584,
0.983477191340299));
#14682=CARTESIAN_POINT('Ctrl Pts',(0.1263605996034,-0.0907139092175491,
0.983509970917649));
#14683=CARTESIAN_POINT('Ctrl Pts',(0.126934040150914,-0.0899101199345179,
0.983580409167302));
#14684=CARTESIAN_POINT('Ctrl Pts',(0.127237914153945,-0.0894795697620802,
0.983618087232992));
#14685=CARTESIAN_POINT('Ctrl Pts',(0.128060048929613,-0.0883020549922773,
0.983720997241086));
#14686=CARTESIAN_POINT('Ctrl Pts',(0.128573951065136,-0.0875520878678512,
0.983786393415878));
#14687=CARTESIAN_POINT('Ctrl Pts',(0.131245346144746,-0.0835793202351674,
0.98413208898729));
#14688=CARTESIAN_POINT('Ctrl Pts',(0.133288137551191,-0.0802814491528155,
0.984416618854767));
#14689=CARTESIAN_POINT('Ctrl Pts',(0.14252933799061,-0.064035904474919,
0.985808355921005));
#14690=CARTESIAN_POINT('Ctrl Pts',(0.147975937388227,-0.0501815091361336,
0.986975912152673));
#14691=CARTESIAN_POINT('Ctrl Pts',(0.152402707976014,-0.0314476080578434,
0.988446945003004));
#14692=CARTESIAN_POINT('Ctrl Pts',(0.153238747877481,-0.0270819629670539,
0.988781716040223));
#14693=CARTESIAN_POINT('Ctrl Pts',(0.15398314584966,-0.0220324700510599,
0.989155584208909));
#14694=CARTESIAN_POINT('Ctrl Pts',(0.154075333604147,-0.0213782730607475,
0.989203765396006));
#14695=CARTESIAN_POINT('Ctrl Pts',(0.154206786705354,-0.0204003852691087,
0.989275384691173));
#14696=CARTESIAN_POINT('Ctrl Pts',(0.154249205283681,-0.0200771377385511,
0.989298993531867));
#14697=CARTESIAN_POINT('Ctrl Pts',(0.154323338313836,-0.0194981070605036,
0.989341163950043));
#14698=CARTESIAN_POINT('Ctrl Pts',(0.154355433469979,-0.0192423774284857,
0.98935974656144));
#14699=CARTESIAN_POINT('Ctrl Pts',(0.154423563335354,-0.0186883878346796,
0.989399910974417));
#14700=CARTESIAN_POINT('Ctrl Pts',(0.154459369553669,-0.0183901037053667,
0.989421479783852));
#14701=CARTESIAN_POINT('Ctrl Pts',(0.154556953350991,-0.0175567862331444,
0.989481582609495));
#14702=CARTESIAN_POINT('Ctrl Pts',(0.154616817491248,-0.0170215258944013,
0.989520010932838));
#14703=CARTESIAN_POINT('Ctrl Pts',(0.15494764676042,-0.0139176320546861,
0.989741881549012));
#14704=CARTESIAN_POINT('Ctrl Pts',(0.155157401757367,-0.0113426849930247,
0.989922098789935));
#14705=CARTESIAN_POINT('Ctrl Pts',(0.156132117426485,0.0059307821592932,
0.991112598290918));
#14706=CARTESIAN_POINT('Ctrl Pts',(0.154871822917651,0.0206697883842667,
0.992045555031383));
#14707=CARTESIAN_POINT('Ctrl Pts',(0.151136687573145,0.0368376112444624,
0.993160347712217));
#14708=CARTESIAN_POINT('Ctrl Pts',(0.150682359059377,0.0386540323005574,
0.993286820563852));
#14709=CARTESIAN_POINT('Ctrl Pts',(0.149140586046172,0.0443771436301441,
0.993689915692079));
#14710=CARTESIAN_POINT('Ctrl Pts',(0.147933195110242,0.0482494576948214,
0.993969564796378));
#14711=CARTESIAN_POINT('Ctrl Pts',(0.146284517609919,0.0528904590626598,
0.994315322690666));
#14712=CARTESIAN_POINT('Ctrl Pts',(0.145986147965356,0.0537085216662338,
0.994376674074993));
#14713=CARTESIAN_POINT('Ctrl Pts',(0.145481495854097,0.0550568849639068,
0.994478488818316));
#14714=CARTESIAN_POINT('Ctrl Pts',(0.145279141257644,0.0555886437836925,
0.994518821328992));
#14715=CARTESIAN_POINT('Ctrl Pts',(0.144907777827163,0.0565486549957006,
0.994591966784752));
#14716=CARTESIAN_POINT('Ctrl Pts',(0.144739775587607,0.056977292065568,
0.994624745717515));
#14717=CARTESIAN_POINT('Ctrl Pts',(0.144375354026135,0.0578950556897465,
0.994695190708184));
#14718=CARTESIAN_POINT('Ctrl Pts',(0.144178346979375,0.0583839410553832,
0.994732876194692));
#14719=CARTESIAN_POINT('Ctrl Pts',(0.143634595916026,0.0597137567792696,
0.994835827161011));
#14720=CARTESIAN_POINT('Ctrl Pts',(0.143282959046863,0.060552650430303,
0.994901257093939));
#14721=CARTESIAN_POINT('Ctrl Pts',(0.141390865147565,0.0649578089395814,
0.995247454082914));
#14722=CARTESIAN_POINT('Ctrl Pts',(0.139724702220233,0.0684682137111977,
0.995532466245441));
#14723=CARTESIAN_POINT('Ctrl Pts',(0.131083263538171,0.0850426409293185,
0.996924413983738));
#14724=CARTESIAN_POINT('Ctrl Pts',(0.122397897917246,0.0971271347750815,
0.998091617682632));
#14725=CARTESIAN_POINT('Ctrl Pts',(0.109062425398387,0.110999558059501,
0.999562077214838));
#14726=CARTESIAN_POINT('Ctrl Pts',(0.105849553528857,0.11406750477441,0.999896648026993));
#14727=CARTESIAN_POINT('Ctrl Pts',(0.10201262818374,0.117429393773445,1.00027032021568));
#14728=CARTESIAN_POINT('Ctrl Pts',(0.101513025104336,0.117861548467192,
1.00031849519401));
#14729=CARTESIAN_POINT('Ctrl Pts',(0.100762762552196,0.118502212877876,
1.00039010709367));
#14730=CARTESIAN_POINT('Ctrl Pts',(0.1005141847983,0.118713130839588,1.00041371469671));
#14731=CARTESIAN_POINT('Ctrl Pts',(0.100067896593436,0.119089399183898,
1.00045588378237));
#14732=CARTESIAN_POINT('Ctrl Pts',(0.0998704374891159,0.119255040337439,
1.00047446629319));
#14733=CARTESIAN_POINT('Ctrl Pts',(0.0994419110524191,0.119612704537383,
1.0005146314889));
#14734=CARTESIAN_POINT('Ctrl Pts',(0.0992106994597293,0.119804548650624,
1.00053620117724));
#14735=CARTESIAN_POINT('Ctrl Pts',(0.0985634083727691,0.12033846917419,
1.00059630892742));
#14736=CARTESIAN_POINT('Ctrl Pts',(0.0981461002175099,0.120679060604004,
1.00063474126835));
#14737=CARTESIAN_POINT('Ctrl Pts',(0.0957168351372661,0.122640800646394,
1.00085668155352));
#14738=CARTESIAN_POINT('Ctrl Pts',(0.0936663525049465,0.12421390834673,
1.00103696207699));
#14739=CARTESIAN_POINT('Ctrl Pts',(0.0796813794627272,0.134399657797159,
1.00222746062012));
#14740=CARTESIAN_POINT('Ctrl Pts',(0.066614805334272,0.141332824680005,
1.00316037368355));
#14741=CARTESIAN_POINT('Ctrl Pts',(0.0510047975938716,0.146961976327272,
1.00427518840198));
#14742=CARTESIAN_POINT('Ctrl Pts',(0.0492312643835637,0.147565558590524,
1.00440173276362));
#14743=CARTESIAN_POINT('Ctrl Pts',(0.0435867099227604,0.149373473060959,
1.0048048229761));
#14744=CARTESIAN_POINT('Ctrl Pts',(0.0396795691273101,0.150458508016175,
1.00508439276004));
#14745=CARTESIAN_POINT('Ctrl Pts',(0.0348873772864512,0.15158968144272,
1.0054300628959));
#14746=CARTESIAN_POINT('Ctrl Pts',(0.0340383188044144,0.151782585996964,
1.00549140874169));
#14747=CARTESIAN_POINT('Ctrl Pts',(0.0326318634008249,0.15208973561969,
1.00559321619123));
#14748=CARTESIAN_POINT('Ctrl Pts',(0.0320753711090026,0.152208070556371,
1.00563354697973));
#14749=CARTESIAN_POINT('Ctrl Pts',(0.0310674131024543,0.152416633928575,
1.00570669059324));
#14750=CARTESIAN_POINT('Ctrl Pts',(0.0306161699791301,0.152507916458299,
1.00573946941385));
#14751=CARTESIAN_POINT('Ctrl Pts',(0.0301633266312624,0.152597431918257,
1.00577239994307));
#14752=CARTESIAN_POINT('Ctrl Pts',(0.0301621205796583,0.152597670308719,
1.00577248764676));
#14753=CARTESIAN_POINT('Ctrl Pts',(0.0301597155018312,0.152598145671376,
1.00577266254375));
#14754=CARTESIAN_POINT('Ctrl Pts',(0.0301585162608852,0.152598382686173,
1.00577274975267));
#14755=CARTESIAN_POINT('Ctrl Pts',(0.0301561244804412,0.152598855362015,
1.00577292368367));
#14756=CARTESIAN_POINT('Ctrl Pts',(0.0301549319303764,0.152599091025312,
1.00577301040653));
#14757=CARTESIAN_POINT('Ctrl Pts',(0.0301525534617249,0.15259956101247,
1.00577318337048));
#14758=CARTESIAN_POINT('Ctrl Pts',(0.0301513675411587,0.152599795336883,
1.00577326961171));
#14759=CARTESIAN_POINT('Ctrl Pts',(0.0301490022977461,0.152600262653427,
1.00577344161489));
#14760=CARTESIAN_POINT('Ctrl Pts',(0.0301478229596279,0.152600495648734,
1.00577352737793));
#14761=CARTESIAN_POINT('Ctrl Pts',(0.0301454708219992,0.152600960319221,
1.005773698429));
#14762=CARTESIAN_POINT('Ctrl Pts',(0.0301442980134178,0.15260119199635,
1.00577378371768));
#14763=CARTESIAN_POINT('Ctrl Pts',(0.0301419588697503,0.152601654043811,
1.00577395382475));
#14764=CARTESIAN_POINT('Ctrl Pts',(0.0301407925320586,0.152601884414814,
1.00577403864334));
#14765=CARTESIAN_POINT('Ctrl Pts',(0.0301384662985743,0.152602343856728,
1.0057742078125));
#14766=CARTESIAN_POINT('Ctrl Pts',(0.0301373063880749,0.152602572930696,
1.00577429216415));
#14767=CARTESIAN_POINT('Ctrl Pts',(0.0301349929385682,0.152603029792905,
1.00577446040456));
#14768=CARTESIAN_POINT('Ctrl Pts',(0.0301338393974747,0.152603257581708,
1.00577454429347));
#14769=CARTESIAN_POINT('Ctrl Pts',(0.0301315386429228,0.152603711882696,
1.0057747116116));
#14770=CARTESIAN_POINT('Ctrl Pts',(0.0301303914208618,0.152603938396728,
1.00577479504143));
#14771=CARTESIAN_POINT('Ctrl Pts',(0.0296182384711124,0.152705054780455,
1.00581204062154));
#14772=CARTESIAN_POINT('Ctrl Pts',(0.0291067350185148,0.152803376173466,
1.00584928425823));
#14773=CARTESIAN_POINT('Ctrl Pts',(0.0277248485209288,0.1530618125971,1.00595002994691));
#14774=CARTESIAN_POINT('Ctrl Pts',(0.0268535885034833,0.15321706962793,
1.00601368517867));
#14775=CARTESIAN_POINT('Ctrl Pts',(0.0249153348461428,0.153545423153314,
1.00615561810144));
#14776=CARTESIAN_POINT('Ctrl Pts',(0.0238477748976303,0.153714847703908,
1.00623400855744));
#14777=CARTESIAN_POINT('Ctrl Pts',(0.020598848896711,0.154195801449675,
1.00647326815107));
#14778=CARTESIAN_POINT('Ctrl Pts',(0.0184126347732405,0.15447210664942,
1.00663521659951));
#14779=CARTESIAN_POINT('Ctrl Pts',(0.00128168582482278,0.156268386009311,
1.00791204814532));
#14780=CARTESIAN_POINT('Ctrl Pts',(-0.0138047606114468,0.155662166319765,
1.00909405839476));
#14781=CARTESIAN_POINT('Ctrl Pts',(-0.0293488402462114,0.1527582513758,
1.01030532816512));
#14782=CARTESIAN_POINT('Ctrl Pts',(-0.0301312089151297,0.152605858579218,
1.01036624553402));
#14783=CARTESIAN_POINT('Ctrl Pts',(-0.0320990556092688,0.152206830408436,
1.01051929652536));
#14784=CARTESIAN_POINT('Ctrl Pts',(-0.0332829103453998,0.151952349857471,
1.01061121519526));
#14785=CARTESIAN_POINT('Ctrl Pts',(-0.0373399433792838,0.151030562971816,
1.0109254352568));
#14786=CARTESIAN_POINT('Ctrl Pts',(-0.0401972737794545,0.150295324446178,
1.01114539025543));
#14787=CARTESIAN_POINT('Ctrl Pts',(-0.0435447708229174,0.149331644117594,
1.01140017135279));
#14788=CARTESIAN_POINT('Ctrl Pts',(-0.0440565877785823,0.149181446890677,
1.01143904484155));
#14789=CARTESIAN_POINT('Ctrl Pts',(-0.0448851285912375,0.148933668291434,
1.01150183086639));
#14790=CARTESIAN_POINT('Ctrl Pts',(-0.0452023250601255,0.148837704007131,
1.01152583355143));
#14791=CARTESIAN_POINT('Ctrl Pts',(-0.0457661109998347,0.148665168246601,
1.01156843220941));
#14792=CARTESIAN_POINT('Ctrl Pts',(-0.0460128181847806,0.148588996000174,
1.01158705102834));
#14793=CARTESIAN_POINT('Ctrl Pts',(-0.0465426001212743,0.148423976818807,
1.01162698557786));
#14794=CARTESIAN_POINT('Ctrl Pts',(-0.0468256099792224,0.148334934438409,
1.01164828966424));
#14795=CARTESIAN_POINT('Ctrl Pts',(-0.0475954101592194,0.148090312299131,
1.01170616329803));
#14796=CARTESIAN_POINT('Ctrl Pts',(-0.0480816972259792,0.147933140562169,
1.01174264114639));
#14797=CARTESIAN_POINT('Ctrl Pts',(-0.0506542848038794,0.147087634838227,
1.01193523195263));
#14798=CARTESIAN_POINT('Ctrl Pts',(-0.052726738744623,0.146357511749173,
1.01208903112382));
#14799=CARTESIAN_POINT('Ctrl Pts',(-0.0577889011771071,0.144452618949119,
1.01246299068799));
#14800=CARTESIAN_POINT('Ctrl Pts',(-0.0607588120708827,0.14322877469962,
1.01268089937769));
#14801=CARTESIAN_POINT('Ctrl Pts',(-0.063688626060837,0.141913922539273,
1.01289638536134));
#14802=CARTESIAN_POINT('Origin',(0.,0.,-0.129405622560373));
#14803=CARTESIAN_POINT('',(-0.0636886243720526,0.141913923297172,1.09662690323003));
#14804=CARTESIAN_POINT('',(-0.0636886366175018,0.141913917801616,1.08266645291));
#14805=CARTESIAN_POINT('',(-0.0636886258329924,0.141913922641526,-0.129405622560373));
#14806=CARTESIAN_POINT('Ctrl Pts',(-0.0636886243721051,0.141913923297148,
1.09662690323004));
#14807=CARTESIAN_POINT('Ctrl Pts',(-0.0606910358173481,0.143259191520664,
1.09641019358287));
#14808=CARTESIAN_POINT('Ctrl Pts',(-0.0576487518881258,0.144510416255214,
1.09619253612461));
#14809=CARTESIAN_POINT('Ctrl Pts',(-0.0487306005434893,0.147851148303692,
1.09555661654928));
#14810=CARTESIAN_POINT('Ctrl Pts',(-0.0427697403818496,0.149684226985495,
1.09513391348564));
#14811=CARTESIAN_POINT('Ctrl Pts',(-0.0352901438448625,0.151501022618486,
1.09459708320992));
#14812=CARTESIAN_POINT('Ctrl Pts',(-0.0338599732463984,0.151827059712076,
1.09449416940812));
#14813=CARTESIAN_POINT('Ctrl Pts',(-0.0318015728751101,0.152265785270025,
1.09434557360214));
#14814=CARTESIAN_POINT('Ctrl Pts',(-0.031176894660229,0.152394916643116,
1.09430041584057));
#14815=CARTESIAN_POINT('Ctrl Pts',(-0.0300910129164921,0.15261243051825,
1.09422180185109));
#14816=CARTESIAN_POINT('Ctrl Pts',(-0.0296301670539519,0.152702574302262,
1.09418840209104));
#14817=CARTESIAN_POINT('Ctrl Pts',(-0.0287422018335271,0.152872093799484,
1.09412397412506));
#14818=CARTESIAN_POINT('Ctrl Pts',(-0.028315143627443,0.152951769728825,
1.09409295579902));
#14819=CARTESIAN_POINT('Ctrl Pts',(-0.0271931157132175,0.15315624543371,
1.09401137203812));
#14820=CARTESIAN_POINT('Ctrl Pts',(-0.0264976271319612,0.153278102752604,
1.09396071384157));
#14821=CARTESIAN_POINT('Ctrl Pts',(-0.0240698801550837,0.153686454030928,
1.09378355623299));
#14822=CARTESIAN_POINT('Ctrl Pts',(-0.0223336788795188,0.153948340690714,
1.0936562850526));
#14823=CARTESIAN_POINT('Ctrl Pts',(-0.00984123617193006,0.155616920212879,
1.09273602087342));
#14824=CARTESIAN_POINT('Ctrl Pts',(0.00102956083148582,0.155924103007786,
1.09190809851299));
#14825=CARTESIAN_POINT('Ctrl Pts',(0.0179309100360783,0.154633695595715,
1.09059497342993));
#14826=CARTESIAN_POINT('Ctrl Pts',(0.0239876154017345,0.153810583154407,
1.09011986125403));
#14827=CARTESIAN_POINT('Ctrl Pts',(0.0332290777608797,0.151995368933204,
1.08939855476949));
#14828=CARTESIAN_POINT('Ctrl Pts',(0.0364568356744049,0.151253648520396,
1.08914738422744));
#14829=CARTESIAN_POINT('Ctrl Pts',(0.0408257540884962,0.150101689040192,
1.08881044914836));
#14830=CARTESIAN_POINT('Ctrl Pts',(0.0419892496499482,0.14978038051122,
1.08872101926153));
#14831=CARTESIAN_POINT('Ctrl Pts',(0.0437178039215849,0.1492813006192,1.08858872034962));
#14832=CARTESIAN_POINT('Ctrl Pts',(0.0442857464431731,0.149113801458605,
1.08854534280673));
#14833=CARTESIAN_POINT('Ctrl Pts',(0.0453102739715165,0.148805275119575,
1.0884672748202));
#14834=CARTESIAN_POINT('Ctrl Pts',(0.0457671884065209,0.148665380342434,
1.08843252409074));
#14835=CARTESIAN_POINT('Ctrl Pts',(0.0464838097112746,0.148442353398558,
1.08837813240717));
#14836=CARTESIAN_POINT('Ctrl Pts',(0.0467439496842704,0.148360641744423,
1.08835841080417));
#14837=CARTESIAN_POINT('Ctrl Pts',(0.0472496306887385,0.148200341983529,
1.08832012108284));
#14838=CARTESIAN_POINT('Ctrl Pts',(0.0474951885219765,0.148121828348726,
1.08830154941273));
#14839=CARTESIAN_POINT('Ctrl Pts',(0.0480507510872503,0.147942671488438,
1.08825958021533));
#14840=CARTESIAN_POINT('Ctrl Pts',(0.0483606348011116,0.147841664405186,
1.08823620432213));
#14841=CARTESIAN_POINT('Ctrl Pts',(0.0492969520476,0.147533211393719,1.08816566965565));
#14842=CARTESIAN_POINT('Ctrl Pts',(0.0499223962295122,0.147322748893458,
1.08811868373729));
#14843=CARTESIAN_POINT('Ctrl Pts',(0.0547219064225555,0.145673634499721,
1.08775898813051));
#14844=CARTESIAN_POINT('Ctrl Pts',(0.0588348417975893,0.144061671967499,
1.08745576702389));
#14845=CARTESIAN_POINT('Ctrl Pts',(0.0763913558360544,0.136303202843618,
1.08616036458814));
#14846=CARTESIAN_POINT('Ctrl Pts',(0.0889885014990023,0.128434020690596,
1.08522070187036));
#14847=CARTESIAN_POINT('Ctrl Pts',(0.103291450140318,0.116370662134439,
1.08394619738253));
#14848=CARTESIAN_POINT('Ctrl Pts',(0.106198923090093,0.113723519562871,
1.08367473356972));
#14849=CARTESIAN_POINT('Ctrl Pts',(0.109654247928001,0.110329425742178,
1.08333443202295));
#14850=CARTESIAN_POINT('Ctrl Pts',(0.110300001892403,0.109683844718726,
1.08327003373154));
#14851=CARTESIAN_POINT('Ctrl Pts',(0.111310099622651,0.108656076544217,
1.08316800385142));
#14852=CARTESIAN_POINT('Ctrl Pts',(0.111678253091648,0.108277647840552,
1.08313053947914));
#14853=CARTESIAN_POINT('Ctrl Pts',(0.112363873283518,0.107565675344448,
1.08306024238957));
#14854=CARTESIAN_POINT('Ctrl Pts',(0.112681800248584,0.107232580944171,
1.08302743012615));
#14855=CARTESIAN_POINT('Ctrl Pts',(0.113388711572908,0.106485329604507,
1.08295398606815));
#14856=CARTESIAN_POINT('Ctrl Pts',(0.113776913415572,0.106070444945475,
1.08291332135019));
#14857=CARTESIAN_POINT('Ctrl Pts',(0.114752364388992,0.105016430667634,
1.0828102888986));
#14858=CARTESIAN_POINT('Ctrl Pts',(0.115336546583136,0.104374502674475,
1.08274779255658));
#14859=CARTESIAN_POINT('Ctrl Pts',(0.118589858393052,0.100738940043217,
1.08239521443387));
#14860=CARTESIAN_POINT('Ctrl Pts',(0.121147556661058,0.0976481059500292,
1.08210057196515));
#14861=CARTESIAN_POINT('Ctrl Pts',(0.124743587952362,0.092943496655078,
1.08165888842169));
#14862=CARTESIAN_POINT('Ctrl Pts',(0.125876260641376,0.0914036256625607,
1.08151534591618));
#14863=CARTESIAN_POINT('Ctrl Pts',(0.13548016295333,0.0778299329645663,
1.08025903975177));
#14864=CARTESIAN_POINT('Ctrl Pts',(0.142231095549923,0.0646731057569159,
1.07909202409414));
#14865=CARTESIAN_POINT('Ctrl Pts',(0.147880404653027,0.0483107645352777,
1.07778978239498));
#14866=CARTESIAN_POINT('Ctrl Pts',(0.148666263755362,0.0458354472663105,
1.07759679249956));
#14867=CARTESIAN_POINT('Ctrl Pts',(0.1495401688619,0.0428232587818683,1.07736767329061));
#14868=CARTESIAN_POINT('Ctrl Pts',(0.149687806861027,0.0423043035196591,
1.07732840285649));
#14869=CARTESIAN_POINT('Ctrl Pts',(0.149913516779106,0.0414949442716691,
1.07726748432112));
#14870=CARTESIAN_POINT('Ctrl Pts',(0.149993449921502,0.041205071265812,
1.07724573146733));
#14871=CARTESIAN_POINT('Ctrl Pts',(0.15014035435182,0.0406662385563369,
1.07720541930946));
#14872=CARTESIAN_POINT('Ctrl Pts',(0.150207546605777,0.0404173466191966,
1.07718684777061));
#14873=CARTESIAN_POINT('Ctrl Pts',(0.150358279277258,0.0398534385236162,
1.07714488065014));
#14874=CARTESIAN_POINT('Ctrl Pts',(0.150441448511972,0.0395383267763001,
1.07712150669359));
#14875=CARTESIAN_POINT('Ctrl Pts',(0.150689987245872,0.0385845242215516,
1.07705098364594));
#14876=CARTESIAN_POINT('Ctrl Pts',(0.150852287229712,0.0379450292475615,
1.07700400732597));
#14877=CARTESIAN_POINT('Ctrl Pts',(0.152068354326881,0.0330223284250973,
1.07664461155035));
#14878=CARTESIAN_POINT('Ctrl Pts',(0.152943695199273,0.0286965807532526,
1.07634166281779));
#14879=CARTESIAN_POINT('Ctrl Pts',(0.155520071892186,0.0124338223857224,
1.07523038589395));
#14880=CARTESIAN_POINT('Ctrl Pts',(0.156016042365109,0.00034937246958913,
1.07445655448604));
#14881=CARTESIAN_POINT('Ctrl Pts',(0.154791477433783,-0.0159244915900999,
1.07336407318295));
#14882=CARTESIAN_POINT('Ctrl Pts',(0.154296729050599,-0.0201619837809552,
1.07307529362274));
#14883=CARTESIAN_POINT('Ctrl Pts',(0.15321980489979,-0.0269499301488922,
1.07260168214296));
#14884=CARTESIAN_POINT('Ctrl Pts',(0.152746332292334,-0.0295154862350913,
1.07242011852912));
#14885=CARTESIAN_POINT('Ctrl Pts',(0.152044447913902,-0.0328469539985112,
1.07218046013581));
#14886=CARTESIAN_POINT('Ctrl Pts',(0.151874315636641,-0.0336248232116175,
1.072124223568));
#14887=CARTESIAN_POINT('Ctrl Pts',(0.151587175255337,-0.034891014769014,
1.07203221349378));
#14888=CARTESIAN_POINT('Ctrl Pts',(0.151473760009997,-0.0353801445893342,
1.07199655522128));
#14889=CARTESIAN_POINT('Ctrl Pts',(0.151250578989105,-0.0363219188264252,
1.07192767294409));
#14890=CARTESIAN_POINT('Ctrl Pts',(0.151141144320495,-0.0367746368654985,
1.07189445990069));
#14891=CARTESIAN_POINT('Ctrl Pts',(0.150885170755583,-0.0378131239575834,
1.0718180373986));
#14892=CARTESIAN_POINT('Ctrl Pts',(0.1507372517929,-0.0383985416424383,
1.07177478395101));
#14893=CARTESIAN_POINT('Ctrl Pts',(0.150333548822834,-0.0399579872764489,
1.07165909588471));
#14894=CARTESIAN_POINT('Ctrl Pts',(0.150071711740404,-0.0409304030697252,
1.07158646715413));
#14895=CARTESIAN_POINT('Ctrl Pts',(0.147918322892713,-0.0486291427657746,
1.07100746526774));
#14896=CARTESIAN_POINT('Ctrl Pts',(0.145585250760267,-0.0552225589933986,
1.07048676710374));
#14897=CARTESIAN_POINT('Ctrl Pts',(0.138752403217296,-0.0710550084938144,
1.06917379951877));
#14898=CARTESIAN_POINT('Ctrl Pts',(0.133765686062294,-0.0800484779595857,
1.06837052268306));
#14899=CARTESIAN_POINT('Ctrl Pts',(0.125770847161814,-0.0916073867786282,
1.06729026894513));
#14900=CARTESIAN_POINT('Ctrl Pts',(0.123497161338834,-0.0946502772148985,
1.06700107517324));
#14901=CARTESIAN_POINT('Ctrl Pts',(0.119863541997304,-0.0991589950937276,
1.06656832044312));
#14902=CARTESIAN_POINT('Ctrl Pts',(0.118583074845973,-0.100686793531841,
1.06642089617918));
#14903=CARTESIAN_POINT('Ctrl Pts',(0.116947108837644,-0.102564238848323,
1.06623917283221));
#14904=CARTESIAN_POINT('Ctrl Pts',(0.116618903470063,-0.102937265981192,
1.06620303824192));
#14905=CARTESIAN_POINT('Ctrl Pts',(0.11609545490084,-0.103526483069429,
1.06614592551476));
#14906=CARTESIAN_POINT('Ctrl Pts',(0.115901385961924,-0.103743703815122,
1.06612486247855));
#14907=CARTESIAN_POINT('Ctrl Pts',(0.1155334025084,-0.104153265159255,1.06608513617389));
#14908=CARTESIAN_POINT('Ctrl Pts',(0.115359619451581,-0.104345713566927,
1.06606646413134));
#14909=CARTESIAN_POINT('Ctrl Pts',(0.114960275617218,-0.104785732302075,
1.06602375862612));
#14910=CARTESIAN_POINT('Ctrl Pts',(0.114734396013438,-0.105033009293303,
1.06599974955649));
#14911=CARTESIAN_POINT('Ctrl Pts',(0.114130725738578,-0.10568959359255,
1.06593596655915));
#14912=CARTESIAN_POINT('Ctrl Pts',(0.113751527524001,-0.106097609597714,
1.06589629631628));
#14913=CARTESIAN_POINT('Ctrl Pts',(0.111032829077625,-0.108991589265561,
1.06561460110371));
#14914=CARTESIAN_POINT('Ctrl Pts',(0.108614020427173,-0.111402220634307,
1.06537824634035));
#14915=CARTESIAN_POINT('Ctrl Pts',(0.102257363715481,-0.11733332244437,
1.06478590157066));
#14916=CARTESIAN_POINT('Ctrl Pts',(0.0982159520673129,-0.120736539660136,
1.06443543904685));
#14917=CARTESIAN_POINT('Ctrl Pts',(0.0875729060468159,-0.128810126936401,
1.06355393235674));
#14918=CARTESIAN_POINT('Ctrl Pts',(0.0807665015236307,-0.133183442397176,
1.06302648001027));
#14919=CARTESIAN_POINT('Ctrl Pts',(0.0700365598773572,-0.138951523080993,
1.06220985634516));
#14920=CARTESIAN_POINT('Ctrl Pts',(0.0663465139486922,-0.140750777184016,
1.06193159544409));
#14921=CARTESIAN_POINT('Ctrl Pts',(0.0602671256429053,-0.143422848512658,
1.06147366750183));
#14922=CARTESIAN_POINT('Ctrl Pts',(0.0579198746834443,-0.144386726332588,
1.06129699407416));
#14923=CARTESIAN_POINT('Ctrl Pts',(0.0548138787475647,-0.145574251307052,
1.06106288825577));
#14924=CARTESIAN_POINT('Ctrl Pts',(0.0540754259205835,-0.145850170440064,
1.06100720668279));
#14925=CARTESIAN_POINT('Ctrl Pts',(0.052864892295059,-0.146292023098675,
1.06091587688621));
#14926=CARTESIAN_POINT('Ctrl Pts',(0.0523940448716134,-0.146461315407852,
1.06088034064395));
#14927=CARTESIAN_POINT('Ctrl Pts',(0.0514827469776956,-0.146784014082325,
1.06081153369587));
#14928=CARTESIAN_POINT('Ctrl Pts',(0.0510424066282559,-0.146937717225271,
1.06077827324443));
#14929=CARTESIAN_POINT('Ctrl Pts',(0.0500265810100475,-0.147287179332254,
1.0607015112467));
#14930=CARTESIAN_POINT('Ctrl Pts',(0.0494506294451958,-0.147481548782424,
1.06065796441789));
#14931=CARTESIAN_POINT('Ctrl Pts',(0.0479043451970216,-0.147993305538292,
1.06054097860186));
#14932=CARTESIAN_POINT('Ctrl Pts',(0.0469320170991188,-0.148304519322536,
1.06046733856679));
#14933=CARTESIAN_POINT('Ctrl Pts',(0.0387145581156659,-0.150845783481167,
1.05984422857643));
#14934=CARTESIAN_POINT('Ctrl Pts',(0.031319620478302,-0.152552659921158,
1.05927779558591));
#14935=CARTESIAN_POINT('Ctrl Pts',(0.0141675525319759,-0.155211810083501,
1.05795196677633));
#14936=CARTESIAN_POINT('Ctrl Pts',(0.00438468218431797,-0.155795321765404,
1.05718646470351));
#14937=CARTESIAN_POINT('Ctrl Pts',(-0.00908359376598436,-0.155328587943792,
1.05615132862355));
#14938=CARTESIAN_POINT('Ctrl Pts',(-0.0127744985669397,-0.155068689149605,
1.05586984441875));
#14939=CARTESIAN_POINT('Ctrl Pts',(-0.0184000582917418,-0.154470303649111,
1.05544723229978));
#14940=CARTESIAN_POINT('Ctrl Pts',(-0.0203432661095739,-0.154226422353404,
1.05530243735466));
#14941=CARTESIAN_POINT('Ctrl Pts',(-0.0227703244371664,-0.153875140326209,
1.05512349078963));
#14942=CARTESIAN_POINT('Ctrl Pts',(-0.023258848588846,-0.153802056116356,
1.05508756894396));
#14943=CARTESIAN_POINT('Ctrl Pts',(-0.0240342566423214,-0.153682274443948,
1.05503071492794));
#14944=CARTESIAN_POINT('Ctrl Pts',(-0.0243213663826324,-0.153637098747953,
1.05500969914258));
#14945=CARTESIAN_POINT('Ctrl Pts',(-0.0248645376653519,-0.153550071908389,
1.05497000959026));
#14946=CARTESIAN_POINT('Ctrl Pts',(-0.0251206178240656,-0.153508385366391,
1.05495132729294));
#14947=CARTESIAN_POINT('Ctrl Pts',(-0.0257081412498728,-0.153411234594297,
1.05490853065624));
#14948=CARTESIAN_POINT('Ctrl Pts',(-0.0260395099131109,-0.153355336899367,
1.0548844410755));
#14949=CARTESIAN_POINT('Ctrl Pts',(-0.0269234538962342,-0.153203279043141,
1.05482030293648));
#14950=CARTESIAN_POINT('Ctrl Pts',(-0.0274757016220419,-0.153105202149349,
1.05478035989851));
#14951=CARTESIAN_POINT('Ctrl Pts',(-0.0314650975034128,-0.152374421485862,
1.05449265718641));
#14952=CARTESIAN_POINT('Ctrl Pts',(-0.03488092383369,-0.151628963823294,
1.05425084321478));
#14953=CARTESIAN_POINT('Ctrl Pts',(-0.0433137369418515,-0.149488498295355,
1.05365857132373));
#14954=CARTESIAN_POINT('Ctrl Pts',(-0.0482913525893562,-0.147955547414858,
1.05331313684806));
#14955=CARTESIAN_POINT('Ctrl Pts',(-0.0607702538684128,-0.143415356197325,
1.0524369138624));
#14956=CARTESIAN_POINT('Ctrl Pts',(-0.0681307305130796,-0.140068504963997,
1.05190974114082));
#14957=CARTESIAN_POINT('Ctrl Pts',(-0.080612022054574,-0.133175654673393,
1.05095390104198));
#14958=CARTESIAN_POINT('Ctrl Pts',(-0.0858422056327382,-0.129865904897493,
1.05053207977654));
#14959=CARTESIAN_POINT('Ctrl Pts',(-0.091698278722626,-0.125651470789151,
1.05002604385517));
#14960=CARTESIAN_POINT('Ctrl Pts',(-0.0925294520410273,-0.125040660770912,
1.04995339073812));
#14961=CARTESIAN_POINT('Ctrl Pts',(-0.0937972728805838,-0.124089405488513,
1.04984125333863));
#14962=CARTESIAN_POINT('Ctrl Pts',(-0.0942382920711193,-0.123754811007321,
1.04980199703721));
#14963=CARTESIAN_POINT('Ctrl Pts',(-0.095038840145718,-0.123140686838785,
1.04973027781843));
#14964=CARTESIAN_POINT('Ctrl Pts',(-0.0953989470330005,-0.122861917567147,
1.04969784508377));
#14965=CARTESIAN_POINT('Ctrl Pts',(-0.0961819073568622,-0.122250287512484,
1.04962694949502));
#14966=CARTESIAN_POINT('Ctrl Pts',(-0.0966042666007759,-0.121916806719874,
1.04958846229534));
#14967=CARTESIAN_POINT('Ctrl Pts',(-0.09775496451879,-0.120998520172192,
1.04948293112828));
#14968=CARTESIAN_POINT('Ctrl Pts',(-0.0984797691577612,-0.12040934335774,
1.04941571275575));
#14969=CARTESIAN_POINT('Ctrl Pts',(-0.102109763473829,-0.11740390569505,
1.04907522485682));
#14970=CARTESIAN_POINT('Ctrl Pts',(-0.104931287377558,-0.114889082188782,
1.04879796829395));
#14971=CARTESIAN_POINT('Ctrl Pts',(-0.10919103813286,-0.110804464448972,
1.04835861563113));
#14972=CARTESIAN_POINT('Ctrl Pts',(-0.110693499877065,-0.10930352466307,
1.04819931522705));
#14973=CARTESIAN_POINT('Ctrl Pts',(-0.122272958236273,-0.0972521362867354,
1.04693699596424));
#14974=CARTESIAN_POINT('Ctrl Pts',(-0.130849422265921,-0.0853639515742955,
1.04578074713185));
#14975=CARTESIAN_POINT('Ctrl Pts',(-0.138929417834625,-0.070014527411993,
1.04447366457841));
#14976=CARTESIAN_POINT('Ctrl Pts',(-0.140149706544214,-0.0675387259033696,
1.04426830095686));
#14977=CARTESIAN_POINT('Ctrl Pts',(-0.141533135571074,-0.0645327479449565,
1.04402651454286));
#14978=CARTESIAN_POINT('Ctrl Pts',(-0.141760066509343,-0.0640327071862858,
1.04398654020616));
#14979=CARTESIAN_POINT('Ctrl Pts',(-0.142108010454061,-0.0632550988868648,
1.04392476972932));
#14980=CARTESIAN_POINT('Ctrl Pts',(-0.142230865920963,-0.0629783689376224,
1.04390286414137));
#14981=CARTESIAN_POINT('Ctrl Pts',(-0.142456758298112,-0.0624655175453418,
1.04386241192416));
#14982=CARTESIAN_POINT('Ctrl Pts',(-0.142560015706833,-0.0622295009676079,
1.0438438523141));
#14983=CARTESIAN_POINT('Ctrl Pts',(-0.1427914799433,-0.0616968409654128,
1.04380209238037));
#14984=CARTESIAN_POINT('Ctrl Pts',(-0.142919348705197,-0.0614000545629998,
1.04377891277425));
#14985=CARTESIAN_POINT('Ctrl Pts',(-0.14324511842001,-0.0606374037818408,
1.04371956859916));
#14986=CARTESIAN_POINT('Ctrl Pts',(-0.143441674222118,-0.060170963128615,
1.04368348379786));
#14987=CARTESIAN_POINT('Ctrl Pts',(-0.144593446739929,-0.0574000071597424,
1.04347031321858));
#14988=CARTESIAN_POINT('Ctrl Pts',(-0.145495460382989,-0.0550735741235107,
1.04329623015511));
#14989=CARTESIAN_POINT('Ctrl Pts',(-0.150654583141779,-0.0407544870207453,
1.04224836769704));
#14990=CARTESIAN_POINT('Ctrl Pts',(-0.153483136687386,-0.0282973266317507,
1.04143322562587));
#14991=CARTESIAN_POINT('Ctrl Pts',(-0.155285119331868,-0.0104587456189201,
1.04024137622979));
#14992=CARTESIAN_POINT('Ctrl Pts',(-0.155547943927636,-0.00526147652008941,
1.03989176974618));
#14993=CARTESIAN_POINT('Ctrl Pts',(-0.155550304046007,0.00074293371199677,
1.03947950815874));
#14994=CARTESIAN_POINT('Ctrl Pts',(-0.155544385392344,0.00154698563916683,
1.03942413272929));
#14995=CARTESIAN_POINT('Ctrl Pts',(-0.155519543941367,0.00319043249726224,
1.03931057288901));
#14996=CARTESIAN_POINT('Ctrl Pts',(-0.155500058275444,0.0040297938030437,
1.03925237420997));
#14997=CARTESIAN_POINT('Ctrl Pts',(-0.155421679500313,0.00653256384603913,
1.03907819969411));
#14998=CARTESIAN_POINT('Ctrl Pts',(-0.155342883500902,0.00819518279790847,
1.0389616482437));
#14999=CARTESIAN_POINT('Ctrl Pts',(-0.155193655213519,0.0105455716828021,
1.03879554745463));
#15000=CARTESIAN_POINT('Ctrl Pts',(-0.155145292663299,0.0112346712151309,
1.03874668659369));
#15001=CARTESIAN_POINT('Ctrl Pts',(-0.155059257330732,0.0123537650580931,
1.03866706293629));
#15002=CARTESIAN_POINT('Ctrl Pts',(-0.155024381570459,0.012783970701975,
1.03863638792337));
#15003=CARTESIAN_POINT('Ctrl Pts',(-0.154947636149121,0.0136841203952315,
1.03857206381552));
#15004=CARTESIAN_POINT('Ctrl Pts',(-0.154905418043876,0.0141540294905362,
1.03853840411779));
#15005=CARTESIAN_POINT('Ctrl Pts',(-0.154799912420558,0.0152713031239057,
1.03845817866608));
#15006=CARTESIAN_POINT('Ctrl Pts',(-0.154734701321405,0.0159184725298402,
1.03841155307539));
#15007=CARTESIAN_POINT('Ctrl Pts',(-0.154501464116133,0.0180961536281239,
1.03825412354951));
#15008=CARTESIAN_POINT('Ctrl Pts',(-0.154314777935465,0.0196245301591377,
1.03814273739566));
#15009=CARTESIAN_POINT('Ctrl Pts',(-0.153177925353005,0.027908054748001,
1.03753396069297));
#15010=CARTESIAN_POINT('Ctrl Pts',(-0.15180699820084,0.0345969160339381,
1.03702347618112));
#15011=CARTESIAN_POINT('Ctrl Pts',(-0.146992244641157,0.0521378965533142,
1.03563505623994));
#15012=CARTESIAN_POINT('Ctrl Pts',(-0.142789835132019,0.0627385163250416,
1.03474117253609));
#15013=CARTESIAN_POINT('Ctrl Pts',(-0.137084250266438,0.0735145576289548,
1.03381248727888));
#15014=CARTESIAN_POINT('Ctrl Pts',(-0.136692780018179,0.0742399204835402,
1.03374988908897));
#15015=CARTESIAN_POINT('Ctrl Pts',(-0.134756038515252,0.077761287729729,
1.03344568520926));
#15016=CARTESIAN_POINT('Ctrl Pts',(-0.133130508350137,0.0805126035024925,
1.03320702448004));
#15017=CARTESIAN_POINT('Ctrl Pts',(-0.131129005210508,0.0836736811500931,
1.03293328622031));
#15018=CARTESIAN_POINT('Ctrl Pts',(-0.130834333783726,0.0841336915384147,
1.03289346315085));
#15019=CARTESIAN_POINT('Ctrl Pts',(-0.130356825132937,0.0848705526022756,
1.03282970467976));
#15020=CARTESIAN_POINT('Ctrl Pts',(-0.130175518600981,0.0851483817831765,
1.03280567218244));
#15021=CARTESIAN_POINT('Ctrl Pts',(-0.129851136339618,0.0856419985902897,
1.03276298976655));
#15022=CARTESIAN_POINT('Ctrl Pts',(-0.129708409410495,0.0858580110617567,
1.03274431702986));
#15023=CARTESIAN_POINT('Ctrl Pts',(-0.129402926228979,0.0863178493697545,
1.03270457997533));
#15024=CARTESIAN_POINT('Ctrl Pts',(-0.129240020209961,0.0865615712452648,
1.03268352596436));
#15025=CARTESIAN_POINT('Ctrl Pts',(-0.128794463471499,0.0872241019831028,
1.03262630853718));
#15026=CARTESIAN_POINT('Ctrl Pts',(-0.12851045623412,0.0876420016041505,
1.0325902349196));
#15027=CARTESIAN_POINT('Ctrl Pts',(-0.127036443167708,0.0897883522852053,
1.03240500526207));
#15028=CARTESIAN_POINT('Ctrl Pts',(-0.125813511017835,0.0914940856854288,
1.03225795500926));
#15029=CARTESIAN_POINT('Ctrl Pts',(-0.122099379454723,0.0964591554942415,
1.03182866613633));
#15030=CARTESIAN_POINT('Ctrl Pts',(-0.119513235456922,0.0996454684090201,
1.03155150908419));
#15031=CARTESIAN_POINT('Ctrl Pts',(-0.10992207231965,0.110551032666018,
1.03058196476839));
#15032=CARTESIAN_POINT('Ctrl Pts',(-0.102271325088489,0.117664688174515,
1.02990834360504));
#15033=CARTESIAN_POINT('Ctrl Pts',(-0.0888470525279429,0.127840813923076,
1.02878131596413));
#15034=CARTESIAN_POINT('Ctrl Pts',(-0.0834926896625997,0.131400251833672,
1.02834409311594));
#15035=CARTESIAN_POINT('Ctrl Pts',(-0.0770749002046541,0.135115683781773,
1.02782449295394));
#15036=CARTESIAN_POINT('Ctrl Pts',(-0.0762109318635579,0.135604874650322,
1.02775464162569));
#15037=CARTESIAN_POINT('Ctrl Pts',(-0.0748177402280161,0.136376199647507,
1.02764212760664));
#15038=CARTESIAN_POINT('Ctrl Pts',(-0.0742914549166371,0.13666360814519,
1.02759965311995));
#15039=CARTESIAN_POINT('Ctrl Pts',(-0.0733540270983685,0.137168529731964,
1.02752404016595));
#15040=CARTESIAN_POINT('Ctrl Pts',(-0.0729435435536719,0.137387256634697,
1.02749094517889));
#15041=CARTESIAN_POINT('Ctrl Pts',(-0.0720862412349883,0.137839146596797,
1.02742185272222));
#15042=CARTESIAN_POINT('Ctrl Pts',(-0.0716392586049876,0.138071985302678,
1.02738584429824));
#15043=CARTESIAN_POINT('Ctrl Pts',(-0.0704755970230742,0.138670979012717,
1.02729213545477));
#15044=CARTESIAN_POINT('Ctrl Pts',(-0.0697572018836638,0.139033747472617,
1.02723431727667));
#15045=CARTESIAN_POINT('Ctrl Pts',(-0.0672695769006429,0.140265791643921,
1.02703419969377));
#15046=CARTESIAN_POINT('Ctrl Pts',(-0.0654867846816166,0.141106938634866,
1.02689093980976));
#15047=CARTESIAN_POINT('Ctrl Pts',(-0.0636886257384703,0.141913922683946,
1.02674653231234));
#15048=CARTESIAN_POINT('',(-0.155549929113474,0.000137046190443996,1.02555842627611));
#15049=CARTESIAN_POINT('Ctrl Pts',(-0.063688626060837,0.141913922539273,
1.01289638536134));
#15050=CARTESIAN_POINT('Ctrl Pts',(-0.0647860609483699,0.141421411875573,
1.01297710100986));
#15051=CARTESIAN_POINT('Ctrl Pts',(-0.0658778700550637,0.140916132225413,
1.01305747580239));
#15052=CARTESIAN_POINT('Ctrl Pts',(-0.0760690842855253,0.136055365930432,
1.01380936440437));
#15053=CARTESIAN_POINT('Ctrl Pts',(-0.0847302227510347,0.130837162779552,
1.01446245564984));
#15054=CARTESIAN_POINT('Ctrl Pts',(-0.0952273593882092,0.123030541893768,
1.01533815688697));
#15055=CARTESIAN_POINT('Ctrl Pts',(-0.0975773191783891,0.121175201413414,
1.01554017014227));
#15056=CARTESIAN_POINT('Ctrl Pts',(-0.102650124851414,0.116926830655957,
1.01599176444776));
#15057=CARTESIAN_POINT('Ctrl Pts',(-0.105345713945323,0.114504187027946,
1.01624227641435));
#15058=CARTESIAN_POINT('Ctrl Pts',(-0.108617462215164,0.111350340665435,
1.016561467905));
#15059=CARTESIAN_POINT('Ctrl Pts',(-0.109275120327414,0.110705011072708,
1.01662643313479));
#15060=CARTESIAN_POINT('Ctrl Pts',(-0.110305605145272,0.109675714431107,
1.01672953292112));
#15061=CARTESIAN_POINT('Ctrl Pts',(-0.110682257903037,0.109295592934538,
1.01676749802043));
#15062=CARTESIAN_POINT('Ctrl Pts',(-0.111378872258385,0.108585269341235,
1.01683824409808));
#15063=CARTESIAN_POINT('Ctrl Pts',(-0.111699346758633,0.108255576432907,
1.01687100214167));
#15064=CARTESIAN_POINT('Ctrl Pts',(-0.112323589949379,0.107607653929309,
1.01693522953592));
#15065=CARTESIAN_POINT('Ctrl Pts',(-0.112627479845196,0.107289546646727,
1.01696669319418));
#15066=CARTESIAN_POINT('Ctrl Pts',(-0.113517513823187,0.106349924313232,
1.01705942952358));
#15067=CARTESIAN_POINT('Ctrl Pts',(-0.114099883571762,0.105724873425555,
1.01712086294045));
#15068=CARTESIAN_POINT('Ctrl Pts',(-0.116964830475933,0.102598716268135,
1.01742689602063));
#15069=CARTESIAN_POINT('Ctrl Pts',(-0.119170294333364,0.100028524794018,
1.01767469167025));
#15070=CARTESIAN_POINT('Ctrl Pts',(-0.125196932601442,0.0925228114824073,
1.01838852799206));
#15071=CARTESIAN_POINT('Ctrl Pts',(-0.128807067184689,0.0874269130915619,
1.01886202898012));
#15072=CARTESIAN_POINT('Ctrl Pts',(-0.13395178446543,0.0791518038537113,
1.0196115992907));
#15073=CARTESIAN_POINT('Ctrl Pts',(-0.135701272316662,0.0761134159306673,
1.0198829829854));
#15074=CARTESIAN_POINT('Ctrl Pts',(-0.13980491859699,0.0683945368410447,
1.02056082806488));
#15075=CARTESIAN_POINT('Ctrl Pts',(-0.142028237974713,0.0636491242664318,
1.02096743996051));
#15076=CARTESIAN_POINT('Ctrl Pts',(-0.144383867333696,0.0578799616989279,
1.02144466275083));
#15077=CARTESIAN_POINT('Ctrl Pts',(-0.144750897720426,0.0569558495145081,
1.02152059276024));
#15078=CARTESIAN_POINT('Ctrl Pts',(-0.14649447471692,0.0524401144942479,
1.02188896295792));
#15079=CARTESIAN_POINT('Ctrl Pts',(-0.147746487837052,0.0488014171157882,
1.02217764892268));
#15080=CARTESIAN_POINT('Ctrl Pts',(-0.149045187578953,0.0445166442764345,
1.02250544703461));
#15081=CARTESIAN_POINT('Ctrl Pts',(-0.149224303425284,0.0439124909539369,
1.02255138919605));
#15082=CARTESIAN_POINT('Ctrl Pts',(-0.149489963520654,0.0429960266407157,
1.02262064426518));
#15083=CARTESIAN_POINT('Ctrl Pts',(-0.14957920839652,0.0426845161735899,
1.0226441083061));
#15084=CARTESIAN_POINT('Ctrl Pts',(-0.149737650714609,0.0421248716764276,
1.02268612343052));
#15085=CARTESIAN_POINT('Ctrl Pts',(-0.149807205442616,0.041876843913858,
1.0227046948792));
#15086=CARTESIAN_POINT('Ctrl Pts',(-0.149956941572525,0.041337746915761,
1.02274495363199));
#15087=CARTESIAN_POINT('Ctrl Pts',(-0.150036891607409,0.0410466174838701,
1.02276662741799));
#15088=CARTESIAN_POINT('Ctrl Pts',(-0.150199845258332,0.0404464016318723,
1.02281117704768));
#15089=CARTESIAN_POINT('Ctrl Pts',(-0.150282743698556,0.0401372877994007,
1.02283404684204));
#15090=CARTESIAN_POINT('Ctrl Pts',(-0.1504922043831,0.0393464984929881,
1.02289237105019));
#15091=CARTESIAN_POINT('Ctrl Pts',(-0.150617409745395,0.0388644622096398,
1.02292775074723));
#15092=CARTESIAN_POINT('Ctrl Pts',(-0.150974076895866,0.0374636920773357,
1.02303008434339));
#15093=CARTESIAN_POINT('Ctrl Pts',(-0.151199467838778,0.0365434146561254,
1.02309672042778));
#15094=CARTESIAN_POINT('Ctrl Pts',(-0.154152104867538,0.0239924909809659,
1.02399816488502));
#15095=CARTESIAN_POINT('Ctrl Pts',(-0.155539404807646,0.0120860470003205,
1.02476979575327));
#15096=CARTESIAN_POINT('Ctrl Pts',(-0.155549939545188,0.000137140396363124,
1.02555840182376));
#15097=CARTESIAN_POINT('Ctrl Pts',(-0.155549939629264,0.000137045001298319,
1.02555840811966));
#15098=CARTESIAN_POINT('Ctrl Pts',(-0.15555638673202,-0.00718059836358552,
1.02604135928988));
#15099=CARTESIAN_POINT('Ctrl Pts',(-0.155046468706238,-0.0144890321433455,
1.02652860014069));
#15100=CARTESIAN_POINT('Ctrl Pts',(-0.153657490307648,-0.0243323487880368,
1.02721131832332));
#15101=CARTESIAN_POINT('Ctrl Pts',(-0.153225198880862,-0.0269207088545793,
1.0273933055807));
#15102=CARTESIAN_POINT('Ctrl Pts',(-0.152589172553378,-0.0302139105113054,
1.02762857309124));
#15103=CARTESIAN_POINT('Ctrl Pts',(-0.152445622439239,-0.0309300523082306,
1.02767996051711));
#15104=CARTESIAN_POINT('Ctrl Pts',(-0.152193820717065,-0.0321418860646949,
1.02776731336339));
#15105=CARTESIAN_POINT('Ctrl Pts',(-0.152088176654594,-0.0326381129224696,
1.02780319605185));
#15106=CARTESIAN_POINT('Ctrl Pts',(-0.151888104592615,-0.0335558152533673,
1.02786976999309));
#15107=CARTESIAN_POINT('Ctrl Pts',(-0.151794344794366,-0.0339774327406821,
1.02790043971062));
#15108=CARTESIAN_POINT('Ctrl Pts',(-0.151596719587348,-0.0348489644006529,
1.02796401393735));
#15109=CARTESIAN_POINT('Ctrl Pts',(-0.151492604511346,-0.0352988169683653,
1.02799692615122));
#15110=CARTESIAN_POINT('Ctrl Pts',(-0.151252241920828,-0.0363167046911205,
1.02807162169078));
#15111=CARTESIAN_POINT('Ctrl Pts',(-0.151114795156655,-0.036884446494989,
1.02811344310804));
#15112=CARTESIAN_POINT('Ctrl Pts',(-0.150699234371018,-0.0385596562193391,
1.02823732199884));
#15113=CARTESIAN_POINT('Ctrl Pts',(-0.150412125425806,-0.0396648298038098,
1.02831966747295));
#15114=CARTESIAN_POINT('Ctrl Pts',(-0.147808877674448,-0.0492506161193129,
1.02903945206169));
#15115=CARTESIAN_POINT('Ctrl Pts',(-0.144790268005165,-0.0575222821753394,
1.02969993143085));
#15116=CARTESIAN_POINT('Ctrl Pts',(-0.138594862237303,-0.0708687962269089,
1.03083027615649));
#15117=CARTESIAN_POINT('Ctrl Pts',(-0.135794596768898,-0.0760969462009458,
1.03129090727525));
#15118=CARTESIAN_POINT('Ctrl Pts',(-0.128882948186217,-0.0873990998547369,
1.03231709409162));
#15119=CARTESIAN_POINT('Ctrl Pts',(-0.124626065847134,-0.0933690903900244,
1.03288068852961));
#15120=CARTESIAN_POINT('Ctrl Pts',(-0.119258877614252,-0.0998716635760938,
1.03350340387367));
#15121=CARTESIAN_POINT('Ctrl Pts',(-0.118544748090849,-0.100718280188701,
1.03358465558085));
#15122=CARTESIAN_POINT('Ctrl Pts',(-0.11761931029254,-0.10179192676455,
1.03368784540701));
#15123=CARTESIAN_POINT('Ctrl Pts',(-0.117416307608891,-0.102026022269235,
1.0337103539049));
#15124=CARTESIAN_POINT('Ctrl Pts',(-0.117018844857276,-0.102481604769332,
1.03375417397945));
#15125=CARTESIAN_POINT('Ctrl Pts',(-0.116824452234789,-0.102703148597403,
1.03377549026883));
#15126=CARTESIAN_POINT('Ctrl Pts',(-0.116458377500567,-0.103117969520258,
1.03381541438236));
#15127=CARTESIAN_POINT('Ctrl Pts',(-0.11628684535156,-0.10331136882119,
1.0338340322998));
#15128=CARTESIAN_POINT('Ctrl Pts',(-0.11589228745911,-0.103753997795884,
1.03387665413083));
#15129=CARTESIAN_POINT('Ctrl Pts',(-0.115668939709457,-0.104002936224478,
1.03390063358425));
#15130=CARTESIAN_POINT('Ctrl Pts',(-0.115080513889742,-0.104654542373605,
1.0339634294704));
#15131=CARTESIAN_POINT('Ctrl Pts',(-0.114714120861869,-0.105056025123374,
1.03400214971291));
#15132=CARTESIAN_POINT('Ctrl Pts',(-0.11221541397595,-0.107765376097631,
1.03426371397184));
#15133=CARTESIAN_POINT('Ctrl Pts',(-0.110015509031068,-0.110010303150013,
1.03448176231003));
#15134=CARTESIAN_POINT('Ctrl Pts',(-0.103903846574431,-0.115880177176948,
1.03506079674051));
#15135=CARTESIAN_POINT('Ctrl Pts',(-0.0998711563501876,-0.11937330497986,
1.03541523746203));
#15136=CARTESIAN_POINT('Ctrl Pts',(-0.0900258171908573,-0.127052481858011,
1.03623970143847));
#15137=CARTESIAN_POINT('Ctrl Pts',(-0.0840882067401964,-0.131057820393929,
1.03670708353823));
#15138=CARTESIAN_POINT('Ctrl Pts',(-0.0736789606190546,-0.137080086506898,
1.0375082964557));
#15139=CARTESIAN_POINT('Ctrl Pts',(-0.0693498745563778,-0.139320234349415,
1.03783661039076));
#15140=CARTESIAN_POINT('Ctrl Pts',(-0.0623248513823275,-0.142546800669475,
1.03836803899733));
#15141=CARTESIAN_POINT('Ctrl Pts',(-0.0596943554125757,-0.143668227518083,
1.03856671905054));
#15142=CARTESIAN_POINT('Ctrl Pts',(-0.0562665431508622,-0.145019171648208,
1.03882593928562));
#15143=CARTESIAN_POINT('Ctrl Pts',(-0.0554961110168068,-0.145315744634239,
1.0388842206676));
#15144=CARTESIAN_POINT('Ctrl Pts',(-0.0543164782900724,-0.14575908764223,
1.03897350248566));
#15145=CARTESIAN_POINT('Ctrl Pts',(-0.0539089534078625,-0.145910301828275,
1.03900435465503));
#15146=CARTESIAN_POINT('Ctrl Pts',(-0.0531124012079008,-0.146202073976774,
1.03906467729382));
#15147=CARTESIAN_POINT('Ctrl Pts',(-0.0527234361511966,-0.146342792345662,
1.0390941421451));
#15148=CARTESIAN_POINT('Ctrl Pts',(-0.0518256092848952,-0.146663560846093,
1.03916217674319));
#15149=CARTESIAN_POINT('Ctrl Pts',(-0.0513163648635911,-0.146842516123313,
1.03920078233914));
#15150=CARTESIAN_POINT('Ctrl Pts',(-0.0499162159752346,-0.147326374271991,
1.03930697869207));
#15151=CARTESIAN_POINT('Ctrl Pts',(-0.0490234709920573,-0.147625839177458,
1.03937474757955));
#15152=CARTESIAN_POINT('Ctrl Pts',(-0.044445477679734,-0.149115389190766,
1.03972261090321));
#15153=CARTESIAN_POINT('Ctrl Pts',(-0.0407197456305465,-0.150175554462964,
1.04000690180176));
#15154=CARTESIAN_POINT('Ctrl Pts',(-0.0239888927808989,-0.154267994572837,
1.04129016625844));
#15155=CARTESIAN_POINT('Ctrl Pts',(-0.0106659611612102,-0.155756875866865,
1.0423361013792));
#15156=CARTESIAN_POINT('Ctrl Pts',(0.00817651927052412,-0.155432200473962,
1.04378662559924));
#15157=CARTESIAN_POINT('Ctrl Pts',(0.0136649733281473,-0.155046147179955,
1.04420466206531));
#15158=CARTESIAN_POINT('Ctrl Pts',(0.0199782635207121,-0.154264110596041,
1.04467259664815));
#15159=CARTESIAN_POINT('Ctrl Pts',(0.0208335953327372,-0.154150926783172,
1.0447357133346));
#15160=CARTESIAN_POINT('Ctrl Pts',(0.0220571587866953,-0.153978645438524,
1.04482556035108));
#15161=CARTESIAN_POINT('Ctrl Pts',(0.0224261676963277,-0.153925334221279,
1.04485259916815));
#15162=CARTESIAN_POINT('Ctrl Pts',(0.0230565395317354,-0.153831948554754,
1.04489868636746));
#15163=CARTESIAN_POINT('Ctrl Pts',(0.0233179969262047,-0.153792533742621,
1.04491777153483));
#15164=CARTESIAN_POINT('Ctrl Pts',(0.0238205546847454,-0.153715461873917,
1.04495439617364));
#15165=CARTESIAN_POINT('Ctrl Pts',(0.024061667327688,-0.153677904112031,
1.04497194130618));
#15166=CARTESIAN_POINT('Ctrl Pts',(0.0247031289444782,-0.153576437911108,
1.04501855117061));
#15167=CARTESIAN_POINT('Ctrl Pts',(0.0251033219348603,-0.153511530833782,
1.04504755983632));
#15168=CARTESIAN_POINT('Ctrl Pts',(0.0265378143113057,-0.153273111714175,
1.04515130472308));
#15169=CARTESIAN_POINT('Ctrl Pts',(0.0275706380732488,-0.153090700039239,
1.04522555837581));
#15170=CARTESIAN_POINT('Ctrl Pts',(0.0289267396891793,-0.152837023207303,
1.04532256690412));
#15171=CARTESIAN_POINT('Ctrl Pts',(0.0292517129266021,-0.15277515906515,
1.0453457769324));
#15172=CARTESIAN_POINT('Ctrl Pts',(0.0306709667188219,-0.152500285615089,
1.04544699061635));
#15173=CARTESIAN_POINT('Ctrl Pts',(0.0317631688852504,-0.152276546373705,
1.0455244872103));
#15174=CARTESIAN_POINT('Ctrl Pts',(0.047402082307416,-0.148897303309184,
1.0466297226484));
#15175=CARTESIAN_POINT('Ctrl Pts',(0.0614263248973267,-0.14368122410808,
1.04757244456601));
#15176=CARTESIAN_POINT('Ctrl Pts',(0.0779899716290621,-0.134644721141109,
1.04883869988228));
#15177=CARTESIAN_POINT('Ctrl Pts',(0.0814084843795106,-0.132605774035906,
1.04910877983507));
#15178=CARTESIAN_POINT('Ctrl Pts',(0.0868251284683801,-0.129086612970358,
1.04955445353322));
#15179=CARTESIAN_POINT('Ctrl Pts',(0.0888726438301031,-0.127685584766996,
1.04972725785172));
#15180=CARTESIAN_POINT('Ctrl Pts',(0.0915201024552387,-0.125779507292003,
1.04995695163857));
#15181=CARTESIAN_POINT('Ctrl Pts',(0.092151054125934,-0.125317982713782,
1.05001217284377));
#15182=CARTESIAN_POINT('Ctrl Pts',(0.0931788548844407,-0.124554214339172,
1.05010293110671));
#15183=CARTESIAN_POINT('Ctrl Pts',(0.0935777821293927,-0.124254778533468,
1.05013835882304));
#15184=CARTESIAN_POINT('Ctrl Pts',(0.0943472287041001,-0.12367142284037,
1.0502070861079));
#15185=CARTESIAN_POINT('Ctrl Pts',(0.0947179242917529,-0.123387743316071,
1.05024037599956));
#15186=CARTESIAN_POINT('Ctrl Pts',(0.0955708971304279,-0.122728886044468,
1.05031739504716));
#15187=CARTESIAN_POINT('Ctrl Pts',(0.0960522490324654,-0.122352528719732,
1.05036117053008));
#15188=CARTESIAN_POINT('Ctrl Pts',(0.0973406894648549,-0.121332839474084,
1.05047919589814));
#15189=CARTESIAN_POINT('Ctrl Pts',(0.0981436005974994,-0.120684304392054,
1.05055365254962));
#15190=CARTESIAN_POINT('Ctrl Pts',(0.105252511557614,-0.114824368025818,
1.05122116184318));
#15191=CARTESIAN_POINT('Ctrl Pts',(0.111143566069588,-0.109131990173809,
1.05183409310911));
#15192=CARTESIAN_POINT('Ctrl Pts',(0.12137141947274,-0.0975581665313749,
1.05301740366399));
#15193=CARTESIAN_POINT('Ctrl Pts',(0.125796107690552,-0.0917820685073719,
1.05358329161818));
#15194=CARTESIAN_POINT('Ctrl Pts',(0.133652426975203,-0.0798854723415791,
1.05468597355418));
#15195=CARTESIAN_POINT('Ctrl Pts',(0.137107274774414,-0.0737989238872712,
1.05522173388818));
#15196=CARTESIAN_POINT('Ctrl Pts',(0.140506342900226,-0.0667418752230778,
1.05579751233231));
#15197=CARTESIAN_POINT('Ctrl Pts',(0.140865279488935,-0.0659809322687426,
1.05585902504274));
#15198=CARTESIAN_POINT('Ctrl Pts',(0.141368859449671,-0.0648905038175394,
1.05594632085494));
#15199=CARTESIAN_POINT('Ctrl Pts',(0.141518552544912,-0.0645633890100181,
1.05597239984413));
#15200=CARTESIAN_POINT('Ctrl Pts',(0.141775337618558,-0.0639970688885476,
1.05601735811322));
#15201=CARTESIAN_POINT('Ctrl Pts',(0.141882961727943,-0.0637581081819211,
1.0560362697451));
#15202=CARTESIAN_POINT('Ctrl Pts',(0.142091022322258,-0.0632930098663629,
1.0560729629802));
#15203=CARTESIAN_POINT('Ctrl Pts',(0.14219152308005,-0.0630669048634031,
1.05609074865594));
#15204=CARTESIAN_POINT('Ctrl Pts',(0.142462339179833,-0.0624536890412416,
1.05613884529386));
#15205=CARTESIAN_POINT('Ctrl Pts',(0.142631617724237,-0.0620661179397875,
1.05616909344945));
#15206=CARTESIAN_POINT('Ctrl Pts',(0.143260170546572,-0.060610864462488,
1.05628212449736));
#15207=CARTESIAN_POINT('Ctrl Pts',(0.143709070050202,-0.059538699647432,
1.0563643048027));
#15208=CARTESIAN_POINT('Ctrl Pts',(0.147448148468797,-0.0503194295806551,
1.05706246195061));
#15209=CARTESIAN_POINT('Ctrl Pts',(0.150055099039325,-0.0419108167251852,
1.05764330628785));
#15210=CARTESIAN_POINT('Ctrl Pts',(0.153916072896132,-0.0243080105455735,
1.05883034463277));
#15211=CARTESIAN_POINT('Ctrl Pts',(0.15508714616739,-0.0151326586777039,
1.05943450274364));
#15212=CARTESIAN_POINT('Ctrl Pts',(0.155601387929949,-0.00160304465676362,
1.06035399711173));
#15213=CARTESIAN_POINT('Ctrl Pts',(0.155586088778054,0.00270644086793452,
1.06065087361816));
#15214=CARTESIAN_POINT('Ctrl Pts',(0.155349709937214,0.00794672527266573,
1.06101928921471));
#15215=CARTESIAN_POINT('Ctrl Pts',(0.155298951399112,0.00888360544141311,
1.06108544202211));
#15216=CARTESIAN_POINT('Ctrl Pts',(0.155206049001805,0.010352262687595,
1.06118961680611));
#15217=CARTESIAN_POINT('Ctrl Pts',(0.155169639421713,0.0108843915012997,
1.06122745931737));
#15218=CARTESIAN_POINT('Ctrl Pts',(0.155100138035701,0.0118288103339126,
1.06129479981587));
#15219=CARTESIAN_POINT('Ctrl Pts',(0.155068137072414,0.0122411776981126,
1.06132426336619));
#15220=CARTESIAN_POINT('Ctrl Pts',(0.15499047865882,0.0131926788158454,
1.06139238958401));
#15221=CARTESIAN_POINT('Ctrl Pts',(0.154943652346649,0.0137317090357788,
1.06143108852619));
#15222=CARTESIAN_POINT('Ctrl Pts',(0.154807111791426,0.0152137417484865,
1.06153778451709));
#15223=CARTESIAN_POINT('Ctrl Pts',(0.154711595621551,0.0161561723702731,
1.06160596246047));
#15224=CARTESIAN_POINT('Ctrl Pts',(0.154174160474704,0.0210159911292765,
1.0619592908737));
#15225=CARTESIAN_POINT('Ctrl Pts',(0.153592081076033,0.02491608052403,1.06224879629655));
#15226=CARTESIAN_POINT('Ctrl Pts',(0.152497251361756,0.0307292486535779,
1.06268976956176));
#15227=CARTESIAN_POINT('Ctrl Pts',(0.152095063209109,0.0326617445901642,
1.06283794475441));
#15228=CARTESIAN_POINT('Ctrl Pts',(0.148397923695127,0.0488733426306351,
1.06409413651517));
#15229=CARTESIAN_POINT('Ctrl Pts',(0.143137722902858,0.0626263656406572,
1.06525590161234));
#15230=CARTESIAN_POINT('Ctrl Pts',(0.134738491699489,0.0777718093808967,
1.06655970121872));
#15231=CARTESIAN_POINT('Ctrl Pts',(0.133385148051825,0.0800707192484765,
1.06675804369127));
#15232=CARTESIAN_POINT('Ctrl Pts',(0.131685488591,0.0827951094216,1.06699264285331));
#15233=CARTESIAN_POINT('Ctrl Pts',(0.131395311181108,0.0832548513477145,
1.06703221547851));
#15234=CARTESIAN_POINT('Ctrl Pts',(0.130940450828424,0.0839672064189209,
1.06709349558014));
#15235=CARTESIAN_POINT('Ctrl Pts',(0.130777437561475,0.0842208717956763,
1.06711530983263));
#15236=CARTESIAN_POINT('Ctrl Pts',(0.130473775096756,0.0846903942935624,
1.06715567122704));
#15237=CARTESIAN_POINT('Ctrl Pts',(0.130333328578934,0.0849063739482967,
1.06717423093138));
#15238=CARTESIAN_POINT('Ctrl Pts',(0.130014746267877,0.0853936389680652,
1.06721608918345));
#15239=CARTESIAN_POINT('Ctrl Pts',(0.129836298049103,0.0856647158252774,
1.06723936653524));
#15240=CARTESIAN_POINT('Ctrl Pts',(0.129307602782967,0.086462398428511,
1.06730784215413));
#15241=CARTESIAN_POINT('Ctrl Pts',(0.128954985250558,0.0869874375709762,
1.06735288565789));
#15242=CARTESIAN_POINT('Ctrl Pts',(0.126402072990087,0.0907390222725643,
1.06767465291229));
#15243=CARTESIAN_POINT('Ctrl Pts',(0.124083924370035,0.0938841865071074,
1.06794396832215));
#15244=CARTESIAN_POINT('Ctrl Pts',(0.120883022390932,0.0979010234299841,
1.06829220904676));
#15245=CARTESIAN_POINT('Ctrl Pts',(0.120105060143235,0.0988538828532884,
1.06837514926172));
#15246=CARTESIAN_POINT('Ctrl Pts',(0.109794580690215,0.1111808903071,1.06945397985748));
#15247=CARTESIAN_POINT('Ctrl Pts',(0.0986936807561965,0.121142998892111,
1.07039962773869));
#15248=CARTESIAN_POINT('Ctrl Pts',(0.0836236490103462,0.13120070260349,
1.0716405631523));
#15249=CARTESIAN_POINT('Ctrl Pts',(0.0808416115047966,0.132932953776351,
1.07186770146406));
#15250=CARTESIAN_POINT('Ctrl Pts',(0.0772618433269091,0.135007970601706,
1.07215865035472));
#15251=CARTESIAN_POINT('Ctrl Pts',(0.0765130053908597,0.135433764301552,
1.07221944023647));
#15252=CARTESIAN_POINT('Ctrl Pts',(0.0753096377071011,0.136104840760534,
1.07231703206297));
#15253=CARTESIAN_POINT('Ctrl Pts',(0.0748573478585455,0.136354122306217,
1.07235369071308));
#15254=CARTESIAN_POINT('Ctrl Pts',(0.073998234657351,0.136822063573469,
1.07242328656145));
#15255=CARTESIAN_POINT('Ctrl Pts',(0.0735916615311184,0.137041173220109,
1.0724562073157));
#15256=CARTESIAN_POINT('Ctrl Pts',(0.0726677382375444,0.137533795039334,
1.07253098744599));
#15257=CARTESIAN_POINT('Ctrl Pts',(0.0721498108724101,0.137806203533238,
1.07257288525258));
#15258=CARTESIAN_POINT('Ctrl Pts',(0.0706123965769501,0.138603777354705,
1.07269719804892));
#15259=CARTESIAN_POINT('Ctrl Pts',(0.0695886451013722,0.139120587941932,
1.0727799040547));
#15260=CARTESIAN_POINT('Ctrl Pts',(0.0598130626881689,0.143920603518945,
1.07356912409087));
#15261=CARTESIAN_POINT('Ctrl Pts',(0.0506844926983515,0.147383018702806,
1.07430427059204));
#15262=CARTESIAN_POINT('Ctrl Pts',(0.0359713117426475,0.151434292157295,
1.0754807478648));
#15263=CARTESIAN_POINT('Ctrl Pts',(0.0305745581743558,0.152615446450166,
1.07591011801506));
#15264=CARTESIAN_POINT('Ctrl Pts',(0.022396772766402,0.153954014577287,
1.07655129702871));
#15265=CARTESIAN_POINT('Ctrl Pts',(0.0196554356018252,0.154327958805929,
1.07676462717102));
#15266=CARTESIAN_POINT('Ctrl Pts',(0.0126390444695441,0.155095058921444,
1.07730469236253));
#15267=CARTESIAN_POINT('Ctrl Pts',(0.00835463179472849,0.155384782872206,
1.07762890009589));
#15268=CARTESIAN_POINT('Ctrl Pts',(0.00315740721380089,0.155520591813789,
1.07801150601459));
#15269=CARTESIAN_POINT('Ctrl Pts',(0.00225129750139979,0.15553634772494,
1.07807781735803));
#15270=CARTESIAN_POINT('Ctrl Pts',(0.000974385890557175,0.155547389857333,
1.07817066262109));
#15271=CARTESIAN_POINT('Ctrl Pts',(0.000603683169115436,0.155549270308945,
1.07819754519448));
#15272=CARTESIAN_POINT('Ctrl Pts',(-3.10391346713135E-5,0.155550220953408,
1.07824344748054));
#15273=CARTESIAN_POINT('Ctrl Pts',(-0.000295054584715183,0.155549944227611,
1.07826250325319));
#15274=CARTESIAN_POINT('Ctrl Pts',(-0.000803595253981717,0.155548116435916,
1.07829913441133));
#15275=CARTESIAN_POINT('Ctrl Pts',(-0.00104811779847694,0.155546660984548,
1.07831671520905));
#15276=CARTESIAN_POINT('Ctrl Pts',(-0.00170066357540278,0.155541238067592,
1.07836354762745));
#15277=CARTESIAN_POINT('Ctrl Pts',(-0.00210868024925973,0.155536241673692,
1.07839274218876));
#15278=CARTESIAN_POINT('Ctrl Pts',(-0.00358170545025264,0.155512406144702,
1.07849783725151));
#15279=CARTESIAN_POINT('Ctrl Pts',(-0.00464656617794333,0.15548423286056,
1.07857323862844));
#15280=CARTESIAN_POINT('Ctrl Pts',(-0.0173853034967802,0.155016208496515,
1.07946930766489));
#15281=CARTESIAN_POINT('Ctrl Pts',(-0.0289761485197711,0.153273456008125,
1.08022670769006));
#15282=CARTESIAN_POINT('Ctrl Pts',(-0.0482860736035472,0.148098724003954,
1.08154419935884));
#15283=CARTESIAN_POINT('Ctrl Pts',(-0.0561189341247354,0.145311076014374,
1.08209531018966));
#15284=CARTESIAN_POINT('Ctrl Pts',(-0.0636886366174998,0.141913917801617,
1.08266645291));
#15285=CARTESIAN_POINT('Origin',(0.,0.,-0.129405622560373));
#15286=CARTESIAN_POINT('',(-0.063688625668895,0.14191392271517,1.16646420862114));
#15287=CARTESIAN_POINT('',(-0.0636886503124993,0.141913911655525,1.15273999320994));
#15288=CARTESIAN_POINT('',(-0.0636886258329924,0.141913922641526,-0.129405622560373));
#15289=CARTESIAN_POINT('',(-0.155549963960585,-0.000105886074850944,1.10930622288127));
#15290=CARTESIAN_POINT('Ctrl Pts',(-0.063688625668895,0.14191392271517,
1.16646420862114));
#15291=CARTESIAN_POINT('Ctrl Pts',(-0.0633562430797375,0.142063090533907,
1.16643737473818));
#15292=CARTESIAN_POINT('Ctrl Pts',(-0.0630233164927144,0.142211099570305,
1.16641059995971));
#15293=CARTESIAN_POINT('Ctrl Pts',(-0.0620459505366581,0.142641500039162,
1.16633230565896));
#15294=CARTESIAN_POINT('Ctrl Pts',(-0.061400116299543,0.142920688776291,
1.16628096054214));
#15295=CARTESIAN_POINT('Ctrl Pts',(-0.0604444253465264,0.143326152047841,
1.16620557966343));
#15296=CARTESIAN_POINT('Ctrl Pts',(-0.0601360323837594,0.143455819091346,
1.1661813463566));
#15297=CARTESIAN_POINT('Ctrl Pts',(-0.0595885203170512,0.143683950446014,
1.16613848815509));
#15298=CARTESIAN_POINT('Ctrl Pts',(-0.0593495720378749,0.143782814244999,
1.16611983937787));
#15299=CARTESIAN_POINT('Ctrl Pts',(-0.0588376497593383,0.143993126231899,
1.1660800058962));
#15300=CARTESIAN_POINT('Ctrl Pts',(-0.0585646057520897,0.144104394063067,
1.16605883213009));
#15301=CARTESIAN_POINT('Ctrl Pts',(-0.0578157134663128,0.144407094180099,
1.16600095093007));
#15302=CARTESIAN_POINT('Ctrl Pts',(-0.0573392262610129,0.144596952681633,
1.16596433684071));
#15303=CARTESIAN_POINT('Ctrl Pts',(-0.0548145519022079,0.145588478520955,
1.16577141674684));
#15304=CARTESIAN_POINT('Ctrl Pts',(-0.0527503385582262,0.146349046113564,
1.16561743048276));
#15305=CARTESIAN_POINT('Ctrl Pts',(-0.0374258082868009,0.15162901781501,
1.16449672842429));
#15306=CARTESIAN_POINT('Ctrl Pts',(-0.0236237399812131,0.154382896166755,
1.16360521488536));
#15307=CARTESIAN_POINT('Ctrl Pts',(-0.00283498022770765,0.155673451882592,
1.16221468753969));
#15308=CARTESIAN_POINT('Ctrl Pts',(0.003987463663544,0.155648132176121,
1.16175177476129));
#15309=CARTESIAN_POINT('Ctrl Pts',(0.0117858821283563,0.155106095329073,
1.16120412078219));
#15310=CARTESIAN_POINT('Ctrl Pts',(0.0127854113815099,0.155026904111061,
1.16113358687199));
#15311=CARTESIAN_POINT('Ctrl Pts',(0.0143842477566286,0.154884663420545,
1.16102018378491));
#15312=CARTESIAN_POINT('Ctrl Pts',(0.0149840876226635,0.154827783831081,
1.1609775076354));
#15313=CARTESIAN_POINT('Ctrl Pts',(0.0160467930153873,0.154720779732145,
1.16090166239918));
#15314=CARTESIAN_POINT('Ctrl Pts',(0.0165097953145605,0.154672059199608,
1.16086853771235));
#15315=CARTESIAN_POINT('Ctrl Pts',(0.0174722472861841,0.154566412144577,
1.16079951045634));
#15316=CARTESIAN_POINT('Ctrl Pts',(0.0179716529309728,0.154509141698687,
1.16076359745229));
#15317=CARTESIAN_POINT('Ctrl Pts',(0.0192639673169386,0.154354592508808,
1.16067041288259));
#15318=CARTESIAN_POINT('Ctrl Pts',(0.0200564112502258,0.154253625529255,
1.16061302601831));
#15319=CARTESIAN_POINT('Ctrl Pts',(0.0234566325922731,0.153793752068544,
1.16036570303146));
#15320=CARTESIAN_POINT('Ctrl Pts',(0.0260557021282155,0.153374804321913,
1.16017389184886));
#15321=CARTESIAN_POINT('Ctrl Pts',(0.0328878155923632,0.152094862297774,
1.15966197711718));
#15322=CARTESIAN_POINT('Ctrl Pts',(0.0370975267667694,0.151123203978766,
1.1593386086524));
#15323=CARTESIAN_POINT('Ctrl Pts',(0.0532192413900348,0.146687889726904,
1.15806980855491));
#15324=CARTESIAN_POINT('Ctrl Pts',(0.0647396495391824,0.14198013101031,
1.15709322072974));
#15325=CARTESIAN_POINT('Ctrl Pts',(0.0763174580160261,0.135543954120722,
1.1560839775288));
#15326=CARTESIAN_POINT('Ctrl Pts',(0.0770533692457254,0.135126963394234,
1.15601972133894));
#15327=CARTESIAN_POINT('Ctrl Pts',(0.0805744679824971,0.13309367773476,
1.15571187718268));
#15328=CARTESIAN_POINT('Ctrl Pts',(0.0833126727950094,0.131397010503638,
1.15547125955316));
#15329=CARTESIAN_POINT('Ctrl Pts',(0.086452731762303,0.129313678664958,
1.15519554652275));
#15330=CARTESIAN_POINT('Ctrl Pts',(0.0869074068190293,0.129008546162611,
1.15515562958001));
#15331=CARTESIAN_POINT('Ctrl Pts',(0.0876352692150949,0.128514483220765,
1.15509175020849));
#15332=CARTESIAN_POINT('Ctrl Pts',(0.0879094736650297,0.128327071397393,
1.15506769010618));
#15333=CARTESIAN_POINT('Ctrl Pts',(0.0883963962761222,0.127991978968315,
1.15502497672983));
#15334=CARTESIAN_POINT('Ctrl Pts',(0.0886093479428623,0.127844644064732,
1.15500630051377));
#15335=CARTESIAN_POINT('Ctrl Pts',(0.0890624049284862,0.127529511607132,
1.15496657625368));
#15336=CARTESIAN_POINT('Ctrl Pts',(0.0893024039862383,0.127361567784584,
1.15494553843046));
#15337=CARTESIAN_POINT('Ctrl Pts',(0.089954236164962,0.126902687685521,
1.15488841061848));
#15338=CARTESIAN_POINT('Ctrl Pts',(0.0903651363077546,0.126610421785932,
1.15485240995418));
#15339=CARTESIAN_POINT('Ctrl Pts',(0.0924679553092545,0.125099272379248,
1.15466819058106));
#15340=CARTESIAN_POINT('Ctrl Pts',(0.0941367669183605,0.123848378969873,
1.15452205037058));
#15341=CARTESIAN_POINT('Ctrl Pts',(0.0989812484015199,0.120062571378479,
1.15409630480898));
#15342=CARTESIAN_POINT('Ctrl Pts',(0.102083508069634,0.117436244459679,
1.15382168212832));
#15343=CARTESIAN_POINT('Ctrl Pts',(0.112762360953917,0.107652327060995,
1.1528544828009));
#15344=CARTESIAN_POINT('Ctrl Pts',(0.119718458835612,0.0998592747115928,
1.1521809658162));
#15345=CARTESIAN_POINT('Ctrl Pts',(0.129650173409336,0.0861892306737257,
1.1510508166205));
#15346=CARTESIAN_POINT('Ctrl Pts',(0.133125632428243,0.0807174054335912,
1.15061013908672));
#15347=CARTESIAN_POINT('Ctrl Pts',(0.136729381274919,0.0741745730719639,
1.15008676910077));
#15348=CARTESIAN_POINT('Ctrl Pts',(0.137200679315452,0.0732991439809676,
1.1500168215337));
#15349=CARTESIAN_POINT('Ctrl Pts',(0.137942912327108,0.071888215375048,
1.1499041821268));
#15350=CARTESIAN_POINT('Ctrl Pts',(0.138219202464033,0.0713555507513797,
1.14986167916771));
#15351=CARTESIAN_POINT('Ctrl Pts',(0.138704197110923,0.0704071345885378,
1.149786033466));
#15352=CARTESIAN_POINT('Ctrl Pts',(0.138914132934551,0.0699920178276809,
1.14975293433335));
#15353=CARTESIAN_POINT('Ctrl Pts',(0.139347548895304,0.0691253711555583,
1.14968385131716));
#15354=CARTESIAN_POINT('Ctrl Pts',(0.139570703379246,0.0686736854095561,
1.14964785655326));
#15355=CARTESIAN_POINT('Ctrl Pts',(0.140144250557256,0.0674984286022034,
1.14955422273499));
#15356=CARTESIAN_POINT('Ctrl Pts',(0.140491231068684,0.0667732190012126,
1.14949646627521));
#15357=CARTESIAN_POINT('Ctrl Pts',(0.141970290858724,0.0636193294008904,
1.1492453516703));
#15358=CARTESIAN_POINT('Ctrl Pts',(0.143045065787499,0.0611644509053154,
1.14905004635061));
#15359=CARTESIAN_POINT('Ctrl Pts',(0.145726137108539,0.0545829394362312,
1.14852643143988));
#15360=CARTESIAN_POINT('Ctrl Pts',(0.147220453331585,0.0504136460590183,
1.14819466807285));
#15361=CARTESIAN_POINT('Ctrl Pts',(0.15220152426085,0.0343946765982378,
1.14692049224163));
#15362=CARTESIAN_POINT('Ctrl Pts',(0.154450636942299,0.0222093985832487,
1.14594799416917));
#15363=CARTESIAN_POINT('Ctrl Pts',(0.155323824893923,0.00849969005322668,
1.14490215593787));
#15364=CARTESIAN_POINT('Ctrl Pts',(0.155393590976728,0.00711107859627856,
1.14479682981267));
#15365=CARTESIAN_POINT('Ctrl Pts',(0.155541279411767,0.00309872455081711,
1.1444945467261));
#15366=CARTESIAN_POINT('Ctrl Pts',(0.155571429467965,0.000473533873413159,
1.14429929940269));
#15367=CARTESIAN_POINT('Ctrl Pts',(0.155528005882422,-0.00266582157227178,
1.1440697725068));
#15368=CARTESIAN_POINT('Ctrl Pts',(0.155518337305567,-0.00318025158010444,
1.14403228854922));
#15369=CARTESIAN_POINT('Ctrl Pts',(0.155498379868171,-0.00402025461294613,
1.14397129989625));
#15370=CARTESIAN_POINT('Ctrl Pts',(0.155489620693745,-0.00434585441326615,
1.14394771318136));
#15371=CARTESIAN_POINT('Ctrl Pts',(0.155472096916919,-0.00492910086356511,
1.14390556109948));
#15372=CARTESIAN_POINT('Ctrl Pts',(0.155463714542212,-0.00518675421837981,
1.14388697482293));
#15373=CARTESIAN_POINT('Ctrl Pts',(0.155444162321329,-0.00574503226446389,
1.14384677799949));
#15374=CARTESIAN_POINT('Ctrl Pts',(0.155432760951465,-0.00604564493531247,
1.14382518056169));
#15375=CARTESIAN_POINT('Ctrl Pts',(0.155398449624585,-0.00688593695445099,
1.14376493692664));
#15376=CARTESIAN_POINT('Ctrl Pts',(0.155373600240654,-0.00742554003681481,
1.14372639718238));
#15377=CARTESIAN_POINT('Ctrl Pts',(0.155212459038221,-0.0105683635775332,
1.14350272447473));
#15378=CARTESIAN_POINT('Ctrl Pts',(0.155013546443811,-0.013168155818712,
1.14332087773324));
#15379=CARTESIAN_POINT('Ctrl Pts',(0.153259323998841,-0.0303909811588266,
1.14212996784765));
#15380=CARTESIAN_POINT('Ctrl Pts',(0.149702400890423,-0.0447362457528364,
1.14119776336399));
#15381=CARTESIAN_POINT('Ctrl Pts',(0.143461225765647,-0.0601529699931097,
1.14008029486486));
#15382=CARTESIAN_POINT('Ctrl Pts',(0.142706369311765,-0.061922490523329,
1.139950317881));
#15383=CARTESIAN_POINT('Ctrl Pts',(0.140282618866334,-0.0673243355060292,
1.13954747653858));
#15384=CARTESIAN_POINT('Ctrl Pts',(0.138506503880416,-0.0709064382457621,
1.13927172827274));
#15385=CARTESIAN_POINT('Ctrl Pts',(0.136179762983446,-0.0751772996682384,
1.13893027429809));
#15386=CARTESIAN_POINT('Ctrl Pts',(0.135758623082696,-0.0759351725890784,
1.13886918442797));
#15387=CARTESIAN_POINT('Ctrl Pts',(0.135051191831707,-0.0771835512987573,
1.13876770728354));
#15388=CARTESIAN_POINT('Ctrl Pts',(0.134768506581321,-0.077676087855746,
1.13872744926716));
#15389=CARTESIAN_POINT('Ctrl Pts',(0.134251748899673,-0.0785651476838894,
1.13865437359359));
#15390=CARTESIAN_POINT('Ctrl Pts',(0.13401859974567,-0.0789622025216168,
1.13862158956739));
#15391=CARTESIAN_POINT('Ctrl Pts',(0.133514228524791,-0.0798124818145884,
1.13855106098906));
#15392=CARTESIAN_POINT('Ctrl Pts',(0.133242454775471,-0.0802653705197622,
1.13851329668065));
#15393=CARTESIAN_POINT('Ctrl Pts',(0.132494057108027,-0.0814982384245717,
1.13840994454275));
#15394=CARTESIAN_POINT('Ctrl Pts',(0.132012862734086,-0.082275403625522,
1.13834419016624));
#15395=CARTESIAN_POINT('Ctrl Pts',(0.129418852359069,-0.0863835789277452,
1.13799332704225));
#15396=CARTESIAN_POINT('Ctrl Pts',(0.127186936864152,-0.0896372686180094,
1.1377038362538));
#15397=CARTESIAN_POINT('Ctrl Pts',(0.116021290579455,-0.104656841062771,
1.1363094611363));
#15398=CARTESIAN_POINT('Ctrl Pts',(0.105565367074166,-0.115194632027259,
1.13514499951444));
#15399=CARTESIAN_POINT('Ctrl Pts',(0.0902668802598648,-0.126756206626722,
1.1336799300187));
#15400=CARTESIAN_POINT('Ctrl Pts',(0.0866371621923835,-0.129264289969544,
1.13334771529968));
#15401=CARTESIAN_POINT('Ctrl Pts',(0.0823471793799926,-0.131966585728735,
1.13297633923749));
#15402=CARTESIAN_POINT('Ctrl Pts',(0.0817867472475284,-0.132314646646602,
1.13292822730454));
#15403=CARTESIAN_POINT('Ctrl Pts',(0.0809461743344661,-0.132829309881414,
1.13285668596281));
#15404=CARTESIAN_POINT('Ctrl Pts',(0.0806677067432171,-0.132998608252282,
1.13283308641053));
#15405=CARTESIAN_POINT('Ctrl Pts',(0.0801680005297435,-0.133300265013923,
1.13279092052415));
#15406=CARTESIAN_POINT('Ctrl Pts',(0.0799469640705385,-0.133432949083612,
1.13277233322123));
#15407=CARTESIAN_POINT('Ctrl Pts',(0.0794725849776099,-0.133716108071473,
1.13273257932045));
#15408=CARTESIAN_POINT('Ctrl Pts',(0.0792191451721574,-0.13386641237789,
1.13271142383295));
#15409=CARTESIAN_POINT('Ctrl Pts',(0.0785172623001348,-0.134279977746775,
1.13265306065199));
#15410=CARTESIAN_POINT('Ctrl Pts',(0.0780679181940378,-0.134541714989414,
1.13261595010682));
#15411=CARTESIAN_POINT('Ctrl Pts',(0.0770579626559391,-0.135123237881236,
1.13253308618868));
#15412=CARTESIAN_POINT('Ctrl Pts',(0.0764966526510069,-0.135441800026314,
1.13248740687318));
#15413=CARTESIAN_POINT('Ctrl Pts',(0.0747454207279084,-0.136421322714181,
1.13234599968118));
#15414=CARTESIAN_POINT('Ctrl Pts',(0.0735487578478895,-0.137070185442955,
1.13225095155387));
#15415=CARTESIAN_POINT('Ctrl Pts',(0.06883857314864,-0.139544724179392,
1.13188234282979));
#15416=CARTESIAN_POINT('Ctrl Pts',(0.06526413281883,-0.141251822571692,
1.13161444238228));
#15417=CARTESIAN_POINT('Ctrl Pts',(0.0519849262739079,-0.146981892733538,
1.13064773465753));
#15418=CARTESIAN_POINT('Ctrl Pts',(0.0419450048870137,-0.150155712891625,
1.12996913343594));
#15419=CARTESIAN_POINT('Ctrl Pts',(0.0252631104516602,-0.153623852135527,
1.12882988961763));
#15420=CARTESIAN_POINT('Ctrl Pts',(0.0187879596408262,-0.154549369007396,
1.12838536887849));
#15421=CARTESIAN_POINT('Ctrl Pts',(0.0112817900340348,-0.155143530793578,
1.12785780677971));
#15422=CARTESIAN_POINT('Ctrl Pts',(0.0102884767902182,-0.1552125674589,
1.12778775645848));
#15423=CARTESIAN_POINT('Ctrl Pts',(0.00869516897896647,-0.155307942902629,
1.12767498318806));
#15424=CARTESIAN_POINT('Ctrl Pts',(0.00809555361213224,-0.155340352406017,
1.12763244984327));
#15425=CARTESIAN_POINT('Ctrl Pts',(0.00703106321219006,-0.155391708620779,
1.12755676917574));
#15426=CARTESIAN_POINT('Ctrl Pts',(0.00656625970249629,-0.155412043236324,
1.12752366560146));
#15427=CARTESIAN_POINT('Ctrl Pts',(0.0055981576850239,-0.155450045834558,
1.12745459257405));
#15428=CARTESIAN_POINT('Ctrl Pts',(0.00509485138919411,-0.15546735540863,
1.12741861231931));
#15429=CARTESIAN_POINT('Ctrl Pts',(0.00378878336307197,-0.155505924314436,
1.1273250581996));
#15430=CARTESIAN_POINT('Ctrl Pts',(0.00298593414470183,-0.155523411513032,
1.12726736730399));
#15431=CARTESIAN_POINT('Ctrl Pts',(-0.000487867583251774,-0.15557216788484,
1.1270169295851));
#15432=CARTESIAN_POINT('Ctrl Pts',(-0.00315909247217263,-0.155540849702531,
1.12682224856852));
#15433=CARTESIAN_POINT('Ctrl Pts',(-0.0102328672689935,-0.155275628195431,
1.12630073125421));
#15434=CARTESIAN_POINT('Ctrl Pts',(-0.0146282716989421,-0.154923333642065,
1.12597047548947));
#15435=CARTESIAN_POINT('Ctrl Pts',(-0.0260239987464294,-0.153520693462305,
1.12509853558099));
#15436=CARTESIAN_POINT('Ctrl Pts',(-0.032977934394724,-0.152178491831197,
1.12455051349504));
#15437=CARTESIAN_POINT('Ctrl Pts',(-0.0486385558193611,-0.148031725065138,
1.12329418510298));
#15438=CARTESIAN_POINT('Ctrl Pts',(-0.057239789031957,-0.144923263589032,
1.12258754429739));
#15439=CARTESIAN_POINT('Ctrl Pts',(-0.0661404259855582,-0.140789612528867,
1.121868347043));
#15440=CARTESIAN_POINT('Ctrl Pts',(-0.0667592846064621,-0.140497220296242,
1.12181841273334));
#15441=CARTESIAN_POINT('Ctrl Pts',(-0.0676743675827402,-0.140057459287887,
1.12174470423906));
#15442=CARTESIAN_POINT('Ctrl Pts',(-0.0679720727886764,-0.139913220448408,
1.12172074469596));
#15443=CARTESIAN_POINT('Ctrl Pts',(-0.0685013363151543,-0.139654703100791,
1.12167818802388));
#15444=CARTESIAN_POINT('Ctrl Pts',(-0.0687330717253776,-0.139540797009703,
1.12165956826852));
#15445=CARTESIAN_POINT('Ctrl Pts',(-0.0692256081841168,-0.139297173377963,
1.12162002257628));
#15446=CARTESIAN_POINT('Ctrl Pts',(-0.0694863280482958,-0.139167300605119,
1.12159910655085));
#15447=CARTESIAN_POINT('Ctrl Pts',(-0.0701963730350758,-0.138811112019545,
1.12154218637856));
#15448=CARTESIAN_POINT('Ctrl Pts',(-0.0706449728533462,-0.138583344730476,
1.12150627137715));
#15449=CARTESIAN_POINT('Ctrl Pts',(-0.0716446162270851,-0.138069681067937,
1.12142632622767));
#15450=CARTESIAN_POINT('Ctrl Pts',(-0.0721950729448844,-0.137782652536816,
1.12138236329432));
#15451=CARTESIAN_POINT('Ctrl Pts',(-0.0738834156721675,-0.136889391948427,
1.12124765772941));
#15452=CARTESIAN_POINT('Ctrl Pts',(-0.0750155282569507,-0.136272284504057,
1.12115752268528));
#15453=CARTESIAN_POINT('Ctrl Pts',(-0.0793229668529194,-0.133854376152974,
1.12081480123757));
#15454=CARTESIAN_POINT('Ctrl Pts',(-0.0824424322483272,-0.13195596506273,
1.12056705880209));
#15455=CARTESIAN_POINT('Ctrl Pts',(-0.0934202578858593,-0.124733760884153,
1.11968617951262));
#15456=CARTESIAN_POINT('Ctrl Pts',(-0.100854403356595,-0.118803450949042,
1.11907118391773));
#15457=CARTESIAN_POINT('Ctrl Pts',(-0.113419725811636,-0.106745344595956,
1.11791478960237));
#15458=CARTESIAN_POINT('Ctrl Pts',(-0.118709038154767,-0.100830245741666,
1.11737985631687));
#15459=CARTESIAN_POINT('Ctrl Pts',(-0.124148939567688,-0.0937224601918963,
1.11675303801319));
#15460=CARTESIAN_POINT('Ctrl Pts',(-0.12476544876914,-0.0929001692356106,
1.11668076014295));
#15461=CARTESIAN_POINT('Ctrl Pts',(-0.125734729447746,-0.0915803048102074,
1.11656508825902));
#15462=CARTESIAN_POINT('Ctrl Pts',(-0.126092808844497,-0.0910866508165007,
1.11652189985285));
#15463=CARTESIAN_POINT('Ctrl Pts',(-0.126719783184938,-0.0902115118721126,
1.1164454612175));
#15464=CARTESIAN_POINT('Ctrl Pts',(-0.126989883235489,-0.0898308959759313,
1.11641225773307));
#15465=CARTESIAN_POINT('Ctrl Pts',(-0.12754551881558,-0.0890403990382476,
1.11634337949984));
#15466=CARTESIAN_POINT('Ctrl Pts',(-0.127830800625397,-0.0886303471253588,
1.11630769558946));
#15467=CARTESIAN_POINT('Ctrl Pts',(-0.128559050824582,-0.0875727610082243,
1.11621577209192));
#15468=CARTESIAN_POINT('Ctrl Pts',(-0.12899909959997,-0.086923243612193,
1.11615942304626));
#15469=CARTESIAN_POINT('Ctrl Pts',(-0.130822948536014,-0.0841868665323108,
1.11592244302159));
#15470=CARTESIAN_POINT('Ctrl Pts',(-0.132161095769767,-0.0820701880659587,
1.11574012628876));
#15471=CARTESIAN_POINT('Ctrl Pts',(-0.136111454279218,-0.0754742086738379,
1.11517459898141));
#15472=CARTESIAN_POINT('Ctrl Pts',(-0.138551054097449,-0.0708962541165567,
1.1147855490348));
#15473=CARTESIAN_POINT('Ctrl Pts',(-0.14506078784016,-0.0570561214165265,
1.11362037035487));
#15474=CARTESIAN_POINT('Ctrl Pts',(-0.148461737401086,-0.0475091711978216,
1.11282885262876));
#15475=CARTESIAN_POINT('Ctrl Pts',(-0.151408433680578,-0.0357139079813251,
1.11189417581377));
#15476=CARTESIAN_POINT('Ctrl Pts',(-0.151865550194059,-0.0337172400337054,
1.11173747911819));
#15477=CARTESIAN_POINT('Ctrl Pts',(-0.152298128320758,-0.0316399752128557,
1.11157636335709));
#15478=CARTESIAN_POINT('Ctrl Pts',(-0.152313088284246,-0.0315678801763142,
1.11157077392979));
#15479=CARTESIAN_POINT('Ctrl Pts',(-0.153035949009394,-0.0280717944816777,
1.11129984302843));
#15480=CARTESIAN_POINT('Ctrl Pts',(-0.153628327122837,-0.0246245666204027,
1.11103806087691));
#15481=CARTESIAN_POINT('Ctrl Pts',(-0.154180355191951,-0.0206042526620967,
1.11074105418904));
#15482=CARTESIAN_POINT('Ctrl Pts',(-0.154253656785587,-0.020048105866898,
1.11070015146496));
#15483=CARTESIAN_POINT('Ctrl Pts',(-0.154366061112768,-0.0191581475115949,
1.11063500393307));
#15484=CARTESIAN_POINT('Ctrl Pts',(-0.154407092428787,-0.0188245917093234,
1.11061065529324));
#15485=CARTESIAN_POINT('Ctrl Pts',(-0.154477885216618,-0.0182332880964603,
1.11056761638991));
#15486=CARTESIAN_POINT('Ctrl Pts',(-0.154508083188542,-0.0179755959403103,
1.11054890189106));
#15487=CARTESIAN_POINT('Ctrl Pts',(-0.15456518562475,-0.0174775395335369,
1.11051281326533));
#15488=CARTESIAN_POINT('Ctrl Pts',(-0.154592174130371,-0.0172371893065659,
1.11049543435578));
#15489=CARTESIAN_POINT('Ctrl Pts',(-0.154649991288702,-0.016711230218809,
1.11045748215791));
#15490=CARTESIAN_POINT('Ctrl Pts',(-0.154680589660553,-0.016425596087944,
1.11043692170671));
#15491=CARTESIAN_POINT('Ctrl Pts',(-0.154753828119392,-0.0157235614993409,
1.11038650804981));
#15492=CARTESIAN_POINT('Ctrl Pts',(-0.154795579406378,-0.0153070673436705,
1.11035670296449));
#15493=CARTESIAN_POINT('Ctrl Pts',(-0.154974907011376,-0.0134423558667297,
1.11022370399947));
#15494=CARTESIAN_POINT('Ctrl Pts',(-0.155093850599082,-0.0119923575481582,
1.11012147967001));
#15495=CARTESIAN_POINT('Ctrl Pts',(-0.155428335971539,-0.00706773879775331,
1.10977769098852));
#15496=CARTESIAN_POINT('Ctrl Pts',(-0.155547593982592,-0.00358745805535069,
1.10954044697179));
#15497=CARTESIAN_POINT('Ctrl Pts',(-0.155549963960585,-0.000105886074850944,
1.10930622288127));
#15498=CARTESIAN_POINT('Ctrl Pts',(-0.155549963809809,-0.00010610733808079,
1.10930623776684));
#15499=CARTESIAN_POINT('Ctrl Pts',(-0.155557297589873,0.0106449796676609,
1.10858295385663));
#15500=CARTESIAN_POINT('Ctrl Pts',(-0.154450027858621,0.0213687656586557,
1.1078892507296));
#15501=CARTESIAN_POINT('Ctrl Pts',(-0.150893360043952,0.038346658686023,
1.10673341008683));
#15502=CARTESIAN_POINT('Ctrl Pts',(-0.14913277537527,0.0447064921555321,
1.10628718600213));
#15503=CARTESIAN_POINT('Ctrl Pts',(-0.14647918261692,0.0523635131565579,
1.10572229128449));
#15504=CARTESIAN_POINT('Ctrl Pts',(-0.145963312060206,0.053784753421134,
1.10561625172379));
#15505=CARTESIAN_POINT('Ctrl Pts',(-0.145197686054202,0.0558018943052019,
1.10546394518654));
#15506=CARTESIAN_POINT('Ctrl Pts',(-0.144964796317964,0.0564041421290725,
1.1054182397703));
#15507=CARTESIAN_POINT('Ctrl Pts',(-0.144555575186568,0.0574431020995894,
1.10533898121703));
#15508=CARTESIAN_POINT('Ctrl Pts',(-0.144380996280835,0.057880499310008,
1.10530548718048));
#15509=CARTESIAN_POINT('Ctrl Pts',(-0.144042236611525,0.0587181721893201,
1.1052410952041));
#15510=CARTESIAN_POINT('Ctrl Pts',(-0.143878366682379,0.059118569562777,
1.10521020799942));
#15511=CARTESIAN_POINT('Ctrl Pts',(-0.143446377233992,0.0601616513187481,
1.10512945611869));
#15512=CARTESIAN_POINT('Ctrl Pts',(-0.143175611114379,0.0608032218204263,
1.10507950230247));
#15513=CARTESIAN_POINT('Ctrl Pts',(-0.142229802399612,0.0630029306735668,
1.10490722883331));
#15514=CARTESIAN_POINT('Ctrl Pts',(-0.141533580788642,0.0645517702961384,
1.10478419273612));
#15515=CARTESIAN_POINT('Ctrl Pts',(-0.135434836821106,0.0775460561328283,
1.10373676204873));
#15516=CARTESIAN_POINT('Ctrl Pts',(-0.12868040533795,0.0883017650519376,
1.10276325893813));
#15517=CARTESIAN_POINT('Ctrl Pts',(-0.117272301066173,0.102335456757039,
1.10136071046782));
#15518=CARTESIAN_POINT('Ctrl Pts',(-0.11362536184951,0.106370209338636,
1.1009396706719));
#15519=CARTESIAN_POINT('Ctrl Pts',(-0.107933257392616,0.112040031229894,
1.10032846571767));
#15520=CARTESIAN_POINT('Ctrl Pts',(-0.106046174224259,0.113827796977805,
1.10013259529038));
#15521=CARTESIAN_POINT('Ctrl Pts',(-0.103356146547034,0.116251248891357,
1.09986358740521));
#15522=CARTESIAN_POINT('Ctrl Pts',(-0.102590493756333,0.11692748448397,
1.09978812704633));
#15523=CARTESIAN_POINT('Ctrl Pts',(-0.101253718857317,0.118084903552562,
1.09965835845616));
#15524=CARTESIAN_POINT('Ctrl Pts',(-0.100685700719042,0.118569598802221,
1.09960382346366));
#15525=CARTESIAN_POINT('Ctrl Pts',(-0.0998511425306055,0.119271413047385,
1.09952460492108));
#15526=CARTESIAN_POINT('Ctrl Pts',(-0.0995873498925043,0.119491758638643,
1.09949969576395));
#15527=CARTESIAN_POINT('Ctrl Pts',(-0.0991328597054476,0.119868843138172,
1.0994570068369));
#15528=CARTESIAN_POINT('Ctrl Pts',(-0.0989425166166196,0.120026004840455,
1.09943919653723));
#15529=CARTESIAN_POINT('Ctrl Pts',(-0.0985607538428087,0.120339691876037,
1.09940361226414));
#15530=CARTESIAN_POINT('Ctrl Pts',(-0.0983693351604216,0.120496213804917,
1.09938583841196));
#15531=CARTESIAN_POINT('Ctrl Pts',(-0.0978503814734785,0.120918498385561,
1.09933783391876));
#15532=CARTESIAN_POINT('Ctrl Pts',(-0.0975221340960157,0.121183389038653,
1.09930766562779));
#15533=CARTESIAN_POINT('Ctrl Pts',(-0.0962914216806294,0.122168316204022,
1.0991952645309));
#15534=CARTESIAN_POINT('Ctrl Pts',(-0.0953819964486638,0.122879657947254,
1.099113625682));
#15535=CARTESIAN_POINT('Ctrl Pts',(-0.0943523951287159,0.123666681103683,
1.09902266898451));
#15536=CARTESIAN_POINT('Ctrl Pts',(-0.0942399730443125,0.123752373563864,
1.09901275689679));
#15537=CARTESIAN_POINT('Ctrl Pts',(-0.0846948556055197,0.131007481372158,
1.09817281245617));
#15538=CARTESIAN_POINT('Ctrl Pts',(-0.0744813799541116,0.137070312887174,
1.09740716183172));
#15539=CARTESIAN_POINT('Ctrl Pts',(-0.0636886243721053,0.141913923297148,
1.09662690323004));
#15540=CARTESIAN_POINT('Ctrl Pts',(-0.0636886366174998,0.141913917801617,
1.08266645291));
#15541=CARTESIAN_POINT('Ctrl Pts',(-0.0654970691897544,0.141102322950838,
1.08280290121822));
#15542=CARTESIAN_POINT('Ctrl Pts',(-0.0672904848875035,0.140255937755946,
1.08294043971035));
#15543=CARTESIAN_POINT('Ctrl Pts',(-0.0701743012142742,0.13882685165615,
1.08316555758902));
#15544=CARTESIAN_POINT('Ctrl Pts',(-0.071274125431853,0.138265419322431,
1.08325236506509));
#15545=CARTESIAN_POINT('Ctrl Pts',(-0.0728937038206069,0.137414207154768,
1.0833816715481));
#15546=CARTESIAN_POINT('Ctrl Pts',(-0.0734186874626417,0.137134432941225,
1.08342381851927));
#15547=CARTESIAN_POINT('Ctrl Pts',(-0.0743493718815002,0.136631576695086,
1.08349895736458));
#15548=CARTESIAN_POINT('Ctrl Pts',(-0.0747557082670035,0.136409680456959,
1.0835319068682));
#15549=CARTESIAN_POINT('Ctrl Pts',(-0.0756084554011755,0.135939049288522,
1.08360136231955));
#15550=CARTESIAN_POINT('Ctrl Pts',(-0.0760546422768576,0.135689922345981,
1.0836378819665));
#15551=CARTESIAN_POINT('Ctrl Pts',(-0.0772283949122343,0.135026953361931,
1.08373442801632));
#15552=CARTESIAN_POINT('Ctrl Pts',(-0.0779538531808934,0.134609434432828,
1.08379458589444));
#15553=CARTESIAN_POINT('Ctrl Pts',(-0.0809989196872986,0.132824053168718,
1.08404918492504));
#15554=CARTESIAN_POINT('Ctrl Pts',(-0.0832860409962447,0.13140200829151,
1.08424557731263));
#15555=CARTESIAN_POINT('Ctrl Pts',(-0.0858571109904579,0.129709320179458,
1.08447252063562));
#15556=CARTESIAN_POINT('Ctrl Pts',(-0.0861784533760765,0.129496044024315,
1.08450099723456));
#15557=CARTESIAN_POINT('Ctrl Pts',(-0.0865619328377933,0.129239467723725,
1.08453511521819));
#15558=CARTESIAN_POINT('Ctrl Pts',(-0.0866248381435066,0.129197312861768,
1.08454071623207));
#15559=CARTESIAN_POINT('Ctrl Pts',(-0.0995119509813744,0.120547602334531,
1.08568906360688));
#15560=CARTESIAN_POINT('Ctrl Pts',(-0.110981311560037,0.110078664137978,
1.08690544180326));
#15561=CARTESIAN_POINT('Ctrl Pts',(-0.122742773812635,0.0956050415601197,
1.08833260506456));
#15562=CARTESIAN_POINT('Ctrl Pts',(-0.124690236484937,0.0930508487712888,
1.08857598900644));
#15563=CARTESIAN_POINT('Ctrl Pts',(-0.1272445532835,0.0894763831246984,
1.08890345243883));
#15564=CARTESIAN_POINT('Ctrl Pts',(-0.12792078492832,0.0885069063442847,
1.08899099433548));
#15565=CARTESIAN_POINT('Ctrl Pts',(-0.129062753524451,0.0868292934410465,
1.08914018600276));
#15566=CARTESIAN_POINT('Ctrl Pts',(-0.129533864614918,0.0861249008798765,
1.08920214705632));
#15567=CARTESIAN_POINT('Ctrl Pts',(-0.130197325078922,0.0851151526237553,
1.08928996333155));
#15568=CARTESIAN_POINT('Ctrl Pts',(-0.130394393414508,0.0848129402689565,
1.08931611919851));
#15569=CARTESIAN_POINT('Ctrl Pts',(-0.130732892256682,0.0842898698441625,
1.0893611672181));
#15570=CARTESIAN_POINT('Ctrl Pts',(-0.130874818165653,0.0840693359715489,
1.08938009207611));
#15571=CARTESIAN_POINT('Ctrl Pts',(-0.131149402518108,0.0836402880933896,
1.08941677711718));
#15572=CARTESIAN_POINT('Ctrl Pts',(-0.131282121688672,0.0834318170751442,
1.08943454150564));
#15573=CARTESIAN_POINT('Ctrl Pts',(-0.131639795992465,0.0828670270762352,
1.08948250773189));
#15574=CARTESIAN_POINT('Ctrl Pts',(-0.131863803253786,0.0825101052478858,
1.08951264736445));
#15575=CARTESIAN_POINT('Ctrl Pts',(-0.132694979999661,0.0811737196676346,
1.08962486970617));
#15576=CARTESIAN_POINT('Ctrl Pts',(-0.133292730079633,0.0801883956627173,
1.08970636075761));
#15577=CARTESIAN_POINT('Ctrl Pts',(-0.138763553081534,0.070940118128965,
1.09046054936208));
#15578=CARTESIAN_POINT('Ctrl Pts',(-0.142874200578925,0.0622482607887882,
1.09109120771017));
#15579=CARTESIAN_POINT('Ctrl Pts',(-0.150265617844189,0.0419537071894152,
1.09251280278583));
#15580=CARTESIAN_POINT('Ctrl Pts',(-0.153053454945115,0.0302399418655237,
1.09330186117327));
#15581=CARTESIAN_POINT('Ctrl Pts',(-0.154632764489578,0.0169260068846493,
1.09423762266343));
#15582=CARTESIAN_POINT('Ctrl Pts',(-0.154779513253198,0.015526867417129,
1.09433637251524));
#15583=CARTESIAN_POINT('Ctrl Pts',(-0.154964209771534,0.0135014608116345,
1.09448000137529));
#15584=CARTESIAN_POINT('Ctrl Pts',(-0.155017380769496,0.0128766219444452,
1.09452440383715));
#15585=CARTESIAN_POINT('Ctrl Pts',(-0.155103604872675,0.0117852855643695,
1.09460212636834));
#15586=CARTESIAN_POINT('Ctrl Pts',(-0.155138335437228,0.0113189252740619,
1.0946353935317));
#15587=CARTESIAN_POINT('Ctrl Pts',(-0.155201448455145,0.0104165175495574,
1.09469987320782));
#15588=CARTESIAN_POINT('Ctrl Pts',(-0.155230097597034,0.00998049263660528,
1.09473107704891));
#15589=CARTESIAN_POINT('Ctrl Pts',(-0.155293853886368,0.00894337672181383,
1.09480541603011));
#15590=CARTESIAN_POINT('Ctrl Pts',(-0.155327308623873,0.00834219508496718,
1.09484860244059));
#15591=CARTESIAN_POINT('Ctrl Pts',(-0.155433880402022,0.00620331918078968,
1.09500259714848));
#15592=CARTESIAN_POINT('Ctrl Pts',(-0.155487657697881,0.00466479716371283,
1.09511400571974));
#15593=CARTESIAN_POINT('Ctrl Pts',(-0.155539991536784,0.00206100437931375,
1.0953036963907));
#15594=CARTESIAN_POINT('Ctrl Pts',(-0.155550456350694,0.000996061320335559,
1.09538160219944));
#15595=CARTESIAN_POINT('Ctrl Pts',(-0.155548320038231,-0.00382820720160956,
1.09573602022358));
#15596=CARTESIAN_POINT('Ctrl Pts',(-0.155410374330263,-0.00758592816398812,
1.0960162512148));
#15597=CARTESIAN_POINT('Ctrl Pts',(-0.1545687886761,-0.0191046024222937,
1.09688802402212));
#15598=CARTESIAN_POINT('Ctrl Pts',(-0.153418226475811,-0.0268201758129123,
1.09749050156596));
#15599=CARTESIAN_POINT('Ctrl Pts',(-0.149765464875519,-0.0429202412377183,
1.09877084722375));
#15600=CARTESIAN_POINT('Ctrl Pts',(-0.147124210951748,-0.0512478577203565,
1.09944698107082));
#15601=CARTESIAN_POINT('Ctrl Pts',(-0.143355590093591,-0.0603848213541838,
1.10017766026405));
#15602=CARTESIAN_POINT('Ctrl Pts',(-0.142900633083672,-0.0614537317166153,
1.10026294405026));
#15603=CARTESIAN_POINT('Ctrl Pts',(-0.142263790529776,-0.0629046514851802,
1.1003783419895));
#15604=CARTESIAN_POINT('Ctrl Pts',(-0.142092274432174,-0.0632911275963539,
1.10040904449476));
#15605=CARTESIAN_POINT('Ctrl Pts',(-0.141817899775513,-0.0639026370033217,
1.10045756213078));
#15606=CARTESIAN_POINT('Ctrl Pts',(-0.14171607827137,-0.0641281285743524,
1.1004754393913));
#15607=CARTESIAN_POINT('Ctrl Pts',(-0.141505287899192,-0.0645919862475548,
1.10051218553325));
#15608=CARTESIAN_POINT('Ctrl Pts',(-0.141396254598972,-0.0648303198927974,
1.10053104987745));
#15609=CARTESIAN_POINT('Ctrl Pts',(-0.141136109539516,-0.0653951874454223,
1.10057572372054));
#15610=CARTESIAN_POINT('Ctrl Pts',(-0.140984464961606,-0.0657214774902751,
1.10060150060297));
#15611=CARTESIAN_POINT('Ctrl Pts',(-0.140474295765508,-0.0668093047137703,
1.10068735327252));
#15612=CARTESIAN_POINT('Ctrl Pts',(-0.140110713797553,-0.0675684758645069,
1.10074712753213));
#15613=CARTESIAN_POINT('Ctrl Pts',(-0.136584216494592,-0.0747810405082375,
1.1013140307224));
#15614=CARTESIAN_POINT('Ctrl Pts',(-0.13298329564159,-0.0810118923922004,
1.10179637340532));
#15615=CARTESIAN_POINT('Ctrl Pts',(-0.126302044105769,-0.0909189660146076,
1.10258794454168));
#15616=CARTESIAN_POINT('Ctrl Pts',(-0.123460514987323,-0.0947415813628541,
1.10290014561543));
#15617=CARTESIAN_POINT('Ctrl Pts',(-0.113816903159399,-0.106542654680463,
1.10390441927588));
#15618=CARTESIAN_POINT('Ctrl Pts',(-0.106383781919192,-0.113965191530275,
1.10460166598278));
#15619=CARTESIAN_POINT('Ctrl Pts',(-0.0973779838983343,-0.121303876758094,
1.1054150942691));
#15620=CARTESIAN_POINT('Ctrl Pts',(-0.0964863206428485,-0.122014310926978,
1.10549529538561));
#15621=CARTESIAN_POINT('Ctrl Pts',(-0.0951264112834025,-0.123073592449157,
1.10561715360899));
#15622=CARTESIAN_POINT('Ctrl Pts',(-0.0946638632870458,-0.123429721917901,
1.10565852234625));
#15623=CARTESIAN_POINT('Ctrl Pts',(-0.0938319116942235,-0.124062838998831,
1.10573279451285));
#15624=CARTESIAN_POINT('Ctrl Pts',(-0.0934632567380556,-0.124340803054096,
1.10576565916038));
#15625=CARTESIAN_POINT('Ctrl Pts',(-0.0926789475219452,-0.124926709639521,
1.10583548258261));
#15626=CARTESIAN_POINT('Ctrl Pts',(-0.0922629846139647,-0.125234227563094,
1.10587245734721));
#15627=CARTESIAN_POINT('Ctrl Pts',(-0.0911471488572198,-0.126050579080165,
1.10597149849921));
#15628=CARTESIAN_POINT('Ctrl Pts',(-0.0904445599742132,-0.126555650787017,
1.10603370884472));
#15629=CARTESIAN_POINT('Ctrl Pts',(-0.0870249032633656,-0.128970926971719,
1.1063358131559));
#15630=CARTESIAN_POINT('Ctrl Pts',(-0.0842515360231853,-0.130799500496015,
1.10657876839933));
#15631=CARTESIAN_POINT('Ctrl Pts',(-0.0686782772003354,-0.14036662284719,
1.10793332792345));
#15632=CARTESIAN_POINT('Ctrl Pts',(-0.054873220017387,-0.146315602695528,
1.10910968644308));
#15633=CARTESIAN_POINT('Ctrl Pts',(-0.0394448751007813,-0.15046912965479,
1.11033419412863));
#15634=CARTESIAN_POINT('Ctrl Pts',(-0.0384505822440917,-0.15072627492771,
1.11041267761977));
#15635=CARTESIAN_POINT('Ctrl Pts',(-0.0365365399051327,-0.151201114067557,
1.11056285619434));
#15636=CARTESIAN_POINT('Ctrl Pts',(-0.035617208046781,-0.151420309760325,
1.11063459045438));
#15637=CARTESIAN_POINT('Ctrl Pts',(-0.0317070461640164,-0.152315024873353,
1.1109378676337));
#15638=CARTESIAN_POINT('Ctrl Pts',(-0.0286983292024785,-0.152910473376288,
1.11116671455371));
#15639=CARTESIAN_POINT('Ctrl Pts',(-0.0251415121431128,-0.153505693844402,
1.11143051998525));
#15640=CARTESIAN_POINT('Ctrl Pts',(-0.0246088356718649,-0.153591988415209,
1.11146985146595));
#15641=CARTESIAN_POINT('Ctrl Pts',(-0.0237464616207541,-0.15372709301235,
1.1115332300835));
#15642=CARTESIAN_POINT('Ctrl Pts',(-0.0234170436193986,-0.153777617484842,
1.11155737011441));
#15643=CARTESIAN_POINT('Ctrl Pts',(-0.022831939179184,-0.153865434116311,
1.11160011994497));
#15644=CARTESIAN_POINT('Ctrl Pts',(-0.0225763202332963,-0.153903148216975,
1.11161875322072));
#15645=CARTESIAN_POINT('Ctrl Pts',(-0.022028188874875,-0.153982624663333,
1.11165861600681));
#15646=CARTESIAN_POINT('Ctrl Pts',(-0.021735651804616,-0.154024190463421,
1.11167983431728));
#15647=CARTESIAN_POINT('Ctrl Pts',(-0.0209318936926681,-0.154136058763158,
1.11173798211519));
#15648=CARTESIAN_POINT('Ctrl Pts',(-0.0204204321123242,-0.154204652190425,
1.11177481677605));
#15649=CARTESIAN_POINT('Ctrl Pts',(-0.0176833070480242,-0.154557878092712,
1.11197109406447));
#15650=CARTESIAN_POINT('Ctrl Pts',(-0.0154518743723241,-0.154796892807306,
1.11212811977314));
#15651=CARTESIAN_POINT('Ctrl Pts',(-0.00868775871410813,-0.155373673695075,
1.11259723580076));
#15652=CARTESIAN_POINT('Ctrl Pts',(-0.00414446113626913,-0.155561198042398,
1.11290305958846));
#15653=CARTESIAN_POINT('Ctrl Pts',(0.0113174035813567,-0.155521348501438,
1.11393170312614));
#15654=CARTESIAN_POINT('Ctrl Pts',(0.0222003559781261,-0.154344161504432,
1.11463728493112));
#15655=CARTESIAN_POINT('Ctrl Pts',(0.0381502817294884,-0.150895784237119,
1.11573609851731));
#15656=CARTESIAN_POINT('Ctrl Pts',(0.0433664588106869,-0.149480169757907,
1.11610582392226));
#15657=CARTESIAN_POINT('Ctrl Pts',(0.0493998566978678,-0.147500364522822,
1.11655104744773));
#15658=CARTESIAN_POINT('Ctrl Pts',(0.0502989439486908,-0.147196194050595,
1.11661785749473));
#15659=CARTESIAN_POINT('Ctrl Pts',(0.0517550911289746,-0.146688665666304,
1.11672684465253));
#15660=CARTESIAN_POINT('Ctrl Pts',(0.052313880831915,-0.146490313493395,
1.11676885654466));
#15661=CARTESIAN_POINT('Ctrl Pts',(0.0533067076934562,-0.146131487181524,
1.11684384386904));
#15662=CARTESIAN_POINT('Ctrl Pts',(0.0537411911567228,-0.145972261048395,
1.11687677755471));
#15663=CARTESIAN_POINT('Ctrl Pts',(0.0546549514227546,-0.145632760696325,
1.11694629158622));
#15664=CARTESIAN_POINT('Ctrl Pts',(0.0551340605323534,-0.1454520541646,
1.1169828860135));
#15665=CARTESIAN_POINT('Ctrl Pts',(0.0563983032747887,-0.144968073366379,
1.11707984187247));
#15666=CARTESIAN_POINT('Ctrl Pts',(0.0571818731949512,-0.144660790244102,
1.11714033679843));
#15667=CARTESIAN_POINT('Ctrl Pts',(0.0608006923555885,-0.1432076461129,
1.11742162981614));
#15668=CARTESIAN_POINT('Ctrl Pts',(0.0636040664325067,-0.141984768098211,
1.11764500199353));
#15669=CARTESIAN_POINT('Ctrl Pts',(0.0794316034484524,-0.134517728496603,
1.11893895879046));
#15670=CARTESIAN_POINT('Ctrl Pts',(0.0915701824792191,-0.126566735119113,
1.1200704520659));
#15671=CARTESIAN_POINT('Ctrl Pts',(0.106731728029147,-0.113299339923834,
1.12162072573471));
#15672=CARTESIAN_POINT('Ctrl Pts',(0.110818815718578,-0.109305120442082,
1.12205446270915));
#15673=CARTESIAN_POINT('Ctrl Pts',(0.115144697854957,-0.104584795121255,
1.12252375486159));
#15674=CARTESIAN_POINT('Ctrl Pts',(0.115608573557686,-0.104071795327169,
1.12257421775728));
#15675=CARTESIAN_POINT('Ctrl Pts',(0.116290145892974,-0.103307864118604,
1.12264854876261));
#15676=CARTESIAN_POINT('Ctrl Pts',(0.116510476461629,-0.103059311567851,
1.12267260677771));
#15677=CARTESIAN_POINT('Ctrl Pts',(0.116900715102366,-0.102616236593141,
1.12271526622882));
#15678=CARTESIAN_POINT('Ctrl Pts',(0.117070936076066,-0.102421995362803,
1.12273389076476));
#15679=CARTESIAN_POINT('Ctrl Pts',(0.117435331978952,-0.102004083404415,
1.12277379591227));
#15680=CARTESIAN_POINT('Ctrl Pts',(0.117629351609803,-0.101780282334224,
1.12279506506013));
#15681=CARTESIAN_POINT('Ctrl Pts',(0.118161765155601,-0.101162588994287,
1.12285349540955));
#15682=CARTESIAN_POINT('Ctrl Pts',(0.118498831983934,-0.100767549318997,
1.12289056024653));
#15683=CARTESIAN_POINT('Ctrl Pts',(0.120311211755843,-0.0986217843385661,
1.12309029984792));
#15684=CARTESIAN_POINT('Ctrl Pts',(0.121749814844777,-0.0968402194555562,
1.12325045558052));
#15685=CARTESIAN_POINT('Ctrl Pts',(0.131871453724246,-0.0837233075298303,
1.12439468636902));
#15686=CARTESIAN_POINT('Ctrl Pts',(0.138997340849035,-0.0712707743269609,
1.12530193213362));
#15687=CARTESIAN_POINT('Ctrl Pts',(0.146734909735347,-0.052023356075842,
1.12668953372001));
#15688=CARTESIAN_POINT('Ctrl Pts',(0.148769016498788,-0.0458838287626516,
1.12712926028703));
#15689=CARTESIAN_POINT('Ctrl Pts',(0.150668539235068,-0.0386753296758805,
1.12765157865191));
#15690=CARTESIAN_POINT('Ctrl Pts',(0.150912516359792,-0.037712095746547,
1.12772148587669));
#15691=CARTESIAN_POINT('Ctrl Pts',(0.151288935602114,-0.036163796979812,
1.12783406573565));
#15692=CARTESIAN_POINT('Ctrl Pts',(0.151427253957926,-0.0355801768986072,
1.12787654973777));
#15693=CARTESIAN_POINT('Ctrl Pts',(0.151666812982498,-0.0345426777461856,
1.1279521649268));
#15694=CARTESIAN_POINT('Ctrl Pts',(0.151769400792548,-0.0340891144006268,
1.127985252556));
#15695=CARTESIAN_POINT('Ctrl Pts',(0.151978863791308,-0.033143342471659,
1.12805431477707));
#15696=CARTESIAN_POINT('Ctrl Pts',(0.152085385009902,-0.032651061925674,
1.12809030025567));
#15697=CARTESIAN_POINT('Ctrl Pts',(0.152355696446327,-0.0313718091724201,
1.12818391681753));
#15698=CARTESIAN_POINT('Ctrl Pts',(0.152515778791782,-0.0305840779639932,
1.12824166529263));
#15699=CARTESIAN_POINT('Ctrl Pts',(0.153183102045879,-0.0271647276782974,
1.12849280687957));
#15700=CARTESIAN_POINT('Ctrl Pts',(0.153628359806295,-0.0245216350459134,
1.12868814800275));
#15701=CARTESIAN_POINT('Ctrl Pts',(0.154627755927137,-0.0174835642627882,
1.12921191354052));
#15702=CARTESIAN_POINT('Ctrl Pts',(0.155062794237672,-0.0130744419771307,
1.12954379478179));
#15703=CARTESIAN_POINT('Ctrl Pts',(0.155995907612279,0.00367337566344355,
1.13081785208543));
#15704=CARTESIAN_POINT('Ctrl Pts',(0.155212788901227,0.0160363950270534,
1.13179008482513));
#15705=CARTESIAN_POINT('Ctrl Pts',(0.152729909648759,0.0295166937569477,
1.13283361576225));
#15706=CARTESIAN_POINT('Ctrl Pts',(0.152465383301336,0.0308539727840429,
1.13293689479962));
#15707=CARTESIAN_POINT('Ctrl Pts',(0.151634849969303,0.0347807378250339,
1.13323914784211));
#15708=CARTESIAN_POINT('Ctrl Pts',(0.151020162428184,0.0373596072769394,
1.13343634854853));
#15709=CARTESIAN_POINT('Ctrl Pts',(0.150207384422566,0.0404204208364463,
1.13366787515993));
#15710=CARTESIAN_POINT('Ctrl Pts',(0.150072470524546,0.0409184844107916,
1.13370546889491));
#15711=CARTESIAN_POINT('Ctrl Pts',(0.149848248961683,0.0417302184649313,
1.13376659609405));
#15712=CARTESIAN_POINT('Ctrl Pts',(0.149760430391615,0.0420442902691618,
1.13379021222501));
#15713=CARTESIAN_POINT('Ctrl Pts',(0.149601437383147,0.0426060895181119,
1.13383239049407));
#15714=CARTESIAN_POINT('Ctrl Pts',(0.149530634688674,0.0428539172570351,
1.13385097369971));
#15715=CARTESIAN_POINT('Ctrl Pts',(0.149375990598862,0.0433901618087672,
1.1338911335101));
#15716=CARTESIAN_POINT('Ctrl Pts',(0.149291929990211,0.0436785113430009,
1.13391269714872));
#15717=CARTESIAN_POINT('Ctrl Pts',(0.149054896327362,0.0444829191098029,
1.13397277100443));
#15718=CARTESIAN_POINT('Ctrl Pts',(0.148900077098037,0.0449984363591205,
1.13401117569352));
#15719=CARTESIAN_POINT('Ctrl Pts',(0.147988441625811,0.0479777734246798,
1.13423263703831));
#15720=CARTESIAN_POINT('Ctrl Pts',(0.147173100554912,0.0504234683713321,
1.1344124825393));
#15721=CARTESIAN_POINT('Ctrl Pts',(0.141295478657645,0.0666942989391085,
1.13560298809118));
#15722=CARTESIAN_POINT('Ctrl Pts',(0.134352915397266,0.0797618053906868,
1.13653620171133));
#15723=CARTESIAN_POINT('Ctrl Pts',(0.124575945899856,0.0931671546948407,
1.13765086756548));
#15724=CARTESIAN_POINT('Ctrl Pts',(0.123449287116668,0.0946549424866219,
1.1377769226277));
#15725=CARTESIAN_POINT('Ctrl Pts',(0.119786144102283,0.0993155618988308,
1.13818004678914));
#15726=CARTESIAN_POINT('Ctrl Pts',(0.1171522105003,0.102409256447219,1.13846015962333));
#15727=CARTESIAN_POINT('Ctrl Pts',(0.113810100500386,0.106036892565904,
1.13880643057292));
#15728=CARTESIAN_POINT('Ctrl Pts',(0.113214411024951,0.106672670549852,
1.13886781431207));
#15729=CARTESIAN_POINT('Ctrl Pts',(0.112220835139746,0.107715414597813,
1.13896967166337));
#15730=CARTESIAN_POINT('Ctrl Pts',(0.111825994234747,0.10812526707127,1.13901001423389));
#15731=CARTESIAN_POINT('Ctrl Pts',(0.111107681329752,0.108862746684649,
1.13908317045316));
#15732=CARTESIAN_POINT('Ctrl Pts',(0.110784985388753,0.109191123587312,
1.13911595004324));
#15733=CARTESIAN_POINT('Ctrl Pts',(0.110089805059015,0.109892288335531,
1.13918638816027));
#15734=CARTESIAN_POINT('Ctrl Pts',(0.109716875492065,0.11026462457738,1.1392240660799));
#15735=CARTESIAN_POINT('Ctrl Pts',(0.108695440519839,0.11127412206478,1.13932697528191));
#15736=CARTESIAN_POINT('Ctrl Pts',(0.108043238536512,0.111907495604359,
1.13939237079232));
#15737=CARTESIAN_POINT('Ctrl Pts',(0.104579814027607,0.115212434965544,
1.13973805650465));
#15738=CARTESIAN_POINT('Ctrl Pts',(0.101675203216065,0.117783660829944,
1.14002257688992));
#15739=CARTESIAN_POINT('Ctrl Pts',(0.0872274311655971,0.129640222111979,
1.14141430982126));
#15740=CARTESIAN_POINT('Ctrl Pts',(0.0744942070606635,0.137352385128099,
1.14258187299207));
#15741=CARTESIAN_POINT('Ctrl Pts',(0.0567792200499203,0.144884982216121,
1.1440529171158));
#15742=CARTESIAN_POINT('Ctrl Pts',(0.0526179139068107,0.146447608911285,
1.14438769208398));
#15743=CARTESIAN_POINT('Ctrl Pts',(0.0477671107435503,0.148035610836402,
1.14476156410014));
#15744=CARTESIAN_POINT('Ctrl Pts',(0.0471379405001526,0.148237153075328,
1.14480974540904));
#15745=CARTESIAN_POINT('Ctrl Pts',(0.0461963888526278,0.148532159623132,
1.1448813648493));
#15746=CARTESIAN_POINT('Ctrl Pts',(0.0458849778270189,0.148628656726924,
1.14490497371427));
#15747=CARTESIAN_POINT('Ctrl Pts',(0.0453268368369209,0.14879968679282,
1.14494714415859));
#15748=CARTESIAN_POINT('Ctrl Pts',(0.0450802240279438,0.148874585918513,
1.14496572677196));
#15749=CARTESIAN_POINT('Ctrl Pts',(0.0445724622848307,0.149027421552716,
1.14500388366486));
#15750=CARTESIAN_POINT('Ctrl Pts',(0.0443112957304139,0.149105284422075,
1.14502345362964));
#15751=CARTESIAN_POINT('Ctrl Pts',(0.0435911318489811,0.149317931159207,
1.14507726697012));
#15752=CARTESIAN_POINT('Ctrl Pts',(0.0431317099502381,0.149451286225563,
1.14511142839477));
#15753=CARTESIAN_POINT('Ctrl Pts',(0.0421022664970025,0.149744957390049,
1.145187614446));
#15754=CARTESIAN_POINT('Ctrl Pts',(0.0415319263577029,0.149904143471119,
1.14522957701373));
#15755=CARTESIAN_POINT('Ctrl Pts',(0.0397961477847074,0.150377944854073,
1.14535657780777));
#15756=CARTESIAN_POINT('Ctrl Pts',(0.0386279112955131,0.15068226294323,
1.14544108615236));
#15757=CARTESIAN_POINT('Ctrl Pts',(0.034241787156889,0.151770454972918,
1.14575517427765));
#15758=CARTESIAN_POINT('Ctrl Pts',(0.0310024672085833,0.152465148008552,
1.14598073843499));
#15759=CARTESIAN_POINT('Ctrl Pts',(0.0164935159925448,0.155095067480247,
1.14697269925986));
#15760=CARTESIAN_POINT('Ctrl Pts',(0.00505301496596258,0.155887808668048,
1.14770856466844));
#15761=CARTESIAN_POINT('Ctrl Pts',(-0.0128930684129306,0.155152097511481,
1.14890955191355));
#15762=CARTESIAN_POINT('Ctrl Pts',(-0.0193904999980737,0.154474578282769,
1.14935353084091));
#15763=CARTESIAN_POINT('Ctrl Pts',(-0.0268070803942238,0.153225890617847,
1.14988048785086));
#15764=CARTESIAN_POINT('Ctrl Pts',(-0.027786933810309,0.153051231105118,
1.1499505095955));
#15765=CARTESIAN_POINT('Ctrl Pts',(-0.0293549441356074,0.152756178542819,
1.15006323864751));
#15766=CARTESIAN_POINT('Ctrl Pts',(-0.0299442093835759,0.152641760780974,
1.15010575651673));
#15767=CARTESIAN_POINT('Ctrl Pts',(-0.0309888378146968,0.152432643304446,
1.1501814106755));
#15768=CARTESIAN_POINT('Ctrl Pts',(-0.0314444690969005,0.152339306052311,
1.15021450325304));
#15769=CARTESIAN_POINT('Ctrl Pts',(-0.0323924233716294,0.152140681191502,
1.15028355432998));
#15770=CARTESIAN_POINT('Ctrl Pts',(-0.0328846667390771,0.152035044143676,
1.15031952362833));
#15771=CARTESIAN_POINT('Ctrl Pts',(-0.0341605116953441,0.151754757660172,
1.15041305131401));
#15772=CARTESIAN_POINT('Ctrl Pts',(-0.0349432807678018,0.151576429949095,
1.15047072667533));
#15773=CARTESIAN_POINT('Ctrl Pts',(-0.0383238783407153,0.150778696094525,
1.15072111324251));
#15774=CARTESIAN_POINT('Ctrl Pts',(-0.0409067486221699,0.150098538038684,
1.15091575797927));
#15775=CARTESIAN_POINT('Ctrl Pts',(-0.0477022978524671,0.148120615611087,
1.15143718354508));
#15776=CARTESIAN_POINT('Ctrl Pts',(-0.0518792533930157,0.146709789773049,
1.1517673829189));
#15777=CARTESIAN_POINT('Ctrl Pts',(-0.0585866146441732,0.14412201433543,
1.15231334060707));
#15778=CARTESIAN_POINT('Ctrl Pts',(-0.0611535904857956,0.143051605183529,
1.15252616729451));
#15779=CARTESIAN_POINT('Ctrl Pts',(-0.0636886503124892,0.14191391165553,
1.15273999320994));
#15780=CARTESIAN_POINT('Origin',(0.,0.,-0.129405622560373));
#15781=CARTESIAN_POINT('',(-0.063688617770428,0.141913926259872,1.23669476364274));
#15782=CARTESIAN_POINT('',(-0.0636886258329928,0.141913922641526,1.22279509470766));
#15783=CARTESIAN_POINT('',(-0.0636886258329924,0.141913922641526,-0.129405622560373));
#15784=CARTESIAN_POINT('Ctrl Pts',(-0.063688617770428,0.141913926259872,
1.23669476364274));
#15785=CARTESIAN_POINT('Ctrl Pts',(-0.0619802210974833,0.14268062636867,
1.23655225137014));
#15786=CARTESIAN_POINT('Ctrl Pts',(-0.0602576689874724,0.143416616927621,
1.2364089803923));
#15787=CARTESIAN_POINT('Ctrl Pts',(-0.049519912432359,0.147776775471332,
1.23551896995172));
#15788=CARTESIAN_POINT('Ctrl Pts',(-0.0401957081937531,0.15058053366981,
1.23475765945508));
#15789=CARTESIAN_POINT('Ctrl Pts',(-0.0277979561050489,0.153074049098719,
1.23379236394043));
#15790=CARTESIAN_POINT('Ctrl Pts',(-0.0249089320833586,0.153570629986059,
1.23357078671092));
#15791=CARTESIAN_POINT('Ctrl Pts',(-0.0209083663318317,0.154142386404852,
1.23326999052332));
#15792=CARTESIAN_POINT('Ctrl Pts',(-0.0198076328172458,0.154287695320831,
1.23318785437603));
#15793=CARTESIAN_POINT('Ctrl Pts',(-0.0179041886797547,0.154518263921758,
1.23304700410495));
#15794=CARTESIAN_POINT('Ctrl Pts',(-0.01710221149343,0.154609082188135,
1.23298802146388));
#15795=CARTESIAN_POINT('Ctrl Pts',(-0.015947708175783,0.154730728248995,
1.2329036656448));
#15796=CARTESIAN_POINT('Ctrl Pts',(-0.0155957453002853,0.154766599742278,
1.23287802278838));
#15797=CARTESIAN_POINT('Ctrl Pts',(-0.0149837427781496,0.154826865122191,
1.23283356627658));
#15798=CARTESIAN_POINT('Ctrl Pts',(-0.0147237600480891,0.154851805303272,
1.2328147222889));
#15799=CARTESIAN_POINT('Ctrl Pts',(-0.0142154178984678,0.154899278825929,
1.23277795891429));
#15800=CARTESIAN_POINT('Ctrl Pts',(-0.0139670676371253,0.154921869698375,
1.23276003624387));
#15801=CARTESIAN_POINT('Ctrl Pts',(-0.0132878934394813,0.154982003484026,
1.23271112370259));
#15802=CARTESIAN_POINT('Ctrl Pts',(-0.0128569610276343,0.155018347563041,
1.2326802004149));
#15803=CARTESIAN_POINT('Ctrl Pts',(-0.0112083343221554,0.155150467834646,
1.23256230323861));
#15804=CARTESIAN_POINT('Ctrl Pts',(-0.00998963530012164,0.155233700792277,
1.23247599911868));
#15805=CARTESIAN_POINT('Ctrl Pts',(-0.00825669940367521,0.155331560752508,
1.23235431942471));
#15806=CARTESIAN_POINT('Ctrl Pts',(-0.00774321797879547,0.155358004115675,
1.23231839454185));
#15807=CARTESIAN_POINT('Ctrl Pts',(0.00891379943519178,0.156133021579668,
1.23115694221173));
#15808=CARTESIAN_POINT('Ctrl Pts',(0.0250778714235947,0.154364029266605,
1.23014056897496));
#15809=CARTESIAN_POINT('Ctrl Pts',(0.0441742869932295,0.149189576965858,
1.22880824125981));
#15810=CARTESIAN_POINT('Ctrl Pts',(0.0476327197820298,0.14812163384217,
1.22856187345984));
#15811=CARTESIAN_POINT('Ctrl Pts',(0.0532362918842732,0.146174737072919,
1.22815190921912));
#15812=CARTESIAN_POINT('Ctrl Pts',(0.0554046816553065,0.145366697700235,
1.22799055424427));
#15813=CARTESIAN_POINT('Ctrl Pts',(0.0580831598197573,0.144299942100431,
1.22778748592316));
#15814=CARTESIAN_POINT('Ctrl Pts',(0.0586110054833854,0.144086351767268,
1.22774728357157));
#15815=CARTESIAN_POINT('Ctrl Pts',(0.0596311942272293,0.143667003538852,
1.22766921930849));
#15816=CARTESIAN_POINT('Ctrl Pts',(0.0601236753954979,0.143461600698028,
1.22763136974784));
#15817=CARTESIAN_POINT('Ctrl Pts',(0.0610292022110306,0.143078444131952,
1.22756146581913));
#15818=CARTESIAN_POINT('Ctrl Pts',(0.0614425542000458,0.142901424847058,
1.22752943664127));
#15819=CARTESIAN_POINT('Ctrl Pts',(0.0623547264745322,0.142506094838405,
1.22745848745755));
#15820=CARTESIAN_POINT('Ctrl Pts',(0.0628531777807489,0.142286953051706,
1.22741953946881));
#15821=CARTESIAN_POINT('Ctrl Pts',(0.0642128445064391,0.141680643307619,
1.22731280313361));
#15822=CARTESIAN_POINT('Ctrl Pts',(0.0650716890100894,0.14128824899465,
1.2272448367346));
#15823=CARTESIAN_POINT('Ctrl Pts',(0.0695513385731975,0.139192050424392,
1.22688740760547));
#15824=CARTESIAN_POINT('Ctrl Pts',(0.0731086525740806,0.13735696225473,
1.22659344783234));
#15825=CARTESIAN_POINT('Ctrl Pts',(0.0782668027717617,0.134438897707471,
1.22615143937549));
#15826=CARTESIAN_POINT('Ctrl Pts',(0.0799248063603882,0.133459860711217,
1.22600685624823));
#15827=CARTESIAN_POINT('Ctrl Pts',(0.094103027330795,0.124728780074457,
1.22474876560777));
#15828=CARTESIAN_POINT('Ctrl Pts',(0.105480051346796,0.115267208218718,
1.2235809571384));
#15829=CARTESIAN_POINT('Ctrl Pts',(0.117090789467428,0.102431591022558,
1.22227904061027));
#15830=CARTESIAN_POINT('Ctrl Pts',(0.118776873488069,0.100471589366699,
1.22208693209259));
#15831=CARTESIAN_POINT('Ctrl Pts',(0.120754546619859,0.0980532115760005,
1.22185871814389));
#15832=CARTESIAN_POINT('Ctrl Pts',(0.121093483359897,0.0976343235784191,
1.22181949992813));
#15833=CARTESIAN_POINT('Ctrl Pts',(0.121618066498002,0.0969790633141017,
1.22175864463112));
#15834=CARTESIAN_POINT('Ctrl Pts',(0.121805211580056,0.0967439055243859,
1.22173690314216));
#15835=CARTESIAN_POINT('Ctrl Pts',(0.122151636086156,0.0963060059019595,
1.22169660127609));
#15836=CARTESIAN_POINT('Ctrl Pts',(0.122311091405146,0.0961034124911095,
1.22167802871997));
#15837=CARTESIAN_POINT('Ctrl Pts',(0.122671100029508,0.0956436619132668,
1.22163604559286));
#15838=CARTESIAN_POINT('Ctrl Pts',(0.122871348429918,0.0953862704320105,
1.22161265671647));
#15839=CARTESIAN_POINT('Ctrl Pts',(0.123474905406152,0.0946054273645897,
1.22154204413177));
#15840=CARTESIAN_POINT('Ctrl Pts',(0.123875696463312,0.0940800245497745,
1.22149499384077));
#15841=CARTESIAN_POINT('Ctrl Pts',(0.126945161957871,0.0900025936559428,
1.22113327094287));
#15842=CARTESIAN_POINT('Ctrl Pts',(0.129464211722795,0.08633984106592,1.22082820814525));
#15843=CARTESIAN_POINT('Ctrl Pts',(0.139694322214312,0.0700082002312593,
1.21952793523499));
#15844=CARTESIAN_POINT('Ctrl Pts',(0.145728490340589,0.0563817964781705,
1.21858522679993));
#15845=CARTESIAN_POINT('Ctrl Pts',(0.150788030555051,0.03838864017662,1.21731136853533));
#15846=CARTESIAN_POINT('Ctrl Pts',(0.151694555985656,0.034633441164891,
1.21704455748844));
#15847=CARTESIAN_POINT('Ctrl Pts',(0.152640472689856,0.0299585274104973,
1.2167094165039));
#15848=CARTESIAN_POINT('Ctrl Pts',(0.15281277791523,0.0290668558830159,
1.21664536334146));
#15849=CARTESIAN_POINT('Ctrl Pts',(0.153072691823266,0.0276555802289996,
1.21654375704728));
#15850=CARTESIAN_POINT('Ctrl Pts',(0.153165487275325,0.0271369415209088,
1.2165063687731));
#15851=CARTESIAN_POINT('Ctrl Pts',(0.153334459092464,0.0261640647630248,
1.21643613967267));
#15852=CARTESIAN_POINT('Ctrl Pts',(0.153411256601335,0.0257099391232977,
1.21640331892501));
#15853=CARTESIAN_POINT('Ctrl Pts',(0.153578529731744,0.0246933642653808,
1.21632975858325));
#15854=CARTESIAN_POINT('Ctrl Pts',(0.153667934237563,0.024130748113193,
1.21628898558493));
#15855=CARTESIAN_POINT('Ctrl Pts',(0.153886481342392,0.0227049576631806,
1.21618549570191));
#15856=CARTESIAN_POINT('Ctrl Pts',(0.154011451859404,0.0218411739809905,
1.21612264820548));
#15857=CARTESIAN_POINT('Ctrl Pts',(0.154679355500181,0.0169335914477857,
1.21576468219993));
#15858=CARTESIAN_POINT('Ctrl Pts',(0.155070238804793,0.0128710845264202,
1.21546483867438));
#15859=CARTESIAN_POINT('Ctrl Pts',(0.15601372391043,-0.00378271351719459,
1.21421995094));
#15860=CARTESIAN_POINT('Ctrl Pts',(0.155194907269087,-0.0164023279397902,
1.21323498107176));
#15861=CARTESIAN_POINT('Ctrl Pts',(0.152051684110817,-0.0330962051367237,
1.21192481969369));
#15862=CARTESIAN_POINT('Ctrl Pts',(0.151057076281337,-0.0373743146290311,
1.21158901203215));
#15863=CARTESIAN_POINT('Ctrl Pts',(0.149295878405311,-0.043719071150448,
1.21109577630508));
#15864=CARTESIAN_POINT('Ctrl Pts',(0.148664320762149,-0.0458207111110437,
1.21093321511738));
#15865=CARTESIAN_POINT('Ctrl Pts',(0.147830613952849,-0.0483960199098577,
1.21073560195031));
#15866=CARTESIAN_POINT('Ctrl Pts',(0.147670352748653,-0.0488828405868441,
1.21069831709535));
#15867=CARTESIAN_POINT('Ctrl Pts',(0.147414135819535,-0.0496483830546644,
1.21063980657225));
#15868=CARTESIAN_POINT('Ctrl Pts',(0.147319790961125,-0.049927633375557,
1.21061848892346));
#15869=CARTESIAN_POINT('Ctrl Pts',(0.147141180875861,-0.0504513852073031,
1.21057855641658));
#15870=CARTESIAN_POINT('Ctrl Pts',(0.147057100701039,-0.05069594178788,
1.21055993148729));
#15871=CARTESIAN_POINT('Ctrl Pts',(0.146862806008311,-0.0512565188318028,
1.21051728555815));
#15872=CARTESIAN_POINT('Ctrl Pts',(0.146752181294994,-0.0515723937999081,
1.21049328907719));
#15873=CARTESIAN_POINT('Ctrl Pts',(0.146405596872808,-0.0525518767356506,
1.21041897692424));
#15874=CARTESIAN_POINT('Ctrl Pts',(0.146166144504838,-0.0532142536816687,
1.21036886243302));
#15875=CARTESIAN_POINT('Ctrl Pts',(0.1434115636404,-0.0606751261007935,
1.20980571108014));
#15876=CARTESIAN_POINT('Ctrl Pts',(0.140428243654262,-0.0672925627789582,
1.20931853588003));
#15877=CARTESIAN_POINT('Ctrl Pts',(0.136093794934221,-0.07535177962701,
1.20871199222262));
#15878=CARTESIAN_POINT('Ctrl Pts',(0.135163340672948,-0.0770083322369855,
1.20858658693945));
#15879=CARTESIAN_POINT('Ctrl Pts',(0.129414885904463,-0.0868174051934478,
1.20783732797264));
#15880=CARTESIAN_POINT('Ctrl Pts',(0.123891349658511,-0.0945324911768807,
1.20721852541187));
#15881=CARTESIAN_POINT('Ctrl Pts',(0.114844748748526,-0.105002712583112,
1.20627924981462));
#15882=CARTESIAN_POINT('Ctrl Pts',(0.111850965231517,-0.1081861427167,1.20597831166449));
#15883=CARTESIAN_POINT('Ctrl Pts',(0.108053577769304,-0.111897786817798,
1.2056053941144));
#15884=CARTESIAN_POINT('Ctrl Pts',(0.10737377445929,-0.112550268112186,
1.20553896142489));
#15885=CARTESIAN_POINT('Ctrl Pts',(0.106299235923427,-0.113563024269175,
1.20543443593749));
#15886=CARTESIAN_POINT('Ctrl Pts',(0.105908492122233,-0.113927517845795,
1.20539652455456));
#15887=CARTESIAN_POINT('Ctrl Pts',(0.10521187139343,-0.114570658622869,
1.20532910452442));
#15888=CARTESIAN_POINT('Ctrl Pts',(0.10490674446966,-0.114850113879322,
1.20529963059205));
#15889=CARTESIAN_POINT('Ctrl Pts',(0.104200542576868,-0.115491737597227,
1.20523154231391));
#15890=CARTESIAN_POINT('Ctrl Pts',(0.103798690028157,-0.115853038205152,
1.20519289194903));
#15891=CARTESIAN_POINT('Ctrl Pts',(0.102689790031226,-0.116839635536465,
1.20508648855512));
#15892=CARTESIAN_POINT('Ctrl Pts',(0.101978931240855,-0.117460593046961,
1.20501855632836));
#15893=CARTESIAN_POINT('Ctrl Pts',(0.0983036401510497,-0.120612564199263,
1.20466869132767));
#15894=CARTESIAN_POINT('Ctrl Pts',(0.095250734055821,-0.123037754119059,
1.20438250495474));
#15895=CARTESIAN_POINT('Ctrl Pts',(0.0904873900737765,-0.126538098902295,
1.20394200573127));
#15896=CARTESIAN_POINT('Ctrl Pts',(0.0888416159541147,-0.127698961976856,
1.20379085199413));
#15897=CARTESIAN_POINT('Ctrl Pts',(0.0750395186498058,-0.137038440380648,
1.20253192966964));
#15898=CARTESIAN_POINT('Ctrl Pts',(0.0618080310699531,-0.14349269137093,
1.20137042903056));
#15899=CARTESIAN_POINT('Ctrl Pts',(0.0453215735089315,-0.148825176660276,
1.20006580648903));
#15900=CARTESIAN_POINT('Ctrl Pts',(0.0427517391774704,-0.14958365345524,
1.19986657262076));
#15901=CARTESIAN_POINT('Ctrl Pts',(0.0396373991530571,-0.150416008195807,
1.19963105173685));
#15902=CARTESIAN_POINT('Ctrl Pts',(0.0391106593704193,-0.150553828515318,
1.19959141943221));
#15903=CARTESIAN_POINT('Ctrl Pts',(0.0382908663155733,-0.150763732761255,
1.19953006280081));
#15904=CARTESIAN_POINT('Ctrl Pts',(0.0379983157392788,-0.150837732562223,
1.19950823131869));
#15905=CARTESIAN_POINT('Ctrl Pts',(0.0374555311002822,-0.150973348975197,
1.19946784745641));
#15906=CARTESIAN_POINT('Ctrl Pts',(0.0372053616262849,-0.151035194504373,
1.19944928245664));
#15907=CARTESIAN_POINT('Ctrl Pts',(0.0366398570429438,-0.15117350513304,
1.19940742380824));
#15908=CARTESIAN_POINT('Ctrl Pts',(0.0363244363437008,-0.151249605314718,
1.19938415131125));
#15909=CARTESIAN_POINT('Ctrl Pts',(0.0353941045564056,-0.151470984274584,
1.19931572357958));
#15910=CARTESIAN_POINT('Ctrl Pts',(0.0347785336515983,-0.151613506482938,
1.19927072273528));
#15911=CARTESIAN_POINT('Ctrl Pts',(0.0303707580449849,-0.152605774027785,
1.19895035011309));
#15912=CARTESIAN_POINT('Ctrl Pts',(0.0265483514580583,-0.153316981129975,
1.19868231307047));
#15913=CARTESIAN_POINT('Ctrl Pts',(0.0215548149647822,-0.154053689659205,
1.19834002032633));
#15914=CARTESIAN_POINT('Ctrl Pts',(0.0204048210574672,-0.15421022254997,
1.19826172911738));
#15915=CARTESIAN_POINT('Ctrl Pts',(0.00446546950208221,-0.156198399855704,
1.1971827054929));
#15916=CARTESIAN_POINT('Ctrl Pts',(-0.0105101323408154,-0.155908463312189,
1.19623359751688));
#15917=CARTESIAN_POINT('Ctrl Pts',(-0.0284731120979938,-0.152957436135887,
1.1949870518704));
#15918=CARTESIAN_POINT('Ctrl Pts',(-0.0317118146184209,-0.152318920204246,
1.19475829833807));
#15919=CARTESIAN_POINT('Ctrl Pts',(-0.035769185809653,-0.151383994455983,
1.19446553096438));
#15920=CARTESIAN_POINT('Ctrl Pts',(-0.0366091589639963,-0.151183060747679,
1.19440458436024));
#15921=CARTESIAN_POINT('Ctrl Pts',(-0.0379492361250728,-0.150850672224008,
1.19430679258056));
#15922=CARTESIAN_POINT('Ctrl Pts',(-0.0384504426153417,-0.150723698481175,
1.1942700916753));
#15923=CARTESIAN_POINT('Ctrl Pts',(-0.0393982147852614,-0.150478558444309,
1.19420044862472));
#15924=CARTESIAN_POINT('Ctrl Pts',(-0.0398449063300372,-0.150360896880929,
1.19416752309115));
#15925=CARTESIAN_POINT('Ctrl Pts',(-0.0408557687123586,-0.150089808081514,
1.19409277717798));
#15926=CARTESIAN_POINT('Ctrl Pts',(-0.0414196091152278,-0.149935186965903,
1.1940509185778));
#15927=CARTESIAN_POINT('Ctrl Pts',(-0.043083862066403,-0.14946869737273,
1.19392686526356));
#15928=CARTESIAN_POINT('Ctrl Pts',(-0.0441817003601429,-0.149147872556758,
1.19384438143269));
#15929=CARTESIAN_POINT('Ctrl Pts',(-0.053882677392569,-0.146196420891749,
1.19310957500982));
#15930=CARTESIAN_POINT('Ctrl Pts',(-0.062244394346004,-0.142836673773181,
1.19243306582289));
#15931=CARTESIAN_POINT('Ctrl Pts',(-0.0722167194573638,-0.137787229550308,
1.19157367999377));
#15932=CARTESIAN_POINT('Ctrl Pts',(-0.0741447109484442,-0.136759411591685,
1.1914050161732));
#15933=CARTESIAN_POINT('Ctrl Pts',(-0.0820255930790969,-0.132342445727668,
1.19070586767833));
#15934=CARTESIAN_POINT('Ctrl Pts',(-0.0877731821701352,-0.128602463025855,
1.19017221128851));
#15935=CARTESIAN_POINT('Ctrl Pts',(-0.0958176736424423,-0.122576600687255,
1.18940312245267));
#15936=CARTESIAN_POINT('Ctrl Pts',(-0.098320053272869,-0.120578686991808,
1.18916050196915));
#15937=CARTESIAN_POINT('Ctrl Pts',(-0.101657803967322,-0.117740752355734,
1.18883396093112));
#15938=CARTESIAN_POINT('Ctrl Pts',(-0.102547762045985,-0.116966450663619,
1.18874659791094));
#15939=CARTESIAN_POINT('Ctrl Pts',(-0.104060824349233,-0.115619475999487,
1.18859767749402));
#15940=CARTESIAN_POINT('Ctrl Pts',(-0.104688208673864,-0.115051716396478,
1.18853581032601));
#15941=CARTESIAN_POINT('Ctrl Pts',(-0.105576358938092,-0.114234692579732,
1.18844809796628));
#15942=CARTESIAN_POINT('Ctrl Pts',(-0.105840924016965,-0.113989610779967,
1.18842195315675));
#15943=CARTESIAN_POINT('Ctrl Pts',(-0.10629643498847,-0.113564691721451,
1.18837691335344));
#15944=CARTESIAN_POINT('Ctrl Pts',(-0.106487781665436,-0.113385288540765,
1.18835798572348));
#15945=CARTESIAN_POINT('Ctrl Pts',(-0.106858648442976,-0.113035803642193,
1.18832128653134));
#15946=CARTESIAN_POINT('Ctrl Pts',(-0.107038216592967,-0.11286577799774,
1.18830351079552));
#15947=CARTESIAN_POINT('Ctrl Pts',(-0.107523063210476,-0.112404499014242,
1.18825549475797));
#15948=CARTESIAN_POINT('Ctrl Pts',(-0.107827566462819,-0.112112427690842,
1.18822531685948));
#15949=CARTESIAN_POINT('Ctrl Pts',(-0.108961442778839,-0.111015951073513,
1.18811284382975));
#15950=CARTESIAN_POINT('Ctrl Pts',(-0.109783061779411,-0.110203525181222,
1.18803114362674));
#15951=CARTESIAN_POINT('Ctrl Pts',(-0.117246506674956,-0.102657273156656,
1.18728623390129));
#15952=CARTESIAN_POINT('Ctrl Pts',(-0.12327134052086,-0.0953388315933695,
1.18666385947147));
#15953=CARTESIAN_POINT('Ctrl Pts',(-0.135465683443261,-0.0774209234427562,
1.1852372146688));
#15954=CARTESIAN_POINT('Ctrl Pts',(-0.141122963392481,-0.0665522584193492,
1.18443499002265));
#15955=CARTESIAN_POINT('Ctrl Pts',(-0.145930685351747,-0.0538690057411872,
1.18348768209875));
#15956=CARTESIAN_POINT('Ctrl Pts',(-0.146393910136079,-0.0525971251904986,
1.18339262430345));
#15957=CARTESIAN_POINT('Ctrl Pts',(-0.147044198216264,-0.050736452392353,
1.18325339859662));
#15958=CARTESIAN_POINT('Ctrl Pts',(-0.147244455766494,-0.0501523085864997,
1.18320966673442));
#15959=CARTESIAN_POINT('Ctrl Pts',(-0.147589803111224,-0.0491250436512505,
1.18313271302091));
#15960=CARTESIAN_POINT('Ctrl Pts',(-0.147736389696134,-0.0486824305785562,
1.18309954088138));
#15961=CARTESIAN_POINT('Ctrl Pts',(-0.148017398269068,-0.0478209766126687,
1.18303494510264));
#15962=CARTESIAN_POINT('Ctrl Pts',(-0.148152038073715,-0.0474022109379951,
1.18300352897577));
#15963=CARTESIAN_POINT('Ctrl Pts',(-0.148470013382179,-0.0463986340477675,
1.182928200616));
#15964=CARTESIAN_POINT('Ctrl Pts',(-0.148651671152288,-0.0458133032961269,
1.18288423395795));
#15965=CARTESIAN_POINT('Ctrl Pts',(-0.149296628477842,-0.0436909189728369,
1.18272468669071));
#15966=CARTESIAN_POINT('Ctrl Pts',(-0.149739570847545,-0.042147837890083,
1.18260844787047));
#15967=CARTESIAN_POINT('Ctrl Pts',(-0.153749221781477,-0.027317553069109,
1.1814886068959));
#15968=CARTESIAN_POINT('Ctrl Pts',(-0.155561372408739,-0.0136219463444048,
1.180425675306));
#15969=CARTESIAN_POINT('Ctrl Pts',(-0.155546145707511,0.00470322754191661,
1.17900566089395));
#15970=CARTESIAN_POINT('Ctrl Pts',(-0.155340598153982,0.00927506209337149,
1.17865239274666));
#15971=CARTESIAN_POINT('Ctrl Pts',(-0.154604355622536,0.0175221551153412,
1.17802297719083));
#15972=CARTESIAN_POINT('Ctrl Pts',(-0.154143062027286,0.0212003486761419,
1.1777451365529));
#15973=CARTESIAN_POINT('Ctrl Pts',(-0.153459731382905,0.0254212079748754,
1.1774321256691));
#15974=CARTESIAN_POINT('Ctrl Pts',(-0.153365608226058,0.0259830177487437,
1.17739058327479));
#15975=CARTESIAN_POINT('Ctrl Pts',(-0.153210617183231,0.0268779451206424,
1.17732461425008));
#15976=CARTESIAN_POINT('Ctrl Pts',(-0.153151745350456,0.0272113956569777,
1.17730007970307));
#15977=CARTESIAN_POINT('Ctrl Pts',(-0.153045778928927,0.0278003515984167,
1.17725682932418));
#15978=CARTESIAN_POINT('Ctrl Pts',(-0.152999132509397,0.0280559343562187,
1.17723808842471));
#15979=CARTESIAN_POINT('Ctrl Pts',(-0.15289920112623,0.028595811821361,
1.17719856145606));
#15980=CARTESIAN_POINT('Ctrl Pts',(-0.152845763592181,0.0288800746954604,
1.17717778419618));
#15981=CARTESIAN_POINT('Ctrl Pts',(-0.152700101637927,0.0296431993785588,
1.17712209597818));
#15982=CARTESIAN_POINT('Ctrl Pts',(-0.152606416675189,0.0301217847467337,
1.17708726687379));
#15983=CARTESIAN_POINT('Ctrl Pts',(-0.152139775951923,0.0324475286485161,
1.1769184383847));
#15984=CARTESIAN_POINT('Ctrl Pts',(-0.151735504739387,0.0342883508820558,
1.17678612513213));
#15985=CARTESIAN_POINT('Ctrl Pts',(-0.150486139297179,0.0395214228458968,
1.17641255207618));
#15986=CARTESIAN_POINT('Ctrl Pts',(-0.149559983868727,0.0428933099273924,
1.17617493976527));
#15987=CARTESIAN_POINT('Ctrl Pts',(-0.147778643598194,0.0486159671845375,
1.17577253304438));
#15988=CARTESIAN_POINT('Ctrl Pts',(-0.146979024622191,0.0509824172356096,
1.17560638874482));
#15989=CARTESIAN_POINT('Ctrl Pts',(-0.146030370902248,0.0535817681064151,
1.17542318066258));
#15990=CARTESIAN_POINT('Ctrl Pts',(-0.145937337713217,0.0538346408989314,
1.17540535012595));
#15991=CARTESIAN_POINT('Ctrl Pts',(-0.140900274802583,0.0674168316221702,
1.17444718201298));
#15992=CARTESIAN_POINT('Ctrl Pts',(-0.134153700911123,0.0800041192216123,
1.17352759854769));
#15993=CARTESIAN_POINT('Ctrl Pts',(-0.124878851177497,0.0927549672484988,
1.17242943214729));
#15994=CARTESIAN_POINT('Ctrl Pts',(-0.123947166271319,0.0939963355126361,
1.17232065427079));
#15995=CARTESIAN_POINT('Ctrl Pts',(-0.122627142882841,0.0957013663978207,
1.17216851787292));
#15996=CARTESIAN_POINT('Ctrl Pts',(-0.12225441801618,0.0961770500637115,
1.17212577251591));
#15997=CARTESIAN_POINT('Ctrl Pts',(-0.121607013823502,0.0969934441650213,
1.1720518822928));
#15998=CARTESIAN_POINT('Ctrl Pts',(-0.121333648908475,0.0973351922866325,
1.17202078990518));
#15999=CARTESIAN_POINT('Ctrl Pts',(-0.120765291084357,0.0980396119909781,
1.17195636362376));
#16000=CARTESIAN_POINT('Ctrl Pts',(-0.120470098444528,0.0984021159428093,
1.17192302192006));
#16001=CARTESIAN_POINT('Ctrl Pts',(-0.119776209733078,0.0992464265177424,
1.17184492296877));
#16002=CARTESIAN_POINT('Ctrl Pts',(-0.119376235764783,0.099727167351963,
1.17180011426692));
#16003=CARTESIAN_POINT('Ctrl Pts',(-0.118073702044355,0.10127365805355,
1.17165485379448));
#16004=CARTESIAN_POINT('Ctrl Pts',(-0.117159708419134,0.102329640948196,
1.17155393568649));
#16005=CARTESIAN_POINT('Ctrl Pts',(-0.112450723012935,0.107624373374184,
1.17103889718331));
#16006=CARTESIAN_POINT('Ctrl Pts',(-0.108439905333702,0.111664420554101,
1.17061577500794));
#16007=CARTESIAN_POINT('Ctrl Pts',(-0.0970908770588136,0.121906999106413,
1.1694574942426));
#16008=CARTESIAN_POINT('Ctrl Pts',(-0.0893848155286102,0.127664710528775,
1.16870907607776));
#16009=CARTESIAN_POINT('Ctrl Pts',(-0.0755642935341161,0.13612300119827,
1.16745655961448));
#16010=CARTESIAN_POINT('Ctrl Pts',(-0.0697158911162234,0.139208985486056,
1.16695080130333));
#16011=CARTESIAN_POINT('Ctrl Pts',(-0.063688625668895,0.14191392271517,
1.16646420862114));
#16012=CARTESIAN_POINT('',(-0.155549962195241,-0.000108448416659708,1.16559437743963));
#16013=CARTESIAN_POINT('Ctrl Pts',(-0.063688650312489,0.14191391165553,
1.15273999320994));
#16014=CARTESIAN_POINT('Ctrl Pts',(-0.0739614464780745,0.137303648186015,
1.153606477709));
#16015=CARTESIAN_POINT('Ctrl Pts',(-0.0837099676320785,0.131588667287672,
1.15449238101734));
#16016=CARTESIAN_POINT('Ctrl Pts',(-0.0946672385213198,0.123448594247607,
1.15551736220776));
#16017=CARTESIAN_POINT('Ctrl Pts',(-0.0965409102401436,0.121988916665539,
1.1556936561989));
#16018=CARTESIAN_POINT('Ctrl Pts',(-0.0987661346232789,0.120171964062281,
1.15590358349414));
#16019=CARTESIAN_POINT('Ctrl Pts',(-0.09915020928153,0.11985527236038,1.15593983744304));
#16020=CARTESIAN_POINT('Ctrl Pts',(-0.0997790856266643,0.11933163583965,
1.15599922346576));
#16021=CARTESIAN_POINT('Ctrl Pts',(-0.100024775746547,0.119125771697638,
1.15602243067));
#16022=CARTESIAN_POINT('Ctrl Pts',(-0.100466609141012,0.118753228160401,
1.1560641735315));
#16023=CARTESIAN_POINT('Ctrl Pts',(-0.100662975252751,0.118586821220957,
1.15608272836353));
#16024=CARTESIAN_POINT('Ctrl Pts',(-0.101086236400222,0.1182263272587,1.15612272882583));
#16025=CARTESIAN_POINT('Ctrl Pts',(-0.101312985219345,0.118032074779148,
1.15614416196145));
#16026=CARTESIAN_POINT('Ctrl Pts',(-0.101936280623036,0.117494987012195,
1.15620309422219));
#16027=CARTESIAN_POINT('Ctrl Pts',(-0.102331660733526,0.117150793906415,
1.15624049523621));
#16028=CARTESIAN_POINT('Ctrl Pts',(-0.103221703022011,0.116368034834469,
1.15632475031685));
#16029=CARTESIAN_POINT('Ctrl Pts',(-0.10371532835213,0.115928297712132,
1.15637152234746));
#16030=CARTESIAN_POINT('Ctrl Pts',(-0.105251243783014,0.114542392614199,
1.15651724711886));
#16031=CARTESIAN_POINT('Ctrl Pts',(-0.10628353675908,0.113585184664541,
1.15661547129891));
#16032=CARTESIAN_POINT('Ctrl Pts',(-0.110319236855961,0.109739823934036,
1.15700129835694));
#16033=CARTESIAN_POINT('Ctrl Pts',(-0.113219299269509,0.106745300377919,
1.15728266262057));
#16034=CARTESIAN_POINT('Ctrl Pts',(-0.123121353296417,0.0956624886927571,
1.15827429258106));
#16035=CARTESIAN_POINT('Ctrl Pts',(-0.129405384377851,0.0869737594051406,
1.15896519757145));
#16036=CARTESIAN_POINT('Ctrl Pts',(-0.135856822194371,0.075786866241766,
1.15983094069939));
#16037=CARTESIAN_POINT('Ctrl Pts',(-0.136923953371235,0.0738414219364007,
1.15998060764377));
#16038=CARTESIAN_POINT('Ctrl Pts',(-0.139829350213905,0.0682650315463581,
1.16040818602853));
#16039=CARTESIAN_POINT('Ctrl Pts',(-0.141567128377214,0.064584091911264,
1.1606887999465));
#16040=CARTESIAN_POINT('Ctrl Pts',(-0.143499512851601,0.0600370926553177,
1.16103563514014));
#16041=CARTESIAN_POINT('Ctrl Pts',(-0.143833769983821,0.0592318262448007,
1.16109706374737));
#16042=CARTESIAN_POINT('Ctrl Pts',(-0.14437506188982,0.0578961839209958,
1.16119898018359));
#16043=CARTESIAN_POINT('Ctrl Pts',(-0.144585989219853,0.0573673976574312,
1.16123933670269));
#16044=CARTESIAN_POINT('Ctrl Pts',(-0.144962239669032,0.056408896015496,
1.16131250785242));
#16045=CARTESIAN_POINT('Ctrl Pts',(-0.145128567555238,0.0559795797640432,
1.16134528836012));
#16046=CARTESIAN_POINT('Ctrl Pts',(-0.145481129207378,0.0550574346118643,
1.16141571697613));
#16047=CARTESIAN_POINT('Ctrl Pts',(-0.145666769589473,0.0545643866111579,
1.16145338442744));
#16048=CARTESIAN_POINT('Ctrl Pts',(-0.146165695174164,0.0532185812879525,
1.16155623585675));
#16049=CARTESIAN_POINT('Ctrl Pts',(-0.146474015771233,0.0523640189332964,
1.16162158375167));
#16050=CARTESIAN_POINT('Ctrl Pts',(-0.148055989901746,0.0478559950834417,
1.16196656378922));
#16051=CARTESIAN_POINT('Ctrl Pts',(-0.149200378438692,0.04415896912224,
1.16225040556449));
#16052=CARTESIAN_POINT('Ctrl Pts',(-0.153762637149028,0.027206489070008,
1.16355757203731));
#16053=CARTESIAN_POINT('Ctrl Pts',(-0.1555589075521,0.013579755087206,1.16463088765355));
#16054=CARTESIAN_POINT('Ctrl Pts',(-0.155549966785486,-0.000101651532510474,
1.16568277993484));
#16055=CARTESIAN_POINT('Ctrl Pts',(-0.155549962195241,-0.000108448416659708,
1.16559437743963));
#16056=CARTESIAN_POINT('Ctrl Pts',(-0.155545273848805,-0.00683304738623575,
1.16607786915525));
#16057=CARTESIAN_POINT('Ctrl Pts',(-0.15510450926904,-0.0135425737898805,
1.16656136087087));
#16058=CARTESIAN_POINT('Ctrl Pts',(-0.154233530772585,-0.0201945657398758,
1.1670448525865));
#16059=CARTESIAN_POINT('Ctrl Pts',(-0.152905315892433,-0.0303386447574308,
1.16778216228327));
#16060=CARTESIAN_POINT('Ctrl Pts',(-0.150567052089225,-0.0403891467591377,
1.16851947198005));
#16061=CARTESIAN_POINT('Ctrl Pts',(-0.147250196665396,-0.0501316475093558,
1.16925678167683));
#16062=CARTESIAN_POINT('Ctrl Pts',(-0.143912697417014,-0.0599347847512155,
1.16999868032612));
#16063=CARTESIAN_POINT('Ctrl Pts',(-0.139584514653525,-0.0694251282585468,
1.1707405789754));
#16064=CARTESIAN_POINT('Ctrl Pts',(-0.134349708248288,-0.0783961631306013,
1.17148247762469));
#16065=CARTESIAN_POINT('Ctrl Pts',(-0.12915924963263,-0.0872911979491647,
1.17221809111983));
#16066=CARTESIAN_POINT('Ctrl Pts',(-0.123077963757599,-0.0956748891994967,
1.17295370461497));
#16067=CARTESIAN_POINT('Ctrl Pts',(-0.1162338432083,-0.103370673757252,
1.17368931811011));
#16068=CARTESIAN_POINT('Ctrl Pts',(-0.109302007399008,-0.111165088626745,
1.17443435933647));
#16069=CARTESIAN_POINT('Ctrl Pts',(-0.10158825165106,-0.118253078296368,
1.17517940056283));
#16070=CARTESIAN_POINT('Ctrl Pts',(-0.0932649572480594,-0.124488755514374,
1.17592444178919));
#16071=CARTESIAN_POINT('Ctrl Pts',(-0.0849416628450579,-0.130724432732381,
1.17666948301555));
#16072=CARTESIAN_POINT('Ctrl Pts',(-0.0760096876809342,-0.136107321535937,
1.17741452424191));
#16073=CARTESIAN_POINT('Ctrl Pts',(-0.0666694354545085,-0.140538211445063,
1.17815956546827));
#16074=CARTESIAN_POINT('Ctrl Pts',(-0.0574261099938138,-0.144923120601443,
1.17889687516504));
#16075=CARTESIAN_POINT('Ctrl Pts',(-0.0477136841253745,-0.148408640914046,
1.17963418486182));
#16076=CARTESIAN_POINT('Ctrl Pts',(-0.0377293758646995,-0.1509049260192,
1.1803714945586));
#16077=CARTESIAN_POINT('Ctrl Pts',(-0.0276829261230913,-0.15341674778941,
1.18111339320789));
#16078=CARTESIAN_POINT('Ctrl Pts',(-0.0173620635116654,-0.154926575884814,
1.18185529185717));
#16079=CARTESIAN_POINT('Ctrl Pts',(-0.00698588565388585,-0.155393049721121,
1.18259719050646));
#16080=CARTESIAN_POINT('Ctrl Pts',(0.00330238817903047,-0.155855571723885,
1.1833328040016));
#16081=CARTESIAN_POINT('Ctrl Pts',(0.013644103539955,-0.155292330862292,
1.18406841749674));
#16082=CARTESIAN_POINT('Ctrl Pts',(0.0238215047300092,-0.153715120962117,
1.18480403099188));
#16083=CARTESIAN_POINT('Ctrl Pts',(0.0341293409971891,-0.152117697306865,
1.18554907221824));
#16084=CARTESIAN_POINT('Ctrl Pts',(0.0442676532751995,-0.149480227032185,
1.1862941134446));
#16085=CARTESIAN_POINT('Ctrl Pts',(0.0540203889062351,-0.145868434153586,
1.18703915467097));
#16086=CARTESIAN_POINT('Ctrl Pts',(0.06377312453727,-0.142256641274988,
1.18778419589733));
#16087=CARTESIAN_POINT('Ctrl Pts',(0.0731394184026082,-0.137670988493469,
1.18852923712369));
#16088=CARTESIAN_POINT('Ctrl Pts',(0.081927239882205,-0.132226055924253,
1.18927427835005));
#16089=CARTESIAN_POINT('Ctrl Pts',(0.0906238673454805,-0.126837627150743,
1.19001158804683));
#16090=CARTESIAN_POINT('Ctrl Pts',(0.0988192084139562,-0.120567343834098,
1.19074889774361));
#16091=CARTESIAN_POINT('Ctrl Pts',(0.106330827725443,-0.113532187397328,
1.19148620744039));
#16092=CARTESIAN_POINT('Ctrl Pts',(0.113889198713248,-0.106453244748434,
1.19222810608967));
#16093=CARTESIAN_POINT('Ctrl Pts',(0.120754500477318,-0.0986003842753631,
1.19297000473896));
#16094=CARTESIAN_POINT('Ctrl Pts',(0.12677317071246,-0.0901352632852945,
1.19371190338825));
#16095=CARTESIAN_POINT('Ctrl Pts',(0.132740852486812,-0.0817418563903375,
1.19444751688339));
#16096=CARTESIAN_POINT('Ctrl Pts',(0.137875666974655,-0.0727473026465363,
1.19518313037852));
#16097=CARTESIAN_POINT('Ctrl Pts',(0.142069439965937,-0.0633409561639615,
1.19591874387366));
#16098=CARTESIAN_POINT('Ctrl Pts',(0.146316960971395,-0.0538140565553291,
1.19666378510002));
#16099=CARTESIAN_POINT('Ctrl Pts',(0.149598704911011,-0.0438656002926485,
1.19740882632638));
#16100=CARTESIAN_POINT('Ctrl Pts',(0.151852733305272,-0.0337127555639993,
1.19815386755274));
#16101=CARTESIAN_POINT('Ctrl Pts',(0.154106761699532,-0.0235599108353509,
1.1988989087791));
#16102=CARTESIAN_POINT('Ctrl Pts',(0.155332994178447,-0.0132036554256187,
1.19964395000546));
#16103=CARTESIAN_POINT('Ctrl Pts',(0.15552356776244,-0.0028674676008397,
1.20038899123183));
#16104=CARTESIAN_POINT('Ctrl Pts',(0.155712163703785,0.00736145831798887,
1.2011263009286));
#16105=CARTESIAN_POINT('Ctrl Pts',(0.154887989418757,0.0176474101381822,
1.20186361062538));
#16106=CARTESIAN_POINT('Ctrl Pts',(0.153050402774849,0.0277736693732832,
1.20260092032215));
#16107=CARTESIAN_POINT('Ctrl Pts',(0.151201379148786,0.037962953580048,
1.20334281897144));
#16108=CARTESIAN_POINT('Ctrl Pts',(0.148326274897554,0.0479895961619971,
1.20408471762073));
#16109=CARTESIAN_POINT('Ctrl Pts',(0.144477641750931,0.0576369112122566,
1.20482661627002));
#16110=CARTESIAN_POINT('Ctrl Pts',(0.140661613128677,0.0672024969558601,
1.20556222976516));
#16111=CARTESIAN_POINT('Ctrl Pts',(0.135888857329139,0.0763942932412717,
1.20629784326029));
#16112=CARTESIAN_POINT('Ctrl Pts',(0.130259809785238,0.0850187300229408,
1.20703345675543));
#16113=CARTESIAN_POINT('Ctrl Pts',(0.124558619536452,0.0937536988604648,
1.20777849798179));
#16114=CARTESIAN_POINT('Ctrl Pts',(0.117979520416751,0.101905820061075,
1.20852353920816));
#16115=CARTESIAN_POINT('Ctrl Pts',(0.110671389748095,0.10930528802956,1.20926858043452));
#16116=CARTESIAN_POINT('Ctrl Pts',(0.10336325907944,0.116704755998046,1.21001362166088));
#16117=CARTESIAN_POINT('Ctrl Pts',(0.095326874815334,0.123350972979471,
1.21075866288724));
#16118=CARTESIAN_POINT('Ctrl Pts',(0.0867457397866691,0.129116145887583,
1.2115037041136));
#16119=CARTESIAN_POINT('Ctrl Pts',(0.0782536539233378,0.134821491764217,
1.21224101381038));
#16120=CARTESIAN_POINT('Ctrl Pts',(0.0691644551944208,0.139706830500264,
1.21297832350716));
#16121=CARTESIAN_POINT('Ctrl Pts',(0.0596598825377341,0.143654101631606,
1.21371563320394));
#16122=CARTESIAN_POINT('Ctrl Pts',(0.0500961542335173,0.147625940240959,
1.21445753185322));
#16123=CARTESIAN_POINT('Ctrl Pts',(0.040112660108692,0.15064746816253,1.21519943050251));
#16124=CARTESIAN_POINT('Ctrl Pts',(0.0299199574112516,0.152645336150532,
1.2159413291518));
#16125=CARTESIAN_POINT('Ctrl Pts',(0.0198136043893243,0.154626278769709,
1.21667694264694));
#16126=CARTESIAN_POINT('Ctrl Pts',(0.00950250084430574,0.155600681437315,
1.21741255614208));
#16127=CARTESIAN_POINT('Ctrl Pts',(-0.000796251833269475,0.155547962002136,
1.21814816963721));
#16128=CARTESIAN_POINT('Ctrl Pts',(-0.0112269948465221,0.155494566906889,
1.21889321086358));
#16129=CARTESIAN_POINT('Ctrl Pts',(-0.0216440962629482,0.154387488149287,
1.21963825208994));
#16130=CARTESIAN_POINT('Ctrl Pts',(-0.0318241528047296,0.152259731374586,
1.2203832933163));
#16131=CARTESIAN_POINT('Ctrl Pts',(-0.0420042093465111,0.150131974599885,
1.22112833454266));
#16132=CARTESIAN_POINT('Ctrl Pts',(-0.0519462969147143,0.146983869298261,
1.22187337576902));
#16133=CARTESIAN_POINT('Ctrl Pts',(-0.0614435346592933,0.142900295830947,
1.22261841699538));
#16134=CARTESIAN_POINT('Ctrl Pts',(-0.0621942538492122,0.142577505452544,
1.22267730956614));
#16135=CARTESIAN_POINT('Ctrl Pts',(-0.0629426524443354,0.142248703184176,
1.2227362021369));
#16136=CARTESIAN_POINT('Ctrl Pts',(-0.0636886258329928,0.141913922641526,
1.22279509470766));
#16137=CARTESIAN_POINT('Origin',(0.,0.,-0.129405622560373));
#16138=CARTESIAN_POINT('',(-0.0636118382027688,0.141739365081128,1.30659839996889));
#16139=CARTESIAN_POINT('',(-0.0636380227784817,0.141804318283712,1.29280313411188));
#16140=CARTESIAN_POINT('',(-0.0636886258329924,0.141913922641526,-0.129405622560373));
#16141=CARTESIAN_POINT('',(-0.155313773579517,1.76826588726336E-5,1.24941564258899));
#16142=CARTESIAN_POINT('Ctrl Pts',(-0.155296357294745,1.6960594703571E-5,
1.24940562256037));
#16143=CARTESIAN_POINT('Ctrl Pts',(-0.155270088652903,-0.0269814387089377,
1.2513319394326));
#16144=CARTESIAN_POINT('Ctrl Pts',(-0.135721405315835,-0.105941739255518,
1.25696316059875));
#16145=CARTESIAN_POINT('Ctrl Pts',(-0.0100014200241654,-0.183584930129994,
1.26629928605883));
#16146=CARTESIAN_POINT('Ctrl Pts',(0.148824776878697,-0.107956661491269,
1.2774139989406));
#16147=CARTESIAN_POINT('Ctrl Pts',(0.171409230594902,0.0665006063145147,
1.28852871182238));
#16148=CARTESIAN_POINT('Ctrl Pts',(0.0538351618240076,0.165910646501256,
1.29825684549848));
#16149=CARTESIAN_POINT('Ctrl Pts',(-0.0339132747862035,0.154841375238312,
1.30428007488065));
#16150=CARTESIAN_POINT('Ctrl Pts',(-0.0636118382027626,0.141739365081131,
1.30659839996889));
#16151=CARTESIAN_POINT('Ctrl Pts',(-0.155549997573297,2.74763022365475E-5,
1.24955154822045));
#16152=CARTESIAN_POINT('Ctrl Pts',(-0.155549897792255,0.00059236093511806,
1.2495109550988));
#16153=CARTESIAN_POINT('Ctrl Pts',(-0.155546720919687,0.00115723502798456,
1.24947026588767));
#16154=CARTESIAN_POINT('Ctrl Pts',(-0.155528391633386,0.00281276570515671,
1.24935072391838));
#16155=CARTESIAN_POINT('Ctrl Pts',(-0.15550484427919,0.00390327401653914,
1.24927161143684));
#16156=CARTESIAN_POINT('Ctrl Pts',(-0.155311207207001,0.009932153623866,
1.24883212517115));
#16157=CARTESIAN_POINT('Ctrl Pts',(-0.154917365575576,0.0148599720765029,
1.24846492479375));
#16158=CARTESIAN_POINT('Ctrl Pts',(-0.152420345190767,0.0343569442760507,
1.2469797991768));
#16159=CARTESIAN_POINT('Ctrl Pts',(-0.148489503867105,0.0486122476048482,
1.24581281742909));
#16160=CARTESIAN_POINT('Ctrl Pts',(-0.141578533564202,0.0644830634541898,
1.24451056172612));
#16161=CARTESIAN_POINT('Ctrl Pts',(-0.140482173517817,0.0668379212591646,
1.24431753404194));
#16162=CARTESIAN_POINT('Ctrl Pts',(-0.139087357506472,0.0696476891977804,
1.24408837602936));
#16163=CARTESIAN_POINT('Ctrl Pts',(-0.138844925967983,0.0701297382347594,
1.24404910336281));
#16164=CARTESIAN_POINT('Ctrl Pts',(-0.138463488660094,0.0708784538858501,
1.24398818212399));
#16165=CARTESIAN_POINT('Ctrl Pts',(-0.138326212901935,0.0711459889633148,
1.24396642878445));
#16166=CARTESIAN_POINT('Ctrl Pts',(-0.13806980264326,0.0716421563112034,
1.24392611618626));
#16167=CARTESIAN_POINT('Ctrl Pts',(-0.137950876737586,0.0718708882097017,
1.24390754469048));
#16168=CARTESIAN_POINT('Ctrl Pts',(-0.137680326337336,0.0723880960045699,
1.2438655782523));
#16169=CARTESIAN_POINT('Ctrl Pts',(-0.137528363896171,0.0726763911654976,
1.24384220493201));
#16170=CARTESIAN_POINT('Ctrl Pts',(-0.137066046733504,0.073546832286427,
1.24377168570132));
#16171=CARTESIAN_POINT('Ctrl Pts',(-0.136752888145346,0.0741274937650393,
1.24372471253454));
#16172=CARTESIAN_POINT('Ctrl Pts',(-0.134318256015227,0.078573868258185,
1.24336541512064));
#16173=CARTESIAN_POINT('Ctrl Pts',(-0.132036714779972,0.0823502380113913,
1.2430625557419));
#16174=CARTESIAN_POINT('Ctrl Pts',(-0.123133412475427,0.0957631579702634,
1.24197601185141));
#16175=CARTESIAN_POINT('Ctrl Pts',(-0.115592095511441,0.10474216075819,
1.24122458869673));
#16176=CARTESIAN_POINT('Ctrl Pts',(-0.103849755793823,0.115893556086649,
1.24014268286757));
#16177=CARTESIAN_POINT('Ctrl Pts',(-0.100450942899601,0.118851549300029,
1.23983829631164));
#16178=CARTESIAN_POINT('Ctrl Pts',(-0.094807264280304,0.123348057235167,
1.23934153179967));
#16179=CARTESIAN_POINT('Ctrl Pts',(-0.0926419890821297,0.124982482307883,
1.23915285454269));
#16180=CARTESIAN_POINT('Ctrl Pts',(-0.0899495996815603,0.126906375847685,
1.23891996101002));
#16181=CARTESIAN_POINT('Ctrl Pts',(-0.0894620117077727,0.127250568395987,
1.23887785168188));
#16182=CARTESIAN_POINT('Ctrl Pts',(-0.0885186639883457,0.127908383982087,
1.23879650332115));
#16183=CARTESIAN_POINT('Ctrl Pts',(-0.0880631874172144,0.128222398880844,
1.23875727987107));
#16184=CARTESIAN_POINT('Ctrl Pts',(-0.0876020550427119,0.128536697000022,
1.23871762066113));
#16185=CARTESIAN_POINT('Ctrl Pts',(-0.0875980592786067,0.128539420155855,
1.23871727701347));
#16186=CARTESIAN_POINT('Ctrl Pts',(-0.0875899532725982,0.128544943931847,
1.23871657988056));
#16187=CARTESIAN_POINT('Ctrl Pts',(-0.0875858430233142,0.128547744541213,
1.23871622639491));
#16188=CARTESIAN_POINT('Ctrl Pts',(-0.0875774993152979,0.128553429125475,
1.23871550883577));
#16189=CARTESIAN_POINT('Ctrl Pts',(-0.0875732658480037,0.128556313088679,
1.2387151447618));
#16190=CARTESIAN_POINT('Ctrl Pts',(-0.0875646661091541,0.128562170863362,
1.23871440520163));
#16191=CARTESIAN_POINT('Ctrl Pts',(-0.0875602998290239,0.128565144661216,
1.23871402971497));
#16192=CARTESIAN_POINT('Ctrl Pts',(-0.0875514238927936,0.128571189245924,
1.23871326642114));
#16193=CARTESIAN_POINT('Ctrl Pts',(-0.087546914226689,0.128574260017904,
1.23871287861341));
#16194=CARTESIAN_POINT('Ctrl Pts',(-0.087537739829984,0.128580506443638,
1.23871208967321));
#16195=CARTESIAN_POINT('Ctrl Pts',(-0.0875330750879808,0.128583682080917,
1.23871168854011));
#16196=CARTESIAN_POINT('Ctrl Pts',(-0.0875235775708511,0.128590146991806,
1.238710871835));
#16197=CARTESIAN_POINT('Ctrl Pts',(-0.0875187447831786,0.128593436246769,
1.23871045626231));
#16198=CARTESIAN_POINT('Ctrl Pts',(-0.0875088967333875,0.128600138138745,
1.23870960943737));
#16199=CARTESIAN_POINT('Ctrl Pts',(-0.0875038814573037,0.128603550754655,
1.23870917818436));
#16200=CARTESIAN_POINT('Ctrl Pts',(-0.0874936522875372,0.128610510259281,
1.23870829861201));
#16201=CARTESIAN_POINT('Ctrl Pts',(-0.0874884383775677,0.128614057124482,
1.23870785029175));
#16202=CARTESIAN_POINT('Ctrl Pts',(-0.0874777938169087,0.128621297350242,
1.23870693502806));
#16203=CARTESIAN_POINT('Ctrl Pts',(-0.0874723631478317,0.12862499068403,
1.23870646808361));
#16204=CARTESIAN_POINT('Ctrl Pts',(-0.0874612646317786,0.128632537625535,
1.23870551381596));
#16205=CARTESIAN_POINT('Ctrl Pts',(-0.0874555967642515,0.128636391202425,
1.23870502649164));
#16206=CARTESIAN_POINT('Ctrl Pts',(-0.0874440006928635,0.128644274237941,
1.23870402947504));
#16207=CARTESIAN_POINT('Ctrl Pts',(-0.0874380724658325,0.12864830366095,
1.23870351978149));
#16208=CARTESIAN_POINT('Ctrl Pts',(-0.0874259292990253,0.128656556158875,
1.23870247576086));
#16209=CARTESIAN_POINT('Ctrl Pts',(-0.0874197143313886,0.128660779193499,
1.23870194143222));
#16210=CARTESIAN_POINT('Ctrl Pts',(-0.0874069674644387,0.128669439265987,
1.23870084554592));
#16211=CARTESIAN_POINT('Ctrl Pts',(-0.0874004355336225,0.128673876256551,
1.23870028398651));
#16212=CARTESIAN_POINT('Ctrl Pts',(-0.0873870199099423,0.128682987688719,
1.23869913064722));
#16213=CARTESIAN_POINT('Ctrl Pts',(-0.0873801361795286,0.128687662075595,
1.23869853886523));
#16214=CARTESIAN_POINT('Ctrl Pts',(-0.0873659765319695,0.128697275503207,
1.23869732160901));
#16215=CARTESIAN_POINT('Ctrl Pts',(-0.0873587005713848,0.128702214479053,
1.23869669613236));
#16216=CARTESIAN_POINT('Ctrl Pts',(-0.0873437091146058,0.128712388933786,
1.23869540742055));
#16217=CARTESIAN_POINT('Ctrl Pts',(-0.0873359935669576,0.1287176243356,
1.23869474418252));
#16218=CARTESIAN_POINT('Ctrl Pts',(-0.0873200676345597,0.128728428820993,
1.23869337519903));
#16219=CARTESIAN_POINT('Ctrl Pts',(-0.0873118569454363,0.128733997977103,
1.23869266942927));
#16220=CARTESIAN_POINT('Ctrl Pts',(-0.0872948739885516,0.128745514825353,
1.23869120965114));
#16221=CARTESIAN_POINT('Ctrl Pts',(-0.0872861017185357,0.128751462357163,
1.23869045564486));
#16222=CARTESIAN_POINT('Ctrl Pts',(-0.0872699482499101,0.128762411875348,
1.23868906723332));
#16223=CARTESIAN_POINT('Ctrl Pts',(-0.0872625673151107,0.128767414065362,
1.2386884328454));
#16224=CARTESIAN_POINT('Ctrl Pts',(-0.0872447148154183,0.128779510780091,
1.23868689846265));
#16225=CARTESIAN_POINT('Ctrl Pts',(-0.087234242954536,0.128786604567902,
1.23868599845552));
#16226=CARTESIAN_POINT('Ctrl Pts',(-0.0868547250213077,0.129043627898895,
1.23865338161986));
#16227=CARTESIAN_POINT('Ctrl Pts',(-0.0864846108112903,0.129291968989012,
1.23862160529118));
#16228=CARTESIAN_POINT('Ctrl Pts',(-0.0856340603875407,0.129857389310533,
1.23854865160341));
#16229=CARTESIAN_POINT('Ctrl Pts',(-0.0851529236762294,0.130173397550784,
1.23850743470721));
#16230=CARTESIAN_POINT('Ctrl Pts',(-0.0837195808040299,0.131103463145408,
1.2383847902612));
#16231=CARTESIAN_POINT('Ctrl Pts',(-0.0827624256149272,0.131709783382766,
1.23830307772827));
#16232=CARTESIAN_POINT('Ctrl Pts',(-0.0759773452888538,0.135904701928224,
1.23772502082442));
#16233=CARTESIAN_POINT('Ctrl Pts',(-0.0699273504175132,0.139114086459763,
1.23721519076703));
#16234=CARTESIAN_POINT('Ctrl Pts',(-0.063688617770428,0.141913926259872,
1.23669476364274));
#16235=CARTESIAN_POINT('',(-0.155549948070468,0.000127103401447693,1.23559437743963));
#16236=CARTESIAN_POINT('Ctrl Pts',(-0.0636886258329928,0.141913922641526,
1.22279509470766));
#16237=CARTESIAN_POINT('Ctrl Pts',(-0.0730258425131839,0.137723533929853,
1.22353224257703));
#16238=CARTESIAN_POINT('Ctrl Pts',(-0.0819815705725974,0.132592492564984,
1.22426939044639));
#16239=CARTESIAN_POINT('Ctrl Pts',(-0.0903597265864884,0.126613278573833,
1.22500653831575));
#16240=CARTESIAN_POINT('Ctrl Pts',(-0.0987278568671842,0.120641219618241,
1.225742804076));
#16241=CARTESIAN_POINT('Ctrl Pts',(-0.106518983643229,0.113823461665015,
1.22647906983624));
#16242=CARTESIAN_POINT('Ctrl Pts',(-0.113563657596095,0.106297216207184,
1.22721533559648));
#16243=CARTESIAN_POINT('Ctrl Pts',(-0.120601882914084,0.0987778602107073,
1.22795092738528));
#16244=CARTESIAN_POINT('Ctrl Pts',(-0.126894366670152,0.0905519706795469,
1.22868651917408));
#16245=CARTESIAN_POINT('Ctrl Pts',(-0.132309082683801,0.0817930873568847,
1.22942211096287));
#16246=CARTESIAN_POINT('Ctrl Pts',(-0.137737399775053,0.0730122028338862,
1.23015955046464));
#16247=CARTESIAN_POINT('Ctrl Pts',(-0.14228306495749,0.0636964517140005,
1.23089698996641));
#16248=CARTESIAN_POINT('Ctrl Pts',(-0.145858742363638,0.0540465519353256,
1.23163442946818));
#16249=CARTESIAN_POINT('Ctrl Pts',(-0.149250783616596,0.0448922422988105,
1.23233399627117));
#16250=CARTESIAN_POINT('Ctrl Pts',(-0.151770122251847,0.03543807975696,
1.23303356307417));
#16251=CARTESIAN_POINT('Ctrl Pts',(-0.153384283523106,0.0258662727910986,
1.23373312987716));
#16252=CARTESIAN_POINT('Ctrl Pts',(-0.154815814063959,0.0173774468932388,
1.23435354573131));
#16253=CARTESIAN_POINT('Ctrl Pts',(-0.155542888541652,0.00876659949918076,
1.23497396158547));
#16254=CARTESIAN_POINT('Ctrl Pts',(-0.155549948070468,0.000127103401447693,
1.23559437743963));
#16255=CARTESIAN_POINT('Ctrl Pts',(-0.155651476811241,0.000126240882040021,
1.23559444529176));
#16256=CARTESIAN_POINT('Ctrl Pts',(-0.155271154691676,-0.0428543475497745,
1.23867891111416));
#16257=CARTESIAN_POINT('Ctrl Pts',(-0.114465767332605,-0.138094367465394,
1.24546828123047));
#16258=CARTESIAN_POINT('Ctrl Pts',(0.0468123474454561,-0.177797800804905,
1.25596255564071));
#16259=CARTESIAN_POINT('Ctrl Pts',(0.174771089844121,-0.0570834476806803,
1.26707726852248));
#16260=CARTESIAN_POINT('Ctrl Pts',(0.142735519209796,0.115887986436578,
1.27819198140426));
#16261=CARTESIAN_POINT('Ctrl Pts',(0.0172060236451339,0.167488946801519,
1.28676726993406));
#16262=CARTESIAN_POINT('Ctrl Pts',(-0.0488244285946477,0.148605630511624,
1.29163765416994));
#16263=CARTESIAN_POINT('Ctrl Pts',(-0.0636380227784998,0.141804318283704,
1.29280313411188));
#16264=CARTESIAN_POINT('Origin',(0.,0.,-0.129405622560373));
#16265=CARTESIAN_POINT('',(-0.0636886258329916,0.141913922641527,1.37660119646451));
#16266=CARTESIAN_POINT('',(-0.0636886474661844,0.141913912932905,1.36266955208845));
#16267=CARTESIAN_POINT('',(-0.0636886258329924,0.141913922641526,-0.129405622560373));
#16268=CARTESIAN_POINT('',(-0.155549935849213,-0.000141270329049539,1.31940562256037));
#16269=CARTESIAN_POINT('Ctrl Pts',(-0.155549935849213,-0.000141270329049539,
1.31940562256037));
#16270=CARTESIAN_POINT('Ctrl Pts',(-0.155539514661892,-0.0116158314067744,
1.32022803186282));
#16271=CARTESIAN_POINT('Ctrl Pts',(-0.154257754311619,-0.0230340958254805,
1.32105044116527));
#16272=CARTESIAN_POINT('Ctrl Pts',(-0.151751199017876,-0.0341668859663438,
1.32187285046771));
#16273=CARTESIAN_POINT('Ctrl Pts',(-0.149504011980853,-0.044147699775993,
1.32261016016449));
#16274=CARTESIAN_POINT('Ctrl Pts',(-0.146259507782471,-0.0539432732970475,
1.32334746986127));
#16275=CARTESIAN_POINT('Ctrl Pts',(-0.142068554767014,-0.0633429415674076,
1.32408477955805));
#16276=CARTESIAN_POINT('Ctrl Pts',(-0.137851517618334,-0.0728011125693691,
1.32482667820733));
#16277=CARTESIAN_POINT('Ctrl Pts',(-0.132676426851961,-0.0818575037646038,
1.32556857685662));
#16278=CARTESIAN_POINT('Ctrl Pts',(-0.126645813638856,-0.0903141206442943,
1.32631047550591));
#16279=CARTESIAN_POINT('Ctrl Pts',(-0.12066629006405,-0.0986990954732759,
1.32704608900104));
#16280=CARTESIAN_POINT('Ctrl Pts',(-0.113846248774929,-0.106493667539107,
1.32778170249618));
#16281=CARTESIAN_POINT('Ctrl Pts',(-0.106329241111352,-0.113533673351495,
1.32851731599132));
#16282=CARTESIAN_POINT('Ctrl Pts',(-0.0987158943671244,-0.120663904918345,
1.32926235721768));
#16283=CARTESIAN_POINT('Ctrl Pts',(-0.0903882631286982,-0.127019389420133,
1.33000739844404));
#16284=CARTESIAN_POINT('Ctrl Pts',(-0.0815313070020709,-0.132470557025077,
1.3307524396704));
#16285=CARTESIAN_POINT('Ctrl Pts',(-0.0726743508754436,-0.13792172463002,
1.33149748089676));
#16286=CARTESIAN_POINT('Ctrl Pts',(-0.0632889675620807,-0.14246817954184,
1.33224252212312));
#16287=CARTESIAN_POINT('Ctrl Pts',(-0.0535837684891806,-0.146029388324741,
1.33298756334948));
#16288=CARTESIAN_POINT('Ctrl Pts',(-0.0439792833514192,-0.149553641312332,
1.33372487304626));
#16289=CARTESIAN_POINT('Ctrl Pts',(-0.0339896175168683,-0.15213949602857,
1.33446218274304));
#16290=CARTESIAN_POINT('Ctrl Pts',(-0.0238193565707109,-0.1537154538508,
1.33519949243981));
#16291=CARTESIAN_POINT('Ctrl Pts',(-0.0135857967900037,-0.155301220299767,
1.3359413910891));
#16292=CARTESIAN_POINT('Ctrl Pts',(-0.00317028471788524,-0.155864153863497,
1.33668328973839));
#16293=CARTESIAN_POINT('Ctrl Pts',(0.00720522434977123,-0.155383033958246,
1.33742518838768));
#16294=CARTESIAN_POINT('Ctrl Pts',(0.017492835058364,-0.154905989963865,
1.33816080188282));
#16295=CARTESIAN_POINT('Ctrl Pts',(0.0277401800666532,-0.153402581451298,
1.33889641537795));
#16296=CARTESIAN_POINT('Ctrl Pts',(0.0377314847457342,-0.150904398739342,
1.33963202887309));
#16297=CARTESIAN_POINT('Ctrl Pts',(0.0478508394615628,-0.148374198948702,
1.34037707009945));
#16298=CARTESIAN_POINT('Ctrl Pts',(0.0577065890818968,-0.144823730709507,
1.34112211132582));
#16299=CARTESIAN_POINT('Ctrl Pts',(0.0670895699605935,-0.140338134883226,
1.34186715255218));
#16300=CARTESIAN_POINT('Ctrl Pts',(0.0764725508392916,-0.135852539056945,
1.34261219377854));
#16301=CARTESIAN_POINT('Ctrl Pts',(0.085381943627054,-0.130432355263206,
1.3433572350049));
#16302=CARTESIAN_POINT('Ctrl Pts',(0.0936369593371753,-0.12420918784892,
1.34410227623126));
#16303=CARTESIAN_POINT('Ctrl Pts',(0.101806310125775,-0.118050600220654,
1.34483958592804));
#16304=CARTESIAN_POINT('Ctrl Pts',(0.109396091215815,-0.111059513673848,
1.34557689562482));
#16305=CARTESIAN_POINT('Ctrl Pts',(0.116235287794278,-0.103369049388013,
1.3463142053216));
#16306=CARTESIAN_POINT('Ctrl Pts',(0.123117050947461,-0.0956307203100334,
1.34705610397088));
#16307=CARTESIAN_POINT('Ctrl Pts',(0.129238096716883,-0.0871848583285731,
1.34779800262017));
#16308=CARTESIAN_POINT('Ctrl Pts',(0.134460234808284,-0.0782064431827791,
1.34853990126946));
#16309=CARTESIAN_POINT('Ctrl Pts',(0.139638132432452,-0.0693040906140549,
1.3492755147646));
#16310=CARTESIAN_POINT('Ctrl Pts',(0.14393184220442,-0.059878997868156,
1.35001112825974));
#16311=CARTESIAN_POINT('Ctrl Pts',(0.147250897236983,-0.050129589694145,
1.35074674175487));
#16312=CARTESIAN_POINT('Ctrl Pts',(0.150612489769146,-0.0402552316647622,
1.35149178298124));
#16313=CARTESIAN_POINT('Ctrl Pts',(0.15297390508003,-0.030049089248297,
1.3522368242076));
#16314=CARTESIAN_POINT('Ctrl Pts',(0.154293254485432,-0.0197330717399448,
1.35298186543396));
#16315=CARTESIAN_POINT('Ctrl Pts',(0.155612603890834,-0.00941705423159124,
1.35372690666032));
#16316=CARTESIAN_POINT('Ctrl Pts',(0.155889896467494,0.00100785732826855,
1.35447194788668));
#16317=CARTESIAN_POINT('Ctrl Pts',(0.155137669070008,0.0113183980988834,
1.35521698911304));
#16318=CARTESIAN_POINT('Ctrl Pts',(0.154393247775287,0.0215219431111804,
1.35595429880981));
#16319=CARTESIAN_POINT('Ctrl Pts',(0.152635073861283,0.0316899759881723,
1.35669160850659));
#16320=CARTESIAN_POINT('Ctrl Pts',(0.149882258914002,0.041606621622478,
1.35742891820337));
#16321=CARTESIAN_POINT('Ctrl Pts',(0.14711231068186,0.0515849876113171,
1.35817081685266));
#16322=CARTESIAN_POINT('Ctrl Pts',(0.143335374636995,0.0613078750443079,
1.35891271550194));
#16323=CARTESIAN_POINT('Ctrl Pts',(0.1386235318856,0.0705642891805904,1.35965461415123));
#16324=CARTESIAN_POINT('Ctrl Pts',(0.133951606524602,0.0797422856114763,
1.36039022764637));
#16325=CARTESIAN_POINT('Ctrl Pts',(0.128361001530006,0.0884608550278958,
1.36112584114151));
#16326=CARTESIAN_POINT('Ctrl Pts',(0.121969375729713,0.0965363863219678,
1.36186145463665));
#16327=CARTESIAN_POINT('Ctrl Pts',(0.115495833908948,0.104715414818077,
1.36260649586301));
#16328=CARTESIAN_POINT('Ctrl Pts',(0.108201155658404,0.112234011397048,
1.36335153708937));
#16329=CARTESIAN_POINT('Ctrl Pts',(0.100249074280249,0.118936645345129,
1.36409657831573));
#16330=CARTESIAN_POINT('Ctrl Pts',(0.0922969929020949,0.125639279293211,
1.3648416195421));
#16331=CARTESIAN_POINT('Ctrl Pts',(0.0836883375898021,0.131525426243354,
1.36558666076846));
#16332=CARTESIAN_POINT('Ctrl Pts',(0.0746174941672043,0.136484548811238,
1.36633170199482));
#16333=CARTESIAN_POINT('Ctrl Pts',(0.065640543858759,0.141392339056463,
1.3670690312326));
#16334=CARTESIAN_POINT('Ctrl Pts',(0.0561436708638565,0.145429069350255,
1.36780636047038));
#16335=CARTESIAN_POINT('Ctrl Pts',(0.0463186330379303,0.148493726242887,
1.36854368970816));
#16336=CARTESIAN_POINT('Ctrl Pts',(0.0365092861973104,0.151553488753724,
1.36927984140113));
#16337=CARTESIAN_POINT('Ctrl Pts',(0.0263736652944203,0.153643898568171,
1.37001599309411));
#16338=CARTESIAN_POINT('Ctrl Pts',(0.0161230977477578,0.154712146320243,
1.37075214478708));
#16339=CARTESIAN_POINT('Ctrl Pts',(0.00588296731361892,0.155779306384054,
1.37148754693151));
#16340=CARTESIAN_POINT('Ctrl Pts',(-0.00447095844475691,0.155826254591357,
1.37222294907593));
#16341=CARTESIAN_POINT('Ctrl Pts',(-0.0147207954195999,0.154851866899351,
1.37295835122036));
#16342=CARTESIAN_POINT('Ctrl Pts',(-0.0249885283044939,0.153875777955458,
1.37369503735502));
#16343=CARTESIAN_POINT('Ctrl Pts',(-0.0351508846718456,0.151874897306929,
1.37443172348968));
#16344=CARTESIAN_POINT('Ctrl Pts',(-0.0449955051149119,0.14889998999145,
1.37516840962434));
#16345=CARTESIAN_POINT('Ctrl Pts',(-0.0513777991718371,0.146971349533518,
1.37564600523773));
#16346=CARTESIAN_POINT('Ctrl Pts',(-0.0576267276381069,0.144634402484416,
1.37612360085112));
#16347=CARTESIAN_POINT('Ctrl Pts',(-0.0636886258329916,0.141913922641527,
1.37660119646451));
#16348=CARTESIAN_POINT('Ctrl Pts',(-0.0636118382027626,0.141739365081131,
1.30659839996889));
#16349=CARTESIAN_POINT('Ctrl Pts',(-0.0813744076891851,0.133903115139863,
1.30798497917457));
#16350=CARTESIAN_POINT('Ctrl Pts',(-0.131574028003387,0.100038822065039,
1.31225404952175));
#16351=CARTESIAN_POINT('Ctrl Pts',(-0.155195691316953,0.0400812519945282,
1.31652311986892));
#16352=CARTESIAN_POINT('Ctrl Pts',(-0.15556701015029,-0.00014112466882523,
1.31940561101042));
#16353=CARTESIAN_POINT('',(-0.155315966858501,2.90168067545608E-5,1.30558500287933));
#16354=CARTESIAN_POINT('Ctrl Pts',(-0.0636380227784998,0.141804318283704,
1.29280313411188));
#16355=CARTESIAN_POINT('Ctrl Pts',(-0.0959148560870726,0.126985171874289,
1.29534255846386));
#16356=CARTESIAN_POINT('Ctrl Pts',(-0.142237182102223,0.0839092470420679,
1.29960629650446));
#16357=CARTESIAN_POINT('Ctrl Pts',(-0.155340312234673,0.0241955981471813,
1.30387003454505));
#16358=CARTESIAN_POINT('Ctrl Pts',(-0.155299723662096,2.96937538047808E-5,
1.30559434823368));
#16359=CARTESIAN_POINT('Ctrl Pts',(-0.15554999880721,1.92633547010141E-5,
1.30545035502838));
#16360=CARTESIAN_POINT('Ctrl Pts',(-0.15555005883387,-0.000465446963086064,
1.30548436162153));
#16361=CARTESIAN_POINT('Ctrl Pts',(-0.155547853246853,-0.000950150915595704,
1.30551843661611));
#16362=CARTESIAN_POINT('Ctrl Pts',(-0.155538567071807,-0.00195682091136872,
1.30558935389894));
#16363=CARTESIAN_POINT('Ctrl Pts',(-0.15553112438902,-0.00247877574768627,
1.30562620677271));
#16364=CARTESIAN_POINT('Ctrl Pts',(-0.155512361475722,-0.00345123213072981,
1.30569502622914));
#16365=CARTESIAN_POINT('Ctrl Pts',(-0.155501710515548,-0.00390174242615508,
1.30572697172978));
#16366=CARTESIAN_POINT('Ctrl Pts',(-0.155476661418278,-0.00479666117861854,
1.30579055932844));
#16367=CARTESIAN_POINT('Ctrl Pts',(-0.155462315094703,-0.00524106688709894,
1.30582219951222));
#16368=CARTESIAN_POINT('Ctrl Pts',(-0.155429905388864,-0.00612718932417162,
1.30588541762037));
#16369=CARTESIAN_POINT('Ctrl Pts',(-0.155411863922397,-0.00656890271905855,
1.30591699456666));
#16370=CARTESIAN_POINT('Ctrl Pts',(-0.155358282789037,-0.00775655577892897,
1.30600207252022));
#16371=CARTESIAN_POINT('Ctrl Pts',(-0.15531925424223,-0.00850231817017692,
1.30605568201404));
#16372=CARTESIAN_POINT('Ctrl Pts',(-0.15515504957497,-0.0112594031225942,
1.30625458678395));
#16373=CARTESIAN_POINT('Ctrl Pts',(-0.154996165888035,-0.0132684369198708,
1.30640092747855));
#16374=CARTESIAN_POINT('Ctrl Pts',(-0.153260185157275,-0.0308624912253183,
1.30769548410314));
#16375=CARTESIAN_POINT('Ctrl Pts',(-0.149376168893746,-0.0461270517189211,
1.30892174380606));
#16376=CARTESIAN_POINT('Ctrl Pts',(-0.141728961477359,-0.064223146296122,
1.31043358225343));
#16377=CARTESIAN_POINT('Ctrl Pts',(-0.140035518656591,-0.0678363444038684,
1.31073781150859));
#16378=CARTESIAN_POINT('Ctrl Pts',(-0.137259729596023,-0.0732107335590161,
1.31119021751654));
#16379=CARTESIAN_POINT('Ctrl Pts',(-0.136278228544455,-0.0750219329616712,
1.31134265236187));
#16380=CARTESIAN_POINT('Ctrl Pts',(-0.135013027115561,-0.0772498357529264,
1.31152964529558));
#16381=CARTESIAN_POINT('Ctrl Pts',(-0.134762959291308,-0.077685258811472,
1.31156616647412));
#16382=CARTESIAN_POINT('Ctrl Pts',(-0.134363939127277,-0.0783723156188709,
1.31162374493637));
#16383=CARTESIAN_POINT('Ctrl Pts',(-0.134216381170416,-0.0786247481562847,
1.31164488949119));
#16384=CARTESIAN_POINT('Ctrl Pts',(-0.133936798336288,-0.0790999596065081,
1.3116846728616));
#16385=CARTESIAN_POINT('Ctrl Pts',(-0.133804930607092,-0.0793228220937374,
1.31170332089917));
#16386=CARTESIAN_POINT('Ctrl Pts',(-0.13350235111456,-0.0798312937217863,
1.31174584735586));
#16387=CARTESIAN_POINT('Ctrl Pts',(-0.133331279168809,-0.080116684973965,
1.31176970206304));
#16388=CARTESIAN_POINT('Ctrl Pts',(-0.132875110235385,-0.0808721821959808,
1.31183281936455));
#16389=CARTESIAN_POINT('Ctrl Pts',(-0.132588430881952,-0.0813413350858101,
1.31187198163374));
#16390=CARTESIAN_POINT('Ctrl Pts',(-0.13058056559458,-0.0845884008884337,
1.3121428737138));
#16391=CARTESIAN_POINT('Ctrl Pts',(-0.12877454096456,-0.0873132481072574,
1.31236941160099));
#16392=CARTESIAN_POINT('Ctrl Pts',(-0.126441556042374,-0.0906030904096808,
1.31264462278728));
#16393=CARTESIAN_POINT('Ctrl Pts',(-0.125994676248581,-0.0912235094782895,
1.31269660069886));
#16394=CARTESIAN_POINT('Ctrl Pts',(-0.120080788991894,-0.0993076071044975,
1.31337524693761));
#16395=CARTESIAN_POINT('Ctrl Pts',(-0.113962685211251,-0.106272896949726,
1.31397633387423));
#16396=CARTESIAN_POINT('Ctrl Pts',(-0.101008947711542,-0.118606607006691,
1.31515751033723));
#16397=CARTESIAN_POINT('Ctrl Pts',(-0.0942726902580923,-0.124028075670657,
1.31573434681392));
#16398=CARTESIAN_POINT('Ctrl Pts',(-0.0861447681039709,-0.129523254266446,
1.31641646258377));
#16399=CARTESIAN_POINT('Ctrl Pts',(-0.0851599086974459,-0.130172901505695,
1.3164988776663));
#16400=CARTESIAN_POINT('Ctrl Pts',(-0.0835846070952162,-0.131186496412597,
1.31663038691622));
#16401=CARTESIAN_POINT('Ctrl Pts',(-0.0829989426063408,-0.131557815742141,
1.31667921113129));
#16402=CARTESIAN_POINT('Ctrl Pts',(-0.0818829618520441,-0.132254944809996,
1.31677212897925));
#16403=CARTESIAN_POINT('Ctrl Pts',(-0.081353133296262,-0.132581512854851,
1.31681619387815));
#16404=CARTESIAN_POINT('Ctrl Pts',(-0.0804277669819127,-0.133144241364318,
1.31689307703956));
#16405=CARTESIAN_POINT('Ctrl Pts',(-0.0800331105227539,-0.133381842549422,
1.31692584224083));
#16406=CARTESIAN_POINT('Ctrl Pts',(-0.079265107552474,-0.133839579608717,
1.31698955920957));
#16407=CARTESIAN_POINT('Ctrl Pts',(-0.0788918845356574,-0.134059915308606,
1.3170205033396));
#16408=CARTESIAN_POINT('Ctrl Pts',(-0.0779125034064613,-0.13463259593132,
1.31710165502572));
#16409=CARTESIAN_POINT('Ctrl Pts',(-0.0773048812742063,-0.1349824039481,
1.31715195351385));
#16410=CARTESIAN_POINT('Ctrl Pts',(-0.0751970672615263,-0.136176972196828,
1.31732628336913));
#16411=CARTESIAN_POINT('Ctrl Pts',(-0.0736852784998245,-0.137000897701598,
1.31745105324089));
#16412=CARTESIAN_POINT('Ctrl Pts',(-0.0613577688476295,-0.143456328404703,
1.31846674779829));
#16413=CARTESIAN_POINT('Ctrl Pts',(-0.0499299084519012,-0.147822103442598,
1.31940286221832));
#16414=CARTESIAN_POINT('Ctrl Pts',(-0.0290676287696828,-0.153094455870004,
1.32107164474723));
#16415=CARTESIAN_POINT('Ctrl Pts',(-0.0198341904778545,-0.154562244827643,
1.32179569083012));
#16416=CARTESIAN_POINT('Ctrl Pts',(-0.00966275032589286,-0.155251984663078,
1.32254537530335));
#16417=CARTESIAN_POINT('Ctrl Pts',(-0.00880110463397546,-0.155303213535837,
1.32260850064286));
#16418=CARTESIAN_POINT('Ctrl Pts',(-0.00757604145128999,-0.155365820617116,
1.32269766656506));
#16419=CARTESIAN_POINT('Ctrl Pts',(-0.00721296296253917,-0.155383100087144,
1.32272402031452));
#16420=CARTESIAN_POINT('Ctrl Pts',(-0.00658736044452346,-0.155410675960243,
1.32276929993152));
#16421=CARTESIAN_POINT('Ctrl Pts',(-0.00632486624407131,-0.155421580198741,
1.32278825941527));
#16422=CARTESIAN_POINT('Ctrl Pts',(-0.00581615089105437,-0.155441421733273,
1.32282492567624));
#16423=CARTESIAN_POINT('Ctrl Pts',(-0.00556993621752219,-0.155450439093941,
1.32284263699608));
#16424=CARTESIAN_POINT('Ctrl Pts',(-0.00490639121594114,-0.15547316223416,
1.32289027725792));
#16425=CARTESIAN_POINT('Ctrl Pts',(-0.004489021260279,-0.155485772818166,
1.32292014548915));
#16426=CARTESIAN_POINT('Ctrl Pts',(-0.00294478699710083,-0.155526207777226,
1.3230303117388));
#16427=CARTESIAN_POINT('Ctrl Pts',(-0.00181764390367268,-0.155543464803141,
1.32311004557123));
#16428=CARTESIAN_POINT('Ctrl Pts',(0.0100791143516344,-0.155596266098236,
1.32394542711257));
#16429=CARTESIAN_POINT('Ctrl Pts',(0.020826330625677,-0.154525495108031,
1.32464781194362));
#16430=CARTESIAN_POINT('Ctrl Pts',(0.0413458636283426,-0.15029934596446,
1.32602701958209));
#16431=CARTESIAN_POINT('Ctrl Pts',(0.0510867040265423,-0.14727349485332,
1.32670030768066));
#16432=CARTESIAN_POINT('Ctrl Pts',(0.0616369916589631,-0.142822656146584,
1.32749508757108));
#16433=CARTESIAN_POINT('Ctrl Pts',(0.0628061813464088,-0.142312379183446,
1.32758408225122));
#16434=CARTESIAN_POINT('Ctrl Pts',(0.0646363280112985,-0.141486690818027,
1.32772491077386));
#16435=CARTESIAN_POINT('Ctrl Pts',(0.0653015779032153,-0.141180885633662,
1.32777642193344));
#16436=CARTESIAN_POINT('Ctrl Pts',(0.0664247643782563,-0.140654937067164,
1.32786394975641));
#16437=CARTESIAN_POINT('Ctrl Pts',(0.0668838312467152,-0.140437223522803,
1.32789988313271));
#16438=CARTESIAN_POINT('Ctrl Pts',(0.0677835033993699,-0.140005140085795,
1.32797062282043));
#16439=CARTESIAN_POINT('Ctrl Pts',(0.0682241789873927,-0.139790929516246,
1.32800542331237));
#16440=CARTESIAN_POINT('Ctrl Pts',(0.0690699570036463,-0.139374848505379,
1.32807250982114));
#16441=CARTESIAN_POINT('Ctrl Pts',(0.0694752054871472,-0.139173284688337,
1.32810478489198));
#16442=CARTESIAN_POINT('Ctrl Pts',(0.0704149447012462,-0.138700746821056,
1.32817993675351));
#16443=CARTESIAN_POINT('Ctrl Pts',(0.0709487576107526,-0.138428448596697,
1.32822285953901));
#16444=CARTESIAN_POINT('Ctrl Pts',(0.0723618802064355,-0.137697293080737,
1.32833711480769));
#16445=CARTESIAN_POINT('Ctrl Pts',(0.0732383845764503,-0.137233105221232,
1.3284086339555));
#16446=CARTESIAN_POINT('Ctrl Pts',(0.0798282499757151,-0.133662066086512,
1.3289513703526));
#16447=CARTESIAN_POINT('Ctrl Pts',(0.0853453253919051,-0.130208488382998,
1.32943493838304));
#16448=CARTESIAN_POINT('Ctrl Pts',(0.099136254374105,-0.120321907435234,
1.33072326380972));
#16449=CARTESIAN_POINT('Ctrl Pts',(0.107005381870996,-0.113380657644936,
1.33154241044867));
#16450=CARTESIAN_POINT('Ctrl Pts',(0.116844662783263,-0.102758158034655,
1.33265684251503));
#16451=CARTESIAN_POINT('Ctrl Pts',(0.119457532452934,-0.0997086623250283,
1.33296306665312));
#16452=CARTESIAN_POINT('Ctrl Pts',(0.123233696633104,-0.0949396484958213,
1.33341807005433));
#16453=CARTESIAN_POINT('Ctrl Pts',(0.124485327771254,-0.0932924710202543,
1.33357116085352));
#16454=CARTESIAN_POINT('Ctrl Pts',(0.125999964122596,-0.0912143867383204,
1.33375884333785));
#16455=CARTESIAN_POINT('Ctrl Pts',(0.126294152199212,-0.0908066211577997,
1.3337954151008));
#16456=CARTESIAN_POINT('Ctrl Pts',(0.126756375052597,-0.090159355954568,
1.33385305504411));
#16457=CARTESIAN_POINT('Ctrl Pts',(0.126925716731405,-0.0899208013682111,
1.33387421080554));
#16458=CARTESIAN_POINT('Ctrl Pts',(0.127243668331612,-0.0894702096314062,
1.33391400317947));
#16459=CARTESIAN_POINT('Ctrl Pts',(0.127392419967987,-0.0892582818456491,
1.33393264907115));
#16460=CARTESIAN_POINT('Ctrl Pts',(0.127730974153045,-0.0887733703446588,
1.33397515519039));
#16461=CARTESIAN_POINT('Ctrl Pts',(0.127920431011737,-0.0885001490156586,
1.33399899178819));
#16462=CARTESIAN_POINT('Ctrl Pts',(0.128420358944783,-0.0877742287373203,
1.3340620295583));
#16463=CARTESIAN_POINT('Ctrl Pts',(0.128729316011371,-0.0873204846822686,
1.33410113080797));
#16464=CARTESIAN_POINT('Ctrl Pts',(0.130850942601287,-0.084168863182679,
1.33437071590776));
#16465=CARTESIAN_POINT('Ctrl Pts',(0.132581232917176,-0.0814161368992058,
1.33459606433394));
#16466=CARTESIAN_POINT('Ctrl Pts',(0.13696432431337,-0.0739322353633311,
1.33518800319543));
#16467=CARTESIAN_POINT('Ctrl Pts',(0.139458223087769,-0.0691130577450456,
1.33554804777151));
#16468=CARTESIAN_POINT('Ctrl Pts',(0.145033402583886,-0.0568029557448982,
1.33643986197597));
#16469=CARTESIAN_POINT('Ctrl Pts',(0.147791086080892,-0.0491838700494526,
1.33696806779057));
#16470=CARTESIAN_POINT('Ctrl Pts',(0.15103958279508,-0.0374141153602024,
1.33778644477238));
#16471=CARTESIAN_POINT('Ctrl Pts',(0.151977313754222,-0.0334015473762989,
1.33806571094217));
#16472=CARTESIAN_POINT('Ctrl Pts',(0.153234762328562,-0.0268585472664584,
1.33852512939468));
#16473=CARTESIAN_POINT('Ctrl Pts',(0.153653488114263,-0.0243490912198524,
1.33870226212154));
#16474=CARTESIAN_POINT('Ctrl Pts',(0.15412119574545,-0.0210495108636617,
1.33893687882431));
#16475=CARTESIAN_POINT('Ctrl Pts',(0.154225969808342,-0.0202675869584319,
1.33899260196162));
#16476=CARTESIAN_POINT('Ctrl Pts',(0.154387470077688,-0.0189884693381101,
1.33908397517323));
#16477=CARTESIAN_POINT('Ctrl Pts',(0.154447754039681,-0.0184917318341367,
1.33911951299218));
#16478=CARTESIAN_POINT('Ctrl Pts',(0.154559568710073,-0.017531672455502,
1.33918830549427));
#16479=CARTESIAN_POINT('Ctrl Pts',(0.154611415488617,-0.0170683921573794,
1.33922154985337));
#16480=CARTESIAN_POINT('Ctrl Pts',(0.154725999460209,-0.0160011347620351,
1.33929824946366));
#16481=CARTESIAN_POINT('Ctrl Pts',(0.154787283717015,-0.015397012787732,
1.33934174982579));
#16482=CARTESIAN_POINT('Ctrl Pts',(0.154941938873326,-0.0137781185837842,
1.3394585542182));
#16483=CARTESIAN_POINT('Ctrl Pts',(0.155028876030377,-0.0127627770634818,
1.33953205839517));
#16484=CARTESIAN_POINT('Ctrl Pts',(0.155672488145298,-0.00426437425598765,
1.34014945013254));
#16485=CARTESIAN_POINT('Ctrl Pts',(0.155696904999734,0.00324784418413023,
1.34070994580911));
#16486=CARTESIAN_POINT('Ctrl Pts',(0.154988708613029,0.0134885344485974,
1.34149374337532));
#16487=CARTESIAN_POINT('Ctrl Pts',(0.154724604865072,0.0162399507037654,
1.3417062056487));
#16488=CARTESIAN_POINT('Ctrl Pts',(0.15377534342252,0.0239603143191982,
1.34230675811499));
#16489=CARTESIAN_POINT('Ctrl Pts',(0.152922971557529,0.0289053037301482,
1.34269666516858));
#16490=CARTESIAN_POINT('Ctrl Pts',(0.15027405816035,0.0408043732246399,
1.34363994944597));
#16491=CARTESIAN_POINT('Ctrl Pts',(0.148231874503444,0.0476930636696109,
1.34419049859115));
#16492=CARTESIAN_POINT('Ctrl Pts',(0.145426531424755,0.0552053881976066,
1.34477995745877));
#16493=CARTESIAN_POINT('Ctrl Pts',(0.145125677442254,0.0559915061449438,
1.34484149760727));
#16494=CARTESIAN_POINT('Ctrl Pts',(0.14468712359748,0.0571101411239511,
1.3449288252831));
#16495=CARTESIAN_POINT('Ctrl Pts',(0.144554635294281,0.0574446636000431,
1.34495490898803));
#16496=CARTESIAN_POINT('Ctrl Pts',(0.144323634515648,0.0580220622612454,
1.34499987275872));
#16497=CARTESIAN_POINT('Ctrl Pts',(0.1442256672785,0.0582651533197557,1.34501878519815));
#16498=CARTESIAN_POINT('Ctrl Pts',(0.144034023106087,0.0587372445826408,
1.34505547791575));
#16499=CARTESIAN_POINT('Ctrl Pts',(0.143940414324524,0.0589662686602731,
1.34507326227463));
#16500=CARTESIAN_POINT('Ctrl Pts',(0.143685351890981,0.0595860800127816,
1.34512135085048));
#16501=CARTESIAN_POINT('Ctrl Pts',(0.143522849014139,0.0599764378858923,
1.34515159229808));
#16502=CARTESIAN_POINT('Ctrl Pts',(0.14290793553236,0.0614367472350435,
1.34526457374595));
#16503=CARTESIAN_POINT('Ctrl Pts',(0.142445120306893,0.0625023188678151,
1.345346711831));
#16504=CARTESIAN_POINT('Ctrl Pts',(0.138410328545972,0.0715142306325301,
1.3460396312365));
#16505=CARTESIAN_POINT('Ctrl Pts',(0.134187936901027,0.0791539555950223,
1.34661587583481));
#16506=CARTESIAN_POINT('Ctrl Pts',(0.124186779995331,0.094126300335312,
1.34780200127658));
#16507=CARTESIAN_POINT('Ctrl Pts',(0.118344985324206,0.101373392360171,
1.34840976117854));
#16508=CARTESIAN_POINT('Ctrl Pts',(0.108888713581815,0.111165366422583,
1.34933412339123));
#16509=CARTESIAN_POINT('Ctrl Pts',(0.105757617295196,0.114148198103218,
1.34963200466565));
#16510=CARTESIAN_POINT('Ctrl Pts',(0.101800194209621,0.117615496673495,
1.35000153061319));
#16511=CARTESIAN_POINT('Ctrl Pts',(0.101088199322572,0.118228002129573,
1.35006774952524));
#16512=CARTESIAN_POINT('Ctrl Pts',(0.0999630790796138,0.119178311917358,
1.35017200536985));
#16513=CARTESIAN_POINT('Ctrl Pts',(0.0995536788903767,0.119520509608348,
1.3502098623695));
#16514=CARTESIAN_POINT('Ctrl Pts',(0.0988238165589627,0.120124214282875,
1.35027721760755));
#16515=CARTESIAN_POINT('Ctrl Pts',(0.0985040550157329,0.120386563684455,
1.35030668134367));
#16516=CARTESIAN_POINT('Ctrl Pts',(0.097763763223876,0.12098901443662,1.35037479205684));
#16517=CARTESIAN_POINT('Ctrl Pts',(0.0973425000535687,0.121328202342699,
1.35041347523676));
#16518=CARTESIAN_POINT('Ctrl Pts',(0.0961793157355435,0.122254804502689,
1.35052008681497));
#16519=CARTESIAN_POINT('Ctrl Pts',(0.0954338005050662,0.122837647514763,
1.35058819563956));
#16520=CARTESIAN_POINT('Ctrl Pts',(0.0915646607598882,0.125806054160361,
1.35094059411344));
#16521=CARTESIAN_POINT('Ctrl Pts',(0.0883570238875594,0.128079200246822,
1.35122921152411));
#16522=CARTESIAN_POINT('Ctrl Pts',(0.0834054779091896,0.131313622394636,
1.35167006418441));
#16523=CARTESIAN_POINT('Ctrl Pts',(0.0817233868053524,0.132367022431365,
1.35181904253327));
#16524=CARTESIAN_POINT('Ctrl Pts',(0.0674609817423309,0.140923280334954,
1.3530755329944));
#16525=CARTESIAN_POINT('Ctrl Pts',(0.0539009984077992,0.1466456932042,1.35423674111801));
#16526=CARTESIAN_POINT('Ctrl Pts',(0.0371554732459155,0.15107094770266,
1.35554078946067));
#16527=CARTESIAN_POINT('Ctrl Pts',(0.0345514152839025,0.151687713662543,
1.35573977052441));
#16528=CARTESIAN_POINT('Ctrl Pts',(0.031399987164342,0.152348742674966,
1.35597502356239));
#16529=CARTESIAN_POINT('Ctrl Pts',(0.030866843031779,0.152457655149237,
1.35601463260471));
#16530=CARTESIAN_POINT('Ctrl Pts',(0.0300372862465848,0.152622589798859,
1.35607595678393));
#16531=CARTESIAN_POINT('Ctrl Pts',(0.0297412708606671,0.152680549821474,
1.35609777893962));
#16532=CARTESIAN_POINT('Ctrl Pts',(0.0291921220957172,0.152786415875712,
1.35613814757794));
#16533=CARTESIAN_POINT('Ctrl Pts',(0.0289390406972177,0.152834553665209,
1.35615670666161));
#16534=CARTESIAN_POINT('Ctrl Pts',(0.0283670050348196,0.152941886860572,
1.35619855417727));
#16535=CARTESIAN_POINT('Ctrl Pts',(0.0280479851518578,0.153000713283449,
1.35622182146033));
#16536=CARTESIAN_POINT('Ctrl Pts',(0.0271071200016452,0.153171164681162,
1.35629024007954));
#16537=CARTESIAN_POINT('Ctrl Pts',(0.0264847657914144,0.1532800015073,1.35633523703655));
#16538=CARTESIAN_POINT('Ctrl Pts',(0.0220274985685555,0.154031526773631,
1.35665575873807));
#16539=CARTESIAN_POINT('Ctrl Pts',(0.0181699346864958,0.154534079975703,
1.35692394025054));
#16540=CARTESIAN_POINT('Ctrl Pts',(0.0130954031246185,0.155002482321503,
1.35726951667139));
#16541=CARTESIAN_POINT('Ctrl Pts',(0.0118923341248151,0.155099424973858,
1.35735091721061));
#16542=CARTESIAN_POINT('Ctrl Pts',(-0.00414495506203996,0.156203998204142,
1.35843039170935));
#16543=CARTESIAN_POINT('Ctrl Pts',(-0.0190475710698942,0.155093808718543,
1.35937759843878));
#16544=CARTESIAN_POINT('Ctrl Pts',(-0.036777252879314,0.151175554073212,
1.3606211109334));
#16545=CARTESIAN_POINT('Ctrl Pts',(-0.0399644119627392,0.150364415807139,
1.36084903042339));
#16546=CARTESIAN_POINT('Ctrl Pts',(-0.0439519122134506,0.149213858928201,
1.3611408528136));
#16547=CARTESIAN_POINT('Ctrl Pts',(-0.0447785186189123,0.148967884123198,
1.36120171250906));
#16548=CARTESIAN_POINT('Ctrl Pts',(-0.0460969811192774,0.148563581575791,
1.36129939007872));
#16549=CARTESIAN_POINT('Ctrl Pts',(-0.0465901768561539,0.148409652138006,
1.36133606420958));
#16550=CARTESIAN_POINT('Ctrl Pts',(-0.0475227458362642,0.148113484883069,
1.36140567257607));
#16551=CARTESIAN_POINT('Ctrl Pts',(-0.0479622713609593,0.147971741536933,
1.3614385902877));
#16552=CARTESIAN_POINT('Ctrl Pts',(-0.0489569483565189,0.147646069128338,
1.36151334042957));
#16553=CARTESIAN_POINT('Ctrl Pts',(-0.0495117040588307,0.147460963191428,
1.36155521117024));
#16554=CARTESIAN_POINT('Ctrl Pts',(-0.0511495097849859,0.14690419080879,
1.361679370144));
#16555=CARTESIAN_POINT('Ctrl Pts',(-0.0522294935433872,0.146523696043513,
1.36176194832233));
#16556=CARTESIAN_POINT('Ctrl Pts',(-0.0568178536563893,0.144849973880894,
1.36211588511072));
#16557=CARTESIAN_POINT('Ctrl Pts',(-0.0602812047219647,0.143443117612085,
1.36239086377559));
#16558=CARTESIAN_POINT('Ctrl Pts',(-0.0636886474661844,0.141913912932905,
1.36266955208845));
#16559=CARTESIAN_POINT('Origin',(0.,0.,-0.129405622560373));
#16560=CARTESIAN_POINT('',(-0.0636885593981422,0.141913952456372,1.4466066640002));
#16561=CARTESIAN_POINT('',(-0.0636886279094242,0.141913921709658,1.43290478746296));
#16562=CARTESIAN_POINT('',(-0.0636886258329924,0.141913922641526,-0.129405622560373));
#16563=CARTESIAN_POINT('',(-0.15554998452487,6.93852476632616E-5,1.38940562256037));
#16564=CARTESIAN_POINT('Ctrl Pts',(-0.0636885593981421,0.141913952456372,
1.4466066640002));
#16565=CARTESIAN_POINT('Ctrl Pts',(-0.0577818439632503,0.144564785516205,
1.44610477136062));
#16566=CARTESIAN_POINT('Ctrl Pts',(-0.0517103760784334,0.14684652708226,
1.44560109607175));
#16567=CARTESIAN_POINT('Ctrl Pts',(-0.0451514202499666,0.148853254011476,
1.44507888033969));
#16568=CARTESIAN_POINT('Ctrl Pts',(-0.0447938953865853,0.148961232946105,
1.44505048298667));
#16569=CARTESIAN_POINT('Ctrl Pts',(-0.0410245876328218,0.150084834109221,
1.44475183615552));
#16570=CARTESIAN_POINT('Ctrl Pts',(-0.0375789354819654,0.150984445917234,
1.44448519240408));
#16571=CARTESIAN_POINT('Ctrl Pts',(-0.0335551471759432,0.151888684052997,
1.44418332779639));
#16572=CARTESIAN_POINT('Ctrl Pts',(-0.0330044949665369,0.152009287819579,
1.44414222263205));
#16573=CARTESIAN_POINT('Ctrl Pts',(-0.0321237319672833,0.152197180740983,
1.44407681499684));
#16574=CARTESIAN_POINT('Ctrl Pts',(-0.0317940441530217,0.152266394004828,
1.44405240740881));
#16575=CARTESIAN_POINT('Ctrl Pts',(-0.0312099338906359,0.152387039799096,
1.44400930159064));
#16576=CARTESIAN_POINT('Ctrl Pts',(-0.0309556046506675,0.152438907163245,
1.44399057886119));
#16577=CARTESIAN_POINT('Ctrl Pts',(-0.0304166696462392,0.152547412012865,
1.44395100309523));
#16578=CARTESIAN_POINT('Ctrl Pts',(-0.0301320353664039,0.152603889703489,
1.44393015923382));
#16579=CARTESIAN_POINT('Ctrl Pts',(-0.0293644953355584,0.152753955320119,
1.44387410349152));
#16580=CARTESIAN_POINT('Ctrl Pts',(-0.0288812953941729,0.152846050803369,
1.44383897534555));
#16581=CARTESIAN_POINT('Ctrl Pts',(-0.0264964975459197,0.153288868309562,
1.44366636114341));
#16582=CARTESIAN_POINT('Ctrl Pts',(-0.0245888012720797,0.153606423401509,
1.44353065367778));
#16583=CARTESIAN_POINT('Ctrl Pts',(-0.019083902879906,0.154417574327649,
1.44314455357656));
#16584=CARTESIAN_POINT('Ctrl Pts',(-0.0154745213177866,0.154820948220268,
1.44289810843775));
#16585=CARTESIAN_POINT('Ctrl Pts',(-0.00480911613752549,0.155636101335685,
1.4421809223941));
#16586=CARTESIAN_POINT('Ctrl Pts',(0.0022646345665849,0.155693943986604,
1.44171910471083));
#16587=CARTESIAN_POINT('Ctrl Pts',(0.0196580776261543,0.154650131224994,
1.44057063673603));
#16588=CARTESIAN_POINT('Ctrl Pts',(0.0299085088302777,0.152998478405293,
1.43988094496833));
#16589=CARTESIAN_POINT('Ctrl Pts',(0.0410192172414078,0.150048408023844,
1.43907602317761));
#16590=CARTESIAN_POINT('Ctrl Pts',(0.0421172723481944,0.149743901983534,
1.43899586272236));
#16591=CARTESIAN_POINT('Ctrl Pts',(0.043772630674002,0.149265200459738,
1.43887404651391));
#16592=CARTESIAN_POINT('Ctrl Pts',(0.0443324795148297,0.149099880977938,
1.43883267873659));
#16593=CARTESIAN_POINT('Ctrl Pts',(0.0453335617574274,0.148798131607573,
1.4387583983069));
#16594=CARTESIAN_POINT('Ctrl Pts',(0.0457751456257382,0.148662879785215,
1.43872552439566));
#16595=CARTESIAN_POINT('Ctrl Pts',(0.0467103315226779,0.148371881860805,
1.43865567067506));
#16596=CARTESIAN_POINT('Ctrl Pts',(0.0472037705228454,0.148215634918689,
1.43861867482091));
#16597=CARTESIAN_POINT('Ctrl Pts',(0.048520829108425,0.147791345606467,
1.43851955160848));
#16598=CARTESIAN_POINT('Ctrl Pts',(0.0493429946909558,0.14751888527274,
1.43845727994517));
#16599=CARTESIAN_POINT('Ctrl Pts',(0.0533140432296101,0.146165994816054,
1.43815455242023));
#16600=CARTESIAN_POINT('Ctrl Pts',(0.0564297389229465,0.14499160889433,
1.43791102043126));
#16601=CARTESIAN_POINT('Ctrl Pts',(0.0733461776969764,0.13798752141679,
1.43655400187372));
#16602=CARTESIAN_POINT('Ctrl Pts',(0.0862853316404953,0.130287721145884,
1.4353755561742));
#16603=CARTESIAN_POINT('Ctrl Pts',(0.0986594096163809,0.120262327467369,
1.43415525818263));
#16604=CARTESIAN_POINT('Ctrl Pts',(0.0993926787389034,0.119657018132877,
1.43408259507869));
#16605=CARTESIAN_POINT('Ctrl Pts',(0.100708129737373,0.118550685084848,
1.43395166214375));
#16606=CARTESIAN_POINT('Ctrl Pts',(0.101292236237424,0.118052002294806,
1.43389331290064));
#16607=CARTESIAN_POINT('Ctrl Pts',(0.104341615944375,0.115409288792641,
1.43358767713623));
#16608=CARTESIAN_POINT('Ctrl Pts',(0.106742811670848,0.113192106366835,
1.43334346488798));
#16609=CARTESIAN_POINT('Ctrl Pts',(0.109464630392999,0.110515155313681,
1.43306412769316));
#16610=CARTESIAN_POINT('Ctrl Pts',(0.109854628265314,0.110127496721022,
1.433024040159));
#16611=CARTESIAN_POINT('Ctrl Pts',(0.110477361758976,0.109501898620392,
1.4329599411417));
#16612=CARTESIAN_POINT('Ctrl Pts',(0.11071139891844,0.109265270867928,1.43293583093112));
#16613=CARTESIAN_POINT('Ctrl Pts',(0.111126239104583,0.108843137499665,
1.43289306127123));
#16614=CARTESIAN_POINT('Ctrl Pts',(0.111307339987436,0.108657929610833,
1.43287437865513));
#16615=CARTESIAN_POINT('Ctrl Pts',(0.111691962123727,0.108262614317263,
1.43283467723013));
#16616=CARTESIAN_POINT('Ctrl Pts',(0.111895353211077,0.108052385422434,
1.43281366848699));
#16617=CARTESIAN_POINT('Ctrl Pts',(0.11244644483601,0.107479541886851,1.43275670160171));
#16618=CARTESIAN_POINT('Ctrl Pts',(0.112792987822206,0.10711581021167,1.43272083193522));
#16619=CARTESIAN_POINT('Ctrl Pts',(0.114552659033195,0.105250849741183,
1.43253841066223));
#16620=CARTESIAN_POINT('Ctrl Pts',(0.115937689565636,0.103723219748211,
1.43239388945438));
#16621=CARTESIAN_POINT('Ctrl Pts',(0.119915291224847,0.0991568280322926,
1.43197441299661));
#16622=CARTESIAN_POINT('Ctrl Pts',(0.122421820668732,0.0960450767290035,
1.43170426801206));
#16623=CARTESIAN_POINT('Ctrl Pts',(0.131061486307808,0.0844306712315355,
1.43073700761423));
#16624=CARTESIAN_POINT('Ctrl Pts',(0.136451120246247,0.075410575303356,
1.43005973580173));
#16625=CARTESIAN_POINT('Ctrl Pts',(0.14365154759957,0.060020134466745,1.428923478612));
#16626=CARTESIAN_POINT('Ctrl Pts',(0.146037060753417,0.0539568617032269,
1.42848061335713));
#16627=CARTESIAN_POINT('Ctrl Pts',(0.148341149207721,0.0468155543687475,
1.42795485694693));
#16628=CARTESIAN_POINT('Ctrl Pts',(0.148637593005238,0.0458656575583375,
1.42788485045811));
#16629=CARTESIAN_POINT('Ctrl Pts',(0.149098227640117,0.0443382609546246,
1.42777213428897));
#16630=CARTESIAN_POINT('Ctrl Pts',(0.149268227875022,0.043762529619126,
1.42772961390418));
#16631=CARTESIAN_POINT('Ctrl Pts',(0.149564050288794,0.0427389025738611,
1.42765394815234));
#16632=CARTESIAN_POINT('Ctrl Pts',(0.149691204487337,0.0422913965544929,
1.42762084647468));
#16633=CARTESIAN_POINT('Ctrl Pts',(0.149951842233852,0.0413582061475625,
1.42755176919773));
#16634=CARTESIAN_POINT('Ctrl Pts',(0.150084977829886,0.0408724310980645,
1.42751578276327));
#16635=CARTESIAN_POINT('Ctrl Pts',(0.150424346916312,0.0396101483110438,
1.42742219469715));
#16636=CARTESIAN_POINT('Ctrl Pts',(0.15062692555304,0.0388326827286617,
1.42736447587529));
#16637=CARTESIAN_POINT('Ctrl Pts',(0.151477811000626,0.0354602509278637,
1.42711375007225));
#16638=CARTESIAN_POINT('Ctrl Pts',(0.152065112086073,0.0328505198945307,
1.42691880337861));
#16639=CARTESIAN_POINT('Ctrl Pts',(0.153442988303091,0.0258950709319782,
1.42639639379569));
#16640=CARTESIAN_POINT('Ctrl Pts',(0.154116209862769,0.0215288768052759,
1.42606549686928));
#16641=CARTESIAN_POINT('Ctrl Pts',(0.155968623241073,0.00482042250075044,
1.42478876453381));
#16642=CARTESIAN_POINT('Ctrl Pts',(0.155856938857634,-0.0076171419174825,
1.42381248347944));
#16643=CARTESIAN_POINT('Ctrl Pts',(0.153774950567523,-0.0237501082456536,
1.42257434509827));
#16644=CARTESIAN_POINT('Ctrl Pts',(0.153135890237625,-0.0275718797082024,
1.42228359891032));
#16645=CARTESIAN_POINT('Ctrl Pts',(0.152227431146282,-0.0319845317289718,
1.42195374719682));
#16646=CARTESIAN_POINT('Ctrl Pts',(0.152096361422313,-0.032602115607345,
1.42190771714814));
#16647=CARTESIAN_POINT('Ctrl Pts',(0.151892263690029,-0.033535771013551,
1.42183835162374));
#16648=CARTESIAN_POINT('Ctrl Pts',(0.15182200330985,-0.0338524300835437,
1.42181486435631));
#16649=CARTESIAN_POINT('Ctrl Pts',(0.151694145876041,-0.0344202703774804,
1.42177281888703));
#16650=CARTESIAN_POINT('Ctrl Pts',(0.151636914980676,-0.0346715290188518,
1.42175424023509));
#16651=CARTESIAN_POINT('Ctrl Pts',(0.15151129111076,-0.0352167896924782,
1.42171397842817));
#16652=CARTESIAN_POINT('Ctrl Pts',(0.151442666891154,-0.0355107344251004,
1.42169230874421));
#16653=CARTESIAN_POINT('Ctrl Pts',(0.151247774270836,-0.0363346960137935,
1.42163165965066));
#16654=CARTESIAN_POINT('Ctrl Pts',(0.151119574449685,-0.036864259088572,
1.42159278902156));
#16655=CARTESIAN_POINT('Ctrl Pts',(0.150343044405966,-0.039999784816153,
1.42136322255749));
#16656=CARTESIAN_POINT('Ctrl Pts',(0.149630051075436,-0.0425894816651851,
1.42117601860419));
#16657=CARTESIAN_POINT('Ctrl Pts',(0.144599141794687,-0.059171824955237,
1.41998507268791));
#16658=CARTESIAN_POINT('Ctrl Pts',(0.138390443961365,-0.0725148705404471,
1.41905647960248));
#16659=CARTESIAN_POINT('Ctrl Pts',(0.129303777530507,-0.0864894582732642,
1.41793636271821));
#16660=CARTESIAN_POINT('Ctrl Pts',(0.128168299171389,-0.088163370337069,
1.41779964322606));
#16661=CARTESIAN_POINT('Ctrl Pts',(0.124755382241895,-0.0929893363178283,
1.41739711657431));
#16662=CARTESIAN_POINT('Ctrl Pts',(0.122392155314658,-0.0960784993154756,
1.41712869992373));
#16663=CARTESIAN_POINT('Ctrl Pts',(0.119315148389064,-0.0998027420388395,
1.41678949072232));
#16664=CARTESIAN_POINT('Ctrl Pts',(0.118707859136016,-0.100524305832315,
1.41672301058473));
#16665=CARTESIAN_POINT('Ctrl Pts',(0.117742454555519,-0.101650424155894,
1.4166180292465));
#16666=CARTESIAN_POINT('Ctrl Pts',(0.117388721380442,-0.102058720426598,
1.41657970801144));
#16667=CARTESIAN_POINT('Ctrl Pts',(0.116760312732254,-0.102776471400776,
1.41651187971548));
#16668=CARTESIAN_POINT('Ctrl Pts',(0.116486514317401,-0.103086690115851,
1.41648240926242));
#16669=CARTESIAN_POINT('Ctrl Pts',(0.115856176468814,-0.103795156897169,
1.41641474794436));
#16670=CARTESIAN_POINT('Ctrl Pts',(0.115498817148986,-0.104192665026349,
1.41637652295596));
#16671=CARTESIAN_POINT('Ctrl Pts',(0.11450533741787,-0.105286369194166,
1.41627061864795));
#16672=CARTESIAN_POINT('Ctrl Pts',(0.113864933044019,-0.1059786241908,1.41620275869379));
#16673=CARTESIAN_POINT('Ctrl Pts',(0.110214094329664,-0.10985376323717,
1.41581811535255));
#16674=CARTESIAN_POINT('Ctrl Pts',(0.107076836824166,-0.112913860054328,
1.41549588364254));
#16675=CARTESIAN_POINT('Ctrl Pts',(0.0967251249128689,-0.12219120561543,
1.4144565926546));
#16676=CARTESIAN_POINT('Ctrl Pts',(0.0890678488002784,-0.127880071317682,
1.4137206249058));
#16677=CARTESIAN_POINT('Ctrl Pts',(0.0731533824215551,-0.137577348903586,
1.41227540112032));
#16678=CARTESIAN_POINT('Ctrl Pts',(0.0649636405681001,-0.141628791817655,
1.41156945595844));
#16679=CARTESIAN_POINT('Ctrl Pts',(0.0558273440849809,-0.145188080151334,
1.41085088590449));
#16680=CARTESIAN_POINT('Ctrl Pts',(0.0551879371257263,-0.145432329995708,
1.41080095051627));
#16681=CARTESIAN_POINT('Ctrl Pts',(0.0542371248206536,-0.14578836106835,
1.41072724074169));
#16682=CARTESIAN_POINT('Ctrl Pts',(0.0539269534087554,-0.145903377731254,
1.41070328098766));
#16683=CARTESIAN_POINT('Ctrl Pts',(0.0533810890189833,-0.146103814732317,
1.41066126798602));
#16684=CARTESIAN_POINT('Ctrl Pts',(0.0531455547277884,-0.146189655449437,
1.41064318999886));
#16685=CARTESIAN_POINT('Ctrl Pts',(0.052637320018521,-0.14637349147278,
1.41060429000276));
#16686=CARTESIAN_POINT('Ctrl Pts',(0.0523645536149028,-0.146471294092463,
1.41058347951496));
#16687=CARTESIAN_POINT('Ctrl Pts',(0.051801645183462,-0.146671356074279,
1.41054066751045));
#16688=CARTESIAN_POINT('Ctrl Pts',(0.0515114696000755,-0.146773518184855,
1.41051867172985));
#16689=CARTESIAN_POINT('Ctrl Pts',(0.0507790716106046,-0.147028933985619,
1.41046333534763));
#16690=CARTESIAN_POINT('Ctrl Pts',(0.0503364530170813,-0.147181055353175,
1.41043005885366));
#16691=CARTESIAN_POINT('Ctrl Pts',(0.0490711059691243,-0.147609560350339,
1.41033538234264));
#16692=CARTESIAN_POINT('Ctrl Pts',(0.0482467256730211,-0.14788106469746,
1.41027424557166));
#16693=CARTESIAN_POINT('Ctrl Pts',(0.0391794327031243,-0.15078342353184,
1.40960732321446));
#16694=CARTESIAN_POINT('Ctrl Pts',(0.0307317468248462,-0.15272941271282,
1.40903534193767));
#16695=CARTESIAN_POINT('Ctrl Pts',(0.00998667550152534,-0.155715935731724,
1.40765481029465));
#16696=CARTESIAN_POINT('Ctrl Pts',(-0.00235482521677464,-0.15601792333516,
1.4068500850827));
#16697=CARTESIAN_POINT('Ctrl Pts',(-0.0163125766955438,-0.154701820547001,
1.40587548298647));
#16698=CARTESIAN_POINT('Ctrl Pts',(-0.0180199694970762,-0.154512244590398,
1.40575524130209));
#16699=CARTESIAN_POINT('Ctrl Pts',(-0.020417841358966,-0.154205719083121,
1.40558477863521));
#16700=CARTESIAN_POINT('Ctrl Pts',(-0.0211112508531559,-0.154112319761558,
1.40553529663746));
#16701=CARTESIAN_POINT('Ctrl Pts',(-0.0222329614871399,-0.153953517733336,
1.40545493600479));
#16702=CARTESIAN_POINT('Ctrl Pts',(-0.0226616668443592,-0.153890997293083,
1.40542414843897));
#16703=CARTESIAN_POINT('Ctrl Pts',(-0.0235553598542659,-0.153756849814088,
1.40535980913494));
#16704=CARTESIAN_POINT('Ctrl Pts',(-0.0240202942240823,-0.15368490263867,
1.40532624759488));
#16705=CARTESIAN_POINT('Ctrl Pts',(-0.0251198653098533,-0.153509635866561,
1.40524665827793));
#16706=CARTESIAN_POINT('Ctrl Pts',(-0.0257541975902381,-0.15340448891919,
1.40520057318147));
#16707=CARTESIAN_POINT('Ctrl Pts',(-0.0278623127734888,-0.1530416037679,
1.40504683501376));
#16708=CARTESIAN_POINT('Ctrl Pts',(-0.0293329861536879,-0.152766542768491,
1.40493863630077));
#16709=CARTESIAN_POINT('Ctrl Pts',(-0.0371368685561892,-0.151190137438781,
1.40435925555681));
#16710=CARTESIAN_POINT('Ctrl Pts',(-0.0433874191859156,-0.149516270007874,
1.4038763527493));
#16711=CARTESIAN_POINT('Ctrl Pts',(-0.0582212203167935,-0.14453524535105,
1.40268457695414));
#16712=CARTESIAN_POINT('Ctrl Pts',(-0.0666510649336296,-0.140846590084201,
1.40196765960564));
#16713=CARTESIAN_POINT('Ctrl Pts',(-0.0803791378116622,-0.133329807803446,
1.4007597024399));
#16714=CARTESIAN_POINT('Ctrl Pts',(-0.0858542800401925,-0.129871894198812,
1.40026609142151));
#16715=CARTESIAN_POINT('Ctrl Pts',(-0.0916664649086831,-0.125672400356744,
1.39974042420532));
#16716=CARTESIAN_POINT('Ctrl Pts',(-0.0922313841861929,-0.12525839221855,
1.39968931597493));
#16717=CARTESIAN_POINT('Ctrl Pts',(-0.0930614944153107,-0.124641374578354,
1.3996142155801));
#16718=CARTESIAN_POINT('Ctrl Pts',(-0.0933288480639727,-0.124441311968053,
1.39959002794176));
#16719=CARTESIAN_POINT('Ctrl Pts',(-0.0937939489664914,-0.124090931711175,
1.39954795286849));
#16720=CARTESIAN_POINT('Ctrl Pts',(-0.0939919822351667,-0.123940999974898,
1.39953003893238));
#16721=CARTESIAN_POINT('Ctrl Pts',(-0.094417058220138,-0.123617568589008,
1.39949158978689));
#16722=CARTESIAN_POINT('Ctrl Pts',(-0.0946439818366814,-0.123443917843267,
1.3994710654618));
#16723=CARTESIAN_POINT('Ctrl Pts',(-0.0952439703452555,-0.122982156404739,
1.39941679891469));
#16724=CARTESIAN_POINT('Ctrl Pts',(-0.0956162103718621,-0.122692970502384,
1.39938313129306));
#16725=CARTESIAN_POINT('Ctrl Pts',(-0.0964419594738644,-0.12204542199597,
1.3993084308861));
#16726=CARTESIAN_POINT('Ctrl Pts',(-0.0968948000376298,-0.121686212571192,
1.39926745523872));
#16727=CARTESIAN_POINT('Ctrl Pts',(-0.0982558445771977,-0.120594167936516,
1.39914423307526));
#16728=CARTESIAN_POINT('Ctrl Pts',(-0.0991578384285692,-0.119853609089712,
1.39906248024986));
#16729=CARTESIAN_POINT('Ctrl Pts',(-0.102464323851287,-0.117076023258314,
1.39876208604954));
#16730=CARTESIAN_POINT('Ctrl Pts',(-0.104815233622259,-0.11497609589624,
1.39854709117054));
#16731=CARTESIAN_POINT('Ctrl Pts',(-0.115228207152847,-0.105089757898351,
1.39757939922236));
#16732=CARTESIAN_POINT('Ctrl Pts',(-0.122498157472708,-0.0965174939919779,
1.39685756992712));
#16733=CARTESIAN_POINT('Ctrl Pts',(-0.132690416520789,-0.0814712820860795,
1.39564527760622));
#16734=CARTESIAN_POINT('Ctrl Pts',(-0.136204499238017,-0.0754495189133748,
1.39517261860127));
#16735=CARTESIAN_POINT('Ctrl Pts',(-0.139750888521818,-0.0683118193043369,
1.39461428236302));
#16736=CARTESIAN_POINT('Ctrl Pts',(-0.140189960618132,-0.0674061596364181,
1.39454348279125));
#16737=CARTESIAN_POINT('Ctrl Pts',(-0.140878260102637,-0.06595060823246,
1.3944297338395));
#16738=CARTESIAN_POINT('Ctrl Pts',(-0.141133134085882,-0.0654034046535807,
1.39438697937938));
#16739=CARTESIAN_POINT('Ctrl Pts',(-0.141578995342617,-0.0644314169132236,
1.39431104373391));
#16740=CARTESIAN_POINT('Ctrl Pts',(-0.141771273283171,-0.0640072298315101,
1.39427790730606));
#16741=CARTESIAN_POINT('Ctrl Pts',(-0.142166912323166,-0.0631238760545666,
1.39420890434326));
#16742=CARTESIAN_POINT('Ctrl Pts',(-0.142369960313065,-0.0626645759357227,
1.39417302757229));
#16743=CARTESIAN_POINT('Ctrl Pts',(-0.142889335642401,-0.0614741801206648,
1.39408004221332));
#16744=CARTESIAN_POINT('Ctrl Pts',(-0.143202273898766,-0.0607416312609533,
1.39402281925644));
#16745=CARTESIAN_POINT('Ctrl Pts',(-0.144517074735001,-0.0575972086573725,
1.39377715921711));
#16746=CARTESIAN_POINT('Ctrl Pts',(-0.14546367967645,-0.0551628470339443,
1.39358687824211));
#16747=CARTESIAN_POINT('Ctrl Pts',(-0.147795945942313,-0.0486868470246648,
1.39308005716341));
#16748=CARTESIAN_POINT('Ctrl Pts',(-0.149077076666379,-0.0446101987501447,
1.39276033245939));
#16749=CARTESIAN_POINT('Ctrl Pts',(-0.15375309343562,-0.0272639702260042,
1.39139765354976));
#16750=CARTESIAN_POINT('Ctrl Pts',(-0.15555526912902,-0.0136311345579096,
1.39031463336019));
#16751=CARTESIAN_POINT('Ctrl Pts',(-0.15554998842971,5.99959743726453E-5,
1.38928122911086));
#16752=CARTESIAN_POINT('Ctrl Pts',(-0.0636886258329916,0.141913922641527,
1.37660119646451));
#16753=CARTESIAN_POINT('Ctrl Pts',(-0.0672646134278248,0.140309078439693,
1.3768829359352));
#16754=CARTESIAN_POINT('Ctrl Pts',(-0.0707755899134079,0.138570924731718,
1.3771646754059));
#16755=CARTESIAN_POINT('Ctrl Pts',(-0.0742113165068752,0.136705826511954,
1.37744641487659));
#16756=CARTESIAN_POINT('Ctrl Pts',(-0.0832025825392944,0.131824881007623,
1.37818372457337));
#16757=CARTESIAN_POINT('Ctrl Pts',(-0.0917439477378679,0.12603479045185,
1.37892103427014));
#16758=CARTESIAN_POINT('Ctrl Pts',(-0.0996465697393686,0.11944188394017,
1.37965834396692));
#16759=CARTESIAN_POINT('Ctrl Pts',(-0.107598376984517,0.112807943742069,
1.38040024261621));
#16760=CARTESIAN_POINT('Ctrl Pts',(-0.114902627518598,0.105361621827393,
1.38114214126549));
#16761=CARTESIAN_POINT('Ctrl Pts',(-0.121396743056803,0.0972555051151373,
1.38188403991478));
#16762=CARTESIAN_POINT('Ctrl Pts',(-0.127835842296946,0.0892180611159775,
1.38261965340992));
#16763=CARTESIAN_POINT('Ctrl Pts',(-0.133477910941686,0.080532706875503,
1.38335526690506));
#16764=CARTESIAN_POINT('Ctrl Pts',(-0.138204096147797,0.0713822828716657,
1.3840908804002));
#16765=CARTESIAN_POINT('Ctrl Pts',(-0.142990852841695,0.0621145856820285,
1.38483592162656));
#16766=CARTESIAN_POINT('Ctrl Pts',(-0.14683759102957,0.052370652666543,
1.38558096285292));
#16767=CARTESIAN_POINT('Ctrl Pts',(-0.14967002282687,0.0423637435433198,
1.38632600407929));
#16768=CARTESIAN_POINT('Ctrl Pts',(-0.152502454624171,0.0323568344200951,
1.38707104530565));
#16769=CARTESIAN_POINT('Ctrl Pts',(-0.154320443732021,0.0220879207575721,
1.38781608653201));
#16770=CARTESIAN_POINT('Ctrl Pts',(-0.155103327025007,0.0117796623794456,
1.38856112775838));
#16771=CARTESIAN_POINT('Ctrl Pts',(-0.155399123126889,0.0078849022373452,
1.38884262602571));
#16772=CARTESIAN_POINT('Ctrl Pts',(-0.155548240648023,0.00397886205704992,
1.38912412429304));
#16773=CARTESIAN_POINT('Ctrl Pts',(-0.15554998452487,6.93852476632616E-5,
1.38940562256037));
#16774=CARTESIAN_POINT('Ctrl Pts',(-0.0636886474661844,0.141913912932905,
1.36266955208845));
#16775=CARTESIAN_POINT('Ctrl Pts',(-0.0688639616191303,0.139591316424911,
1.3630928312682));
#16776=CARTESIAN_POINT('Ctrl Pts',(-0.0739102973562643,0.1369864912641,
1.36352480444837));
#16777=CARTESIAN_POINT('Ctrl Pts',(-0.0856921396542741,0.130063343831725,
1.36457710306135));
#16778=CARTESIAN_POINT('Ctrl Pts',(-0.0922573124579418,0.125491841598355,
1.36520095550586));
#16779=CARTESIAN_POINT('Ctrl Pts',(-0.101258002258513,0.118134858423088,
1.36609348767914));
#16780=CARTESIAN_POINT('Ctrl Pts',(-0.103992376674986,0.11573511776738,
1.36637012355003));
#16781=CARTESIAN_POINT('Ctrl Pts',(-0.108049550126467,0.111914451201318,
1.36678632492678));
#16782=CARTESIAN_POINT('Ctrl Pts',(-0.109433993044875,0.110561077140873,
1.36692943653171));
#16783=CARTESIAN_POINT('Ctrl Pts',(-0.111138206297609,0.108831721599176,
1.36710659491168));
#16784=CARTESIAN_POINT('Ctrl Pts',(-0.111481860535304,0.108479672356529,
1.36714237079528));
#16785=CARTESIAN_POINT('Ctrl Pts',(-0.11202552556295,0.107917414267432,
1.36719904304916));
#16786=CARTESIAN_POINT('Ctrl Pts',(-0.112226624449519,0.107708270101527,
1.36722002217535));
#16787=CARTESIAN_POINT('Ctrl Pts',(-0.11260645338804,0.107311026825936,
1.36725967580905));
#16788=CARTESIAN_POINT('Ctrl Pts',(-0.112785295681815,0.107123045617149,
1.36727835868759));
#16789=CARTESIAN_POINT('Ctrl Pts',(-0.113195109737595,0.106690125923971,
1.36732119946899));
#16790=CARTESIAN_POINT('Ctrl Pts',(-0.113425757291714,0.106444884455639,
1.36734533239698));
#16791=CARTESIAN_POINT('Ctrl Pts',(-0.114040092506407,0.105787413916382,
1.36740967563519));
#16792=CARTESIAN_POINT('Ctrl Pts',(-0.11442234565153,0.105373841552063,
1.36744977931787));
#16793=CARTESIAN_POINT('Ctrl Pts',(-0.117197768009641,0.102338108916556,
1.36774154067777));
#16794=CARTESIAN_POINT('Ctrl Pts',(-0.119503030045236,0.0996365205062875,
1.36798706129001));
#16795=CARTESIAN_POINT('Ctrl Pts',(-0.123008176081925,0.0952318784020268,
1.36837005112417));
#16796=CARTESIAN_POINT('Ctrl Pts',(-0.124269654302658,0.0935797826475085,
1.36851006608177));
#16797=CARTESIAN_POINT('Ctrl Pts',(-0.131659610814762,0.0834884465253215,
1.36934701413561));
#16798=CARTESIAN_POINT('Ctrl Pts',(-0.136959759196717,0.0744755810458954,
1.37002091294087));
#16799=CARTESIAN_POINT('Ctrl Pts',(-0.143918970474773,0.0593453450142004,
1.37113303291619));
#16800=CARTESIAN_POINT('Ctrl Pts',(-0.146177765129095,0.0535405087759689,
1.37155524821357));
#16801=CARTESIAN_POINT('Ctrl Pts',(-0.148531329392937,0.0462211527850203,
1.37209148393496));
#16802=CARTESIAN_POINT('Ctrl Pts',(-0.148960246835224,0.0448195870285426,
1.37219431909291));
#16803=CARTESIAN_POINT('Ctrl Pts',(-0.149547219814545,0.0427999770713411,
1.37234281282051));
#16804=CARTESIAN_POINT('Ctrl Pts',(-0.149721389143636,0.0421866638001736,
1.37238794802417));
#16805=CARTESIAN_POINT('Ctrl Pts',(-0.150017235197604,0.041119970684242,
1.37246652720118));
#16806=CARTESIAN_POINT('Ctrl Pts',(-0.150140640195161,0.040667075114373,
1.37249991478166));
#16807=CARTESIAN_POINT('Ctrl Pts',(-0.150374273564743,0.0397940822154385,
1.3725643224015));
#16808=CARTESIAN_POINT('Ctrl Pts',(-0.150484796326114,0.03937406757158,
1.37259533258));
#16809=CARTESIAN_POINT('Ctrl Pts',(-0.150770357516921,0.0382700957634074,
1.37267690199069));
#16810=CARTESIAN_POINT('Ctrl Pts',(-0.150942499280473,0.0375854069555614,
1.37272755397808));
#16811=CARTESIAN_POINT('Ctrl Pts',(-0.151526536980619,0.0351936746013996,
1.37290472285196));
#16812=CARTESIAN_POINT('Ctrl Pts',(-0.151914168737528,0.0334809051298725,
1.37303201180024));
#16813=CARTESIAN_POINT('Ctrl Pts',(-0.154461931925954,0.021266474322541,
1.37394307218985));
#16814=CARTESIAN_POINT('Ctrl Pts',(-0.155559753193871,0.0105748508364614,
1.37476089397571));
#16815=CARTESIAN_POINT('Ctrl Pts',(-0.15554787850174,-0.00238697431566608,
1.37576482688623));
#16816=CARTESIAN_POINT('Ctrl Pts',(-0.155497243431645,-0.00463113013496754,
1.37593896517501));
#16817=CARTESIAN_POINT('Ctrl Pts',(-0.155371172290793,-0.00748142693314287,
1.37616018003544));
#16818=CARTESIAN_POINT('Ctrl Pts',(-0.155340709994526,-0.00808929843285904,
1.37620735973367));
#16819=CARTESIAN_POINT('Ctrl Pts',(-0.155068274409692,-0.012954330088632,
1.37658492140736));
#16820=CARTESIAN_POINT('Ctrl Pts',(-0.15465489931931,-0.0172002902653275,
1.37691427835633));
#16821=CARTESIAN_POINT('Ctrl Pts',(-0.153955734643448,-0.0222282118735399,
1.37730091160018));
#16822=CARTESIAN_POINT('Ctrl Pts',(-0.153837619047051,-0.0230314707409262,
1.37736257448975));
#16823=CARTESIAN_POINT('Ctrl Pts',(-0.153221742392761,-0.0270034959724454,
1.37766686266045));
#16824=CARTESIAN_POINT('Ctrl Pts',(-0.152632292925795,-0.0301575550367337,
1.37790651831394));
#16825=CARTESIAN_POINT('Ctrl Pts',(-0.151828632635557,-0.0338255498098905,
1.37818125199822));
#16826=CARTESIAN_POINT('Ctrl Pts',(-0.151708782838084,-0.034359085284491,
1.37822111435406));
#16827=CARTESIAN_POINT('Ctrl Pts',(-0.151511680585906,-0.0352153840253586,
1.37828491943834));
#16828=CARTESIAN_POINT('Ctrl Pts',(-0.151436205901583,-0.0355385449017062,
1.3783089595231));
#16829=CARTESIAN_POINT('Ctrl Pts',(-0.151300020903333,-0.0361133379153534,
1.37835164532919));
#16830=CARTESIAN_POINT('Ctrl Pts',(-0.151239716149397,-0.0363650624067039,
1.37837031392336));
#16831=CARTESIAN_POINT('Ctrl Pts',(-0.151109827927862,-0.0369013306867755,
1.37841003056709));
#16832=CARTESIAN_POINT('Ctrl Pts',(-0.151040069148171,-0.0371858281933781,
1.37843106836598));
#16833=CARTESIAN_POINT('Ctrl Pts',(-0.150847979326769,-0.0379597701411314,
1.37848821522442));
#16834=CARTESIAN_POINT('Ctrl Pts',(-0.150724068690257,-0.0384488251123607,
1.37852423481855));
#16835=CARTESIAN_POINT('Ctrl Pts',(-0.150074597528192,-0.0409607858908205,
1.37870881429158));
#16836=CARTESIAN_POINT('Ctrl Pts',(-0.149510651397193,-0.0429736789304506,
1.37885528568167));
#16837=CARTESIAN_POINT('Ctrl Pts',(-0.147727364648117,-0.048877941345908,
1.37928234904023));
#16838=CARTESIAN_POINT('Ctrl Pts',(-0.14639534406895,-0.0527336349159576,
1.37955792098303));
#16839=CARTESIAN_POINT('Ctrl Pts',(-0.141127032686453,-0.0662381431887435,
1.38052583986846));
#16840=CARTESIAN_POINT('Ctrl Pts',(-0.136375449259961,-0.0755385871689743,
1.38119924533695));
#16841=CARTESIAN_POINT('Ctrl Pts',(-0.127228917362253,-0.0897236731873988,
1.38232824946926));
#16842=CARTESIAN_POINT('Ctrl Pts',(-0.123393759470827,-0.0949289090939788,
1.38276783184552));
#16843=CARTESIAN_POINT('Ctrl Pts',(-0.118608548226377,-0.100641949577517,
1.38328999288634));
#16844=CARTESIAN_POINT('Ctrl Pts',(-0.117963281886143,-0.101397503779286,
1.38335989613302));
#16845=CARTESIAN_POINT('Ctrl Pts',(-0.116916974779799,-0.102599138572368,
1.38347247080913));
#16846=CARTESIAN_POINT('Ctrl Pts',(-0.11652050726507,-0.103049180471761,
1.38351495363448));
#16847=CARTESIAN_POINT('Ctrl Pts',(-0.115812045556906,-0.103844060242853,
1.38359056746984));
#16848=CARTESIAN_POINT('Ctrl Pts',(-0.115501087177952,-0.104189815221598,
1.3836236549275));
#16849=CARTESIAN_POINT('Ctrl Pts',(-0.114850095895701,-0.104907157382385,
1.38369271753777));
#16850=CARTESIAN_POINT('Ctrl Pts',(-0.11450979969522,-0.105278497140006,
1.38372870358017));
#16851=CARTESIAN_POINT('Ctrl Pts',(-0.11362172833703,-0.106238183138333,
1.38382232323869));
#16852=CARTESIAN_POINT('Ctrl Pts',(-0.113071191298008,-0.106823940950737,
1.38388007426121));
#16853=CARTESIAN_POINT('Ctrl Pts',(-0.110665377499298,-0.10934423242774,
1.38413124219618));
#16854=CARTESIAN_POINT('Ctrl Pts',(-0.108764916641453,-0.111234788575827,
1.38432660762635));
#16855=CARTESIAN_POINT('Ctrl Pts',(-0.103596561826311,-0.116117083257788,
1.38485045490948));
#16856=CARTESIAN_POINT('Ctrl Pts',(-0.100248288453831,-0.119019740265329,
1.38518239493091));
#16857=CARTESIAN_POINT('Ctrl Pts',(-0.087118820782712,-0.129454390059997,
1.3864562449401));
#16858=CARTESIAN_POINT('Ctrl Pts',(-0.076578204865397,-0.13595538070058,
1.38742818457375));
#16859=CARTESIAN_POINT('Ctrl Pts',(-0.0618381345820382,-0.142783373288334,
1.38866493250698));
#16860=CARTESIAN_POINT('Ctrl Pts',(-0.0582344820537444,-0.144290672531536,
1.38895809129996));
#16861=CARTESIAN_POINT('Ctrl Pts',(-0.0539853604612679,-0.145882772414045,
1.38929032318999));
#16862=CARTESIAN_POINT('Ctrl Pts',(-0.0533918028628148,-0.146101053573369,
1.38933643295144));
#16863=CARTESIAN_POINT('Ctrl Pts',(-0.0524916553017162,-0.146425865002342,
1.38940589021137));
#16864=CARTESIAN_POINT('Ctrl Pts',(-0.0521860458781278,-0.146535062148398,
1.38942939013984));
#16865=CARTESIAN_POINT('Ctrl Pts',(-0.0516372166121848,-0.146729229306329,
1.389471443637));
#16866=CARTESIAN_POINT('Ctrl Pts',(-0.0513941266457318,-0.146814551806214,
1.38949001773675));
#16867=CARTESIAN_POINT('Ctrl Pts',(-0.0508660585021629,-0.146998426907031,
1.38953025258091));
#16868=CARTESIAN_POINT('Ctrl Pts',(-0.0505810061857008,-0.147096754682547,
1.3895518999392));
#16869=CARTESIAN_POINT('Ctrl Pts',(-0.0497811979379651,-0.147370045845346,
1.38961244336106));
#16870=CARTESIAN_POINT('Ctrl Pts',(-0.0492658010752367,-0.14754314266875,
1.38965123120975));
#16871=CARTESIAN_POINT('Ctrl Pts',(-0.0462163811985503,-0.148549534419033,
1.38987945017749));
#16872=CARTESIAN_POINT('Ctrl Pts',(-0.0436619728792823,-0.149320301683406,
1.39006543660367));
#16873=CARTESIAN_POINT('Ctrl Pts',(-0.0269586552924137,-0.153894999942996,
1.39125593265297));
#16874=CARTESIAN_POINT('Ctrl Pts',(-0.0123513654010456,-0.155749765170369,
1.39218496841677));
#16875=CARTESIAN_POINT('Ctrl Pts',(0.00427533182359346,-0.155503769413597,
1.39330228050662));
#16876=CARTESIAN_POINT('Ctrl Pts',(0.00624872162983864,-0.155436976886721,
1.39343571467272));
#16877=CARTESIAN_POINT('Ctrl Pts',(0.0121562485200483,-0.155124348832398,
1.39383840526435));
#16878=CARTESIAN_POINT('Ctrl Pts',(0.016082589362646,-0.15476654604438,
1.39411040583891));
#16879=CARTESIAN_POINT('Ctrl Pts',(0.0209301905851279,-0.15413833662402,
1.39445361014386));
#16880=CARTESIAN_POINT('Ctrl Pts',(0.0218683890596436,-0.15400802960993,
1.39452037592705));
#16881=CARTESIAN_POINT('Ctrl Pts',(0.0233405248334821,-0.153789840809534,
1.39462570306025));
#16882=CARTESIAN_POINT('Ctrl Pts',(0.0238753052025794,-0.153707725972915,
1.39466408239205));
#16883=CARTESIAN_POINT('Ctrl Pts',(0.0248181253091664,-0.153557918157794,
1.39473195725703));
#16884=CARTESIAN_POINT('Ctrl Pts',(0.0252263462605754,-0.153491384191743,
1.39476141587294));
#16885=CARTESIAN_POINT('Ctrl Pts',(0.0261603880445246,-0.153335322413091,
1.39482898301296));
#16886=CARTESIAN_POINT('Ctrl Pts',(0.0266860209431342,-0.153244716957228,
1.39486712533358));
#16887=CARTESIAN_POINT('Ctrl Pts',(0.028135011055712,-0.152987267690811,
1.39497260490883));
#16888=CARTESIAN_POINT('Ctrl Pts',(0.0290573272660953,-0.15281477213631,
1.3950401204951));
#16889=CARTESIAN_POINT('Ctrl Pts',(0.0342061668073188,-0.151803516406592,
1.39541918648165));
#16890=CARTESIAN_POINT('Ctrl Pts',(0.0383975681508075,-0.150797842921769,
1.39573600115996));
#16891=CARTESIAN_POINT('Ctrl Pts',(0.0514255078870773,-0.147093597668828,
1.39674807775293));
#16892=CARTESIAN_POINT('Ctrl Pts',(0.0600657864033322,-0.143781665621738,
1.39746102473362));
#16893=CARTESIAN_POINT('Ctrl Pts',(0.0762490817109134,-0.135863950107734,
1.3988582510672));
#16894=CARTESIAN_POINT('Ctrl Pts',(0.0837979015692544,-0.131342613888997,
1.39953943577331));
#16895=CARTESIAN_POINT('Ctrl Pts',(0.0918683127884089,-0.125528348512753,
1.40027478385204));
#16896=CARTESIAN_POINT('Ctrl Pts',(0.0928036634911799,-0.124838429317268,
1.40036010968599));
#16897=CARTESIAN_POINT('Ctrl Pts',(0.0940687339961342,-0.123883229831781,
1.40047555555102));
#16898=CARTESIAN_POINT('Ctrl Pts',(0.0944052023409424,-0.123627016187872,
1.40050626454325));
#16899=CARTESIAN_POINT('Ctrl Pts',(0.0949368675241207,-0.12321872790308,
1.40055478991603));
#16900=CARTESIAN_POINT('Ctrl Pts',(0.0951327502078574,-0.12306755690102,
1.40057266846064));
#16901=CARTESIAN_POINT('Ctrl Pts',(0.0955353687750359,-0.122755303341884,
1.40060941517653));
#16902=CARTESIAN_POINT('Ctrl Pts',(0.095742058273858,-0.122594165702152,
1.40062827881778));
#16903=CARTESIAN_POINT('Ctrl Pts',(0.0962314913249354,-0.122210605068048,
1.40067294767757));
#16904=CARTESIAN_POINT('Ctrl Pts',(0.0965138747426703,-0.12198772029559,
1.40069872029979));
#16905=CARTESIAN_POINT('Ctrl Pts',(0.0974540977165782,-0.121240295371979,
1.40078454409008));
#16906=CARTESIAN_POINT('Ctrl Pts',(0.0981084701426475,-0.120711385354342,
1.40084429400798));
#16907=CARTESIAN_POINT('Ctrl Pts',(0.104176922246356,-0.115724486195703,
1.40139892205179));
#16908=CARTESIAN_POINT('Ctrl Pts',(0.109288818738309,-0.110909744696904,
1.40187021526625));
#16909=CARTESIAN_POINT('Ctrl Pts',(0.119108621941048,-0.100319960387341,
1.40282760177878));
#16910=CARTESIAN_POINT('Ctrl Pts',(0.12376188341211,-0.0945196069906272,
1.40331190100052));
#16911=CARTESIAN_POINT('Ctrl Pts',(0.13253147237701,-0.0818245379964986,
1.40433611051396));
#16912=CARTESIAN_POINT('Ctrl Pts',(0.136564372787938,-0.0748998598947808,
1.40487608075201));
#16913=CARTESIAN_POINT('Ctrl Pts',(0.14049422660366,-0.0667700047747948,
1.40550843858125));
#16914=CARTESIAN_POINT('Ctrl Pts',(0.140932821439027,-0.0658392056291265,
1.4055808012198));
#16915=CARTESIAN_POINT('Ctrl Pts',(0.141616710180522,-0.0643496862914652,
1.4056965762208));
#16916=CARTESIAN_POINT('Ctrl Pts',(0.141868012452856,-0.0637937438284535,
1.40573978231875));
#16917=CARTESIAN_POINT('Ctrl Pts',(0.142305738899494,-0.0628100065914654,
1.40581623300461));
#16918=CARTESIAN_POINT('Ctrl Pts',(0.142493522022308,-0.0623828215516508,
1.40584943073304));
#16919=CARTESIAN_POINT('Ctrl Pts',(0.142878199657009,-0.0614969246758663,
1.40591827805429));
#16920=CARTESIAN_POINT('Ctrl Pts',(0.143074813656206,-0.0610380976796266,
1.40595393672606));
#16921=CARTESIAN_POINT('Ctrl Pts',(0.14357432231333,-0.0598567477798282,
1.40604575505881));
#16922=CARTESIAN_POINT('Ctrl Pts',(0.14387396983893,-0.0591328761656403,
1.40610202376271));
#16923=CARTESIAN_POINT('Ctrl Pts',(0.145105210971574,-0.0560937474687334,
1.4063383199317));
#16924=CARTESIAN_POINT('Ctrl Pts',(0.145986435800257,-0.0537586269911329,
1.40652002130098));
#16925=CARTESIAN_POINT('Ctrl Pts',(0.14813692276093,-0.0476167175418052,
1.40699864410027));
#16926=CARTESIAN_POINT('Ctrl Pts',(0.149315663517163,-0.0437804430263291,
1.4072983266247));
#16927=CARTESIAN_POINT('Ctrl Pts',(0.15239855114542,-0.0321649330990623,
1.40820768137138));
#16928=CARTESIAN_POINT('Ctrl Pts',(0.153851703617052,-0.0242802937348053,
1.40882823696877));
#16929=CARTESIAN_POINT('Ctrl Pts',(0.155614324890464,-0.00757268786725114,
1.41013088802435));
#16930=CARTESIAN_POINT('Ctrl Pts',(0.15579368843639,0.00123804627988295,
1.41081073047552));
#16931=CARTESIAN_POINT('Ctrl Pts',(0.155182541497356,0.0107079265542668,
1.41150627780658));
#16932=CARTESIAN_POINT('Ctrl Pts',(0.1551333939331,0.0113978511779808,1.4115567440063));
#16933=CARTESIAN_POINT('Ctrl Pts',(0.155053833879795,0.0124185919313914,
1.4116310789295));
#16934=CARTESIAN_POINT('Ctrl Pts',(0.155026961979705,0.0127496624003516,
1.41165513758687));
#16935=CARTESIAN_POINT('Ctrl Pts',(0.154977310630607,0.0133380056281854,
1.41169779774452));
#16936=CARTESIAN_POINT('Ctrl Pts',(0.154954950762529,0.0135953095755898,
1.41171642234768));
#16937=CARTESIAN_POINT('Ctrl Pts',(0.154905572837179,0.0141475697135342,
1.41175632715783));
#16938=CARTESIAN_POINT('Ctrl Pts',(0.15487835325053,0.0144425040492692,
1.4117775959032));
#16939=CARTESIAN_POINT('Ctrl Pts',(0.154801094654367,0.0152542854216299,
1.41183602401434));
#16940=CARTESIAN_POINT('Ctrl Pts',(0.154749309172403,0.0157709689358164,
1.41187308702776));
#16941=CARTESIAN_POINT('Ctrl Pts',(0.154455251342063,0.0185638810093464,
1.41207279890991));
#16942=CARTESIAN_POINT('Ctrl Pts',(0.154165327161617,0.020834964468423,
1.41223292957326));
#16943=CARTESIAN_POINT('Ctrl Pts',(0.151705237384277,0.037217687789671,
1.41337705047185));
#16944=CARTESIAN_POINT('Ctrl Pts',(0.147651269347817,0.0509789121898426,
1.41428422010012));
#16945=CARTESIAN_POINT('Ctrl Pts',(0.139116595903316,0.0698867453134283,
1.41567183097907));
#16946=CARTESIAN_POINT('Ctrl Pts',(0.13609296513136,0.0756060312159878,
1.41611166482707));
#16947=CARTESIAN_POINT('Ctrl Pts',(0.132204490486604,0.0819680585372037,
1.41663410024237));
#16948=CARTESIAN_POINT('Ctrl Pts',(0.13167817246175,0.0828109216298087,
1.41670401042212));
#16949=CARTESIAN_POINT('Ctrl Pts',(0.130821275621213,0.0841543588142361,
1.41681659413094));
#16950=CARTESIAN_POINT('Ctrl Pts',(0.130495807571174,0.0846581741517003,
1.41685907900717));
#16951=CARTESIAN_POINT('Ctrl Pts',(0.129912847467376,0.0855492303343974,
1.41693469520173));
#16952=CARTESIAN_POINT('Ctrl Pts',(0.129656515867659,0.0859372249514269,
1.41696778295836));
#16953=CARTESIAN_POINT('Ctrl Pts',(0.129118933912947,0.086743052107196,
1.41703684489041));
#16954=CARTESIAN_POINT('Ctrl Pts',(0.128837386665819,0.0871606790347807,
1.41707282995029));
#16955=CARTESIAN_POINT('Ctrl Pts',(0.128101263028642,0.0882412319664316,
1.41716644421233));
#16956=CARTESIAN_POINT('Ctrl Pts',(0.127643572574545,0.0889020075356767,
1.41722419079551));
#16957=CARTESIAN_POINT('Ctrl Pts',(0.125637867168078,0.0917502599931941,
1.41747531281612));
#16958=CARTESIAN_POINT('Ctrl Pts',(0.124038677058333,0.0939009521213358,
1.4176706358889));
#16959=CARTESIAN_POINT('Ctrl Pts',(0.119651533789701,0.0994933334042916,
1.4181943407255));
#16960=CARTESIAN_POINT('Ctrl Pts',(0.11677095914559,0.102858880511751,1.41852617831983));
#16961=CARTESIAN_POINT('Ctrl Pts',(0.105328564155101,0.115126780803263,
1.41980038714684));
#16962=CARTESIAN_POINT('Ctrl Pts',(0.0958618624554302,0.123120852445625,
1.4207728349456));
#16963=CARTESIAN_POINT('Ctrl Pts',(0.0843944804491291,0.13067245096559,
1.42181814082777));
#16964=CARTESIAN_POINT('Ctrl Pts',(0.0832285118141076,0.131418160214536,
1.42192299000539));
#16965=CARTESIAN_POINT('Ctrl Pts',(0.0798181917657878,0.133535676281692,
1.42222522710932));
#16966=CARTESIAN_POINT('Ctrl Pts',(0.0775486571921883,0.13486633591645,
1.42242089121785));
#16967=CARTESIAN_POINT('Ctrl Pts',(0.0747957817238612,0.136387897179991,
1.42265083862931));
#16968=CARTESIAN_POINT('Ctrl Pts',(0.0743440313754666,0.136634667927714,
1.42268833992154));
#16969=CARTESIAN_POINT('Ctrl Pts',(0.0736044233517935,0.137033928146401,
1.42274934712946));
#16970=CARTESIAN_POINT('Ctrl Pts',(0.073317301908686,0.137187761284676,
1.42277293518221));
#16971=CARTESIAN_POINT('Ctrl Pts',(0.0728076029199767,0.137458789202218,
1.42281463717451));
#16972=CARTESIAN_POINT('Ctrl Pts',(0.072585223292913,0.137576346567206,
1.42283277379023));
#16973=CARTESIAN_POINT('Ctrl Pts',(0.0721044479318759,0.137829010395008,
1.42287185937288));
#16974=CARTESIAN_POINT('Ctrl Pts',(0.0718459579075506,0.137963929540243,
1.42289279647424));
#16975=CARTESIAN_POINT('Ctrl Pts',(0.0713099135085865,0.138241803391027,
1.4229360581229));
#16976=CARTESIAN_POINT('Ctrl Pts',(0.0710323047159421,0.138384651102189,
1.42295837599763));
#16977=CARTESIAN_POINT('Ctrl Pts',(0.0703275649086268,0.138744605968689,
1.42301481791084));
#16978=CARTESIAN_POINT('Ctrl Pts',(0.069899853326939,0.138960579273107,
1.42304887398363));
#16979=CARTESIAN_POINT('Ctrl Pts',(0.0686683520551014,0.139575302188463,
1.42314638071538));
#16980=CARTESIAN_POINT('Ctrl Pts',(0.0678620848486968,0.139969086193708,
1.42320954854869));
#16981=CARTESIAN_POINT('Ctrl Pts',(0.058643275810757,0.144373202007019,
1.42392472497687));
#16982=CARTESIAN_POINT('Ctrl Pts',(0.0498887458046868,0.147627306158739,
1.4245377567599));
#16983=CARTESIAN_POINT('Ctrl Pts',(0.0297618703397016,0.153111617344858,
1.42591082694151));
#16984=CARTESIAN_POINT('Ctrl Pts',(0.0183280937428587,0.154896642435418,
1.42666886063419));
#16985=CARTESIAN_POINT('Ctrl Pts',(0.00505766118145182,0.155477567507879,
1.42759196224716));
#16986=CARTESIAN_POINT('Ctrl Pts',(0.0033113983290382,0.155524558013418,
1.4277142075388));
#16987=CARTESIAN_POINT('Ctrl Pts',(0.000860382596904026,0.155549215554783,
1.42788703450928));
#16988=CARTESIAN_POINT('Ctrl Pts',(0.000155961494741628,0.155551516754159,
1.42793684903535));
#16989=CARTESIAN_POINT('Ctrl Pts',(-0.000982460733778573,0.155547502862334,
1.42801759793379));
#16990=CARTESIAN_POINT('Ctrl Pts',(-0.00141646848126894,0.155544156064679,
1.4280484394362));
#16991=CARTESIAN_POINT('Ctrl Pts',(-0.00232004107025522,0.155533406231651,
1.42811277090245));
#16992=CARTESIAN_POINT('Ctrl Pts',(-0.00278959708450549,0.15552569300214,
1.4281462702244));
#16993=CARTESIAN_POINT('Ctrl Pts',(-0.00389776182029502,0.155502469475048,
1.42822549479645));
#16994=CARTESIAN_POINT('Ctrl Pts',(-0.00453631989229349,0.155485151507581,
1.42827127599278));
#16995=CARTESIAN_POINT('Ctrl Pts',(-0.00664665160358494,0.155414907372182,
1.4284230157242));
#16996=CARTESIAN_POINT('Ctrl Pts',(-0.0081177398432963,0.155345014189401,
1.42852950075198));
#16997=CARTESIAN_POINT('Ctrl Pts',(-0.0158553046780688,0.154867188745633,
1.42909349985657));
#16998=CARTESIAN_POINT('Ctrl Pts',(-0.0220929626075653,0.154100999410571,
1.42956205014491));
#16999=CARTESIAN_POINT('Ctrl Pts',(-0.0380932836478177,0.151144192606857,
1.43079982974944));
#17000=CARTESIAN_POINT('Ctrl Pts',(-0.0477217951951853,0.14838554072075,
1.43158139264115));
#17001=CARTESIAN_POINT('Ctrl Pts',(-0.0592634140963715,0.143838361237585,
1.43253669426715));
#17002=CARTESIAN_POINT('Ctrl Pts',(-0.0614875180861261,0.142901743502157,
1.43272156478415));
#17003=CARTESIAN_POINT('Ctrl Pts',(-0.0636886279094242,0.141913921709658,
1.43290478746296));
#17004=CARTESIAN_POINT('Origin',(0.,0.,-0.129405622560373));
#17005=CARTESIAN_POINT('',(-0.063688625831373,0.141913922642253,1.51675072916146));
#17006=CARTESIAN_POINT('',(-0.0636886280167372,0.141913921661498,1.50282608545586));
#17007=CARTESIAN_POINT('',(-0.0636886258329924,0.141913922641526,-0.129405622560373));
#17008=CARTESIAN_POINT('Ctrl Pts',(-0.063688625831373,0.141913922642253,
1.51675072916146));
#17009=CARTESIAN_POINT('Ctrl Pts',(-0.0634115737974058,0.142038259021649,
1.5167292894899));
#17010=CARTESIAN_POINT('Ctrl Pts',(-0.0631341587634355,0.142161783591578,
1.51670782241692));
#17011=CARTESIAN_POINT('Ctrl Pts',(-0.0623721692403226,0.142498404291874,
1.51664885823609));
#17012=CARTESIAN_POINT('Ctrl Pts',(-0.0618868709325375,0.142709838185951,
1.51661130546527));
#17013=CARTESIAN_POINT('Ctrl Pts',(-0.0613978711293336,0.142919921386151,
1.51657346424412));
#17014=CARTESIAN_POINT('Ctrl Pts',(-0.0613952339921468,0.142921054261741,
1.51657326016936));
#17015=CARTESIAN_POINT('Ctrl Pts',(-0.0613898650871311,0.142923360488841,
1.51657284469672));
#17016=CARTESIAN_POINT('Ctrl Pts',(-0.0613871333164061,0.142924533835284,
1.51657263329862));
#17017=CARTESIAN_POINT('Ctrl Pts',(-0.0613815715135784,0.142926922544389,
1.51657220289832));
#17018=CARTESIAN_POINT('Ctrl Pts',(-0.0613787414796765,0.142928137901035,
1.51657198389599));
#17019=CARTESIAN_POINT('Ctrl Pts',(-0.0613729789905258,0.142930612396411,
1.5165715379653));
#17020=CARTESIAN_POINT('Ctrl Pts',(-0.0613700465316182,0.142931871529327,
1.51657131103664));
#17021=CARTESIAN_POINT('Ctrl Pts',(-0.0613640771852345,0.142934434417069,
1.51657084909799));
#17022=CARTESIAN_POINT('Ctrl Pts',(-0.0613610391530454,0.142935738655462,
1.51657061399939));
#17023=CARTESIAN_POINT('Ctrl Pts',(-0.0613548529131532,0.142938394197412,
1.51657013527607));
#17024=CARTESIAN_POINT('Ctrl Pts',(-0.0613517047882596,0.142939745456975,
1.51656989165776));
#17025=CARTESIAN_POINT('Ctrl Pts',(-0.0613452940898259,0.142942496849713,
1.51656939556433));
#17026=CARTESIAN_POINT('Ctrl Pts',(-0.0613420315920367,0.142943896941283,
1.51656914309507));
#17027=CARTESIAN_POINT('Ctrl Pts',(-0.0613353876915296,0.142946747882776,
1.51656862895485));
#17028=CARTESIAN_POINT('Ctrl Pts',(-0.0613320063588894,0.142948198692836,
1.51656836728932));
#17029=CARTESIAN_POINT('Ctrl Pts',(-0.0613251201388662,0.142951153036596,
1.51656783439673));
#17030=CARTESIAN_POINT('Ctrl Pts',(-0.0613216153178053,0.142952656531297,
1.51656756317479));
#17031=CARTESIAN_POINT('Ctrl Pts',(-0.0613144772768866,0.142955718290263,
1.5165670107945));
#17032=CARTESIAN_POINT('Ctrl Pts',(-0.0613108441172547,0.142957276517335,
1.5165667296408));
#17033=CARTESIAN_POINT('Ctrl Pts',(-0.0613034444908888,0.142960449811625,
1.51656615701712));
#17034=CARTESIAN_POINT('Ctrl Pts',(-0.0612996780825213,0.142962064841614,
1.51656586555166));
#17035=CARTESIAN_POINT('Ctrl Pts',(-0.060872511151842,0.143145213360316,
1.5165328090021));
#17036=CARTESIAN_POINT('Ctrl Pts',(-0.0604483110807719,0.143324863164073,
1.51649998039455));
#17037=CARTESIAN_POINT('Ctrl Pts',(-0.0594965426649963,0.143722962528017,
1.51642631646053));
#17038=CARTESIAN_POINT('Ctrl Pts',(-0.0589685592715691,0.143940395818116,
1.51638544730296));
#17039=CARTESIAN_POINT('Ctrl Pts',(-0.057626579403494,0.144484425098828,
1.51628155080268));
#17040=CARTESIAN_POINT('Ctrl Pts',(-0.0568110051460953,0.144807048811859,
1.5162183910559));
#17041=CARTESIAN_POINT('Ctrl Pts',(-0.0521255864926039,0.146614825505493,
1.51585539465859));
#17042=CARTESIAN_POINT('Ctrl Pts',(-0.0482006912242076,0.147951583835434,
1.51555067628713));
#17043=CARTESIAN_POINT('Ctrl Pts',(-0.042509196919865,0.149639509079444,
1.51510739441969));
#17044=CARTESIAN_POINT('Ctrl Pts',(-0.0407823437156287,0.150119334225748,
1.51497272744455));
#17045=CARTESIAN_POINT('Ctrl Pts',(-0.0247139380899117,0.154286410622172,
1.5137182616087));
#17046=CARTESIAN_POINT('Ctrl Pts',(-0.00992516384667007,0.155937452321803,
1.51254348940641));
#17047=CARTESIAN_POINT('Ctrl Pts',(0.00734259446272711,0.155396250235547,
1.51124529336215));
#17048=CARTESIAN_POINT('Ctrl Pts',(0.00981036872442895,0.155259997484279,
1.51106177617048));
#17049=CARTESIAN_POINT('Ctrl Pts',(0.012812769854591,0.15502234512544,1.51084175491769));
#17050=CARTESIAN_POINT('Ctrl Pts',(0.0133512950299314,0.154976893451499,
1.51080241890958));
#17051=CARTESIAN_POINT('Ctrl Pts',(0.0141892635572375,0.154901768324114,
1.51074142096896));
#17052=CARTESIAN_POINT('Ctrl Pts',(0.0144888689648992,0.154874031750151,
1.51071965385025));
#17053=CARTESIAN_POINT('Ctrl Pts',(0.0150450130498069,0.15482091762925,
1.51067932874813));
#17054=CARTESIAN_POINT('Ctrl Pts',(0.0153015665954479,0.154795771953959,
1.51066075846002));
#17055=CARTESIAN_POINT('Ctrl Pts',(0.0158820647205028,0.154737418093621,
1.51061881131201));
#17056=CARTESIAN_POINT('Ctrl Pts',(0.0162059676230002,0.154703830452683,
1.51059545599026));
#17057=CARTESIAN_POINT('Ctrl Pts',(0.0170411077525711,0.154614577587804,
1.51053536108826));
#17058=CARTESIAN_POINT('Ctrl Pts',(0.0175521842537917,0.154557393235694,
1.51049870471842));
#17059=CARTESIAN_POINT('Ctrl Pts',(0.0206659005822639,0.154193355475082,
1.51027605435428));
#17060=CARTESIAN_POINT('Ctrl Pts',(0.0232609259647238,0.153823281139247,
1.51009337955431));
#17061=CARTESIAN_POINT('Ctrl Pts',(0.0272206377575225,0.153156076940302,
1.5098173466242));
#17062=CARTESIAN_POINT('Ctrl Pts',(0.0285925822364789,0.152905891033015,
1.50972221037129));
#17063=CARTESIAN_POINT('Ctrl Pts',(0.0311635770627496,0.15240123302773,
1.50954455974723));
#17064=CARTESIAN_POINT('Ctrl Pts',(0.0323633303686801,0.152150975501402,
1.50946191991524));
#17065=CARTESIAN_POINT('Ctrl Pts',(0.0480581833920141,0.148683126255555,
1.50838281827206));
#17066=CARTESIAN_POINT('Ctrl Pts',(0.0620226148497372,0.143420657705692,
1.50743675080658));
#17067=CARTESIAN_POINT('Ctrl Pts',(0.0769223327153423,0.135216214616027,
1.50627177882863));
#17068=CARTESIAN_POINT('Ctrl Pts',(0.078792825861938,0.134134856789172,
1.50612262793406));
#17069=CARTESIAN_POINT('Ctrl Pts',(0.0815514984620614,0.132462415389452,
1.50589787941424));
#17070=CARTESIAN_POINT('Ctrl Pts',(0.0824571545102543,0.131900553313644,
1.50582330859723));
#17071=CARTESIAN_POINT('Ctrl Pts',(0.0841002150065367,0.130857675917978,
1.50568652643191));
#17072=CARTESIAN_POINT('Ctrl Pts',(0.0848394515442751,0.130379618481977,
1.505624424245));
#17073=CARTESIAN_POINT('Ctrl Pts',(0.086006519932023,0.129610757963195,
1.5055254631358));
#17074=CARTESIAN_POINT('Ctrl Pts',(0.0864370360673013,0.129324045848996,
1.50548875710056));
#17075=CARTESIAN_POINT('Ctrl Pts',(0.0872481022272445,0.128778038522164,
1.50541922032438));
#17076=CARTESIAN_POINT('Ctrl Pts',(0.0876289473621483,0.128519189709944,
1.50538640665426));
#17077=CARTESIAN_POINT('Ctrl Pts',(0.0884773378952887,0.127937040372345,
1.50531294296411));
#17078=CARTESIAN_POINT('Ctrl Pts',(0.0889442697050343,0.127612861777527,
1.5052722599394));
#17079=CARTESIAN_POINT('Ctrl Pts',(0.0901203194974467,0.12678677089015,
1.50516915018316));
#17080=CARTESIAN_POINT('Ctrl Pts',(0.0908270208172611,0.12628146931204,
1.50510659450564));
#17081=CARTESIAN_POINT('Ctrl Pts',(0.0947820210169453,0.123403214296666,
1.50475308683724));
#17082=CARTESIAN_POINT('Ctrl Pts',(0.0979412515675018,0.120911085206228,
1.50445754595618));
#17083=CARTESIAN_POINT('Ctrl Pts',(0.102756938693512,0.116799615877514,
1.50398519670993));
#17084=CARTESIAN_POINT('Ctrl Pts',(0.104480059052111,0.115260813196359,
1.50381146899885));
#17085=CARTESIAN_POINT('Ctrl Pts',(0.116815377746958,0.103741026462546,
1.50253303966394));
#17086=CARTESIAN_POINT('Ctrl Pts',(0.126011599839395,0.0923528403500003,
1.50137757784007));
#17087=CARTESIAN_POINT('Ctrl Pts',(0.134700107778986,0.0778283231196782,
1.50010748544427));
#17088=CARTESIAN_POINT('Ctrl Pts',(0.135864952580801,0.0757765347766056,
1.4999324793348));
#17089=CARTESIAN_POINT('Ctrl Pts',(0.137231126208496,0.0732372535132789,
1.49972191510898));
#17090=CARTESIAN_POINT('Ctrl Pts',(0.137477167097544,0.0727743488516348,
1.4996837701762));
#17091=CARTESIAN_POINT('Ctrl Pts',(0.137859088665095,0.0720469470532173,
1.49962421576684));
#17092=CARTESIAN_POINT('Ctrl Pts',(0.137996555991879,0.071783295032284,
1.49960270886281));
#17093=CARTESIAN_POINT('Ctrl Pts',(0.13825198666125,0.0712899526891006,
1.49956261508574));
#17094=CARTESIAN_POINT('Ctrl Pts',(0.138370132754727,0.0710603654174914,
1.49954401719314));
#17095=CARTESIAN_POINT('Ctrl Pts',(0.138638281864521,0.0705360804446323,
1.49950168389232));
#17096=CARTESIAN_POINT('Ctrl Pts',(0.138787917007515,0.0702411983173544,
1.4994779716832));
#17097=CARTESIAN_POINT('Ctrl Pts',(0.139244078401547,0.0693351041010873,
1.49940540356294));
#17098=CARTESIAN_POINT('Ctrl Pts',(0.139547521508513,0.0687223349244418,
1.49935673548462));
#17099=CARTESIAN_POINT('Ctrl Pts',(0.143851463827285,0.0598849459786123,
1.49866039822767));
#17100=CARTESIAN_POINT('Ctrl Pts',(0.147123742185742,0.0513236201721397,
1.49805421826056));
#17101=CARTESIAN_POINT('Ctrl Pts',(0.152221494482901,0.0333862455787411,
1.49682522297701));
#17102=CARTESIAN_POINT('Ctrl Pts',(0.153975621809865,0.0240315752144556,
1.49620463236699));
#17103=CARTESIAN_POINT('Ctrl Pts',(0.155275615618776,0.0102192199852124,
1.4952629482169));
#17104=CARTESIAN_POINT('Ctrl Pts',(0.155501596065599,0.00584780215777957,
1.4949615235644));
#17105=CARTESIAN_POINT('Ctrl Pts',(0.155551952662081,0.00053031875706886,
1.49458806859122));
#17106=CARTESIAN_POINT('Ctrl Pts',(0.155552309763188,-0.000412398471685439,
1.49452160438454));
#17107=CARTESIAN_POINT('Ctrl Pts',(0.155539441981686,-0.00188947944462984,
1.49441704025413));
#17108=CARTESIAN_POINT('Ctrl Pts',(0.155532031826787,-0.00242388271454619,
1.49437912196931));
#17109=CARTESIAN_POINT('Ctrl Pts',(0.155513998882076,-0.00337192128196993,
1.49431169489536));
#17110=CARTESIAN_POINT('Ctrl Pts',(0.155504479421026,-0.00378557463955963,
1.4942822208522));
#17111=CARTESIAN_POINT('Ctrl Pts',(0.155478724166731,-0.00473927711242047,
1.49421413984222));
#17112=CARTESIAN_POINT('Ctrl Pts',(0.155461324882002,-0.00527928673103993,
1.49417549689011));
#17113=CARTESIAN_POINT('Ctrl Pts',(0.155405818573014,-0.00676196123561041,
1.49406913316351));
#17114=CARTESIAN_POINT('Ctrl Pts',(0.155361948755169,-0.00770437357741231,
1.49400123341052));
#17115=CARTESIAN_POINT('Ctrl Pts',(0.155093148164175,-0.0125327096170083,
1.49365180088238));
#17116=CARTESIAN_POINT('Ctrl Pts',(0.154731006502274,-0.016409266671623,
1.49336602700572));
#17117=CARTESIAN_POINT('Ctrl Pts',(0.153960853381503,-0.0222695801432221,
1.49292558228463));
#17118=CARTESIAN_POINT('Ctrl Pts',(0.153658855175888,-0.0242659055892493,
1.49277405386945));
#17119=CARTESIAN_POINT('Ctrl Pts',(0.150845569777699,-0.0406938567296243,
1.49151498647515));
#17120=CARTESIAN_POINT('Ctrl Pts',(0.146346575403846,-0.0547081111284029,
1.49035373953866));
#17121=CARTESIAN_POINT('Ctrl Pts',(0.13878414728827,-0.0702990705423108,
1.48904900247372));
#17122=CARTESIAN_POINT('Ctrl Pts',(0.137551059375049,-0.0726822349840366,
1.4888494766122));
#17123=CARTESIAN_POINT('Ctrl Pts',(0.13599410496507,-0.0755096192129182,
1.48861365684526));
#17124=CARTESIAN_POINT('Ctrl Pts',(0.135728857481408,-0.0759853699706729,
1.48857400795639));
#17125=CARTESIAN_POINT('Ctrl Pts',(0.135312758419945,-0.0767225585972718,
1.48851263125344));
#17126=CARTESIAN_POINT('Ctrl Pts',(0.135163639337301,-0.0769849608316749,
1.48849079617333));
#17127=CARTESIAN_POINT('Ctrl Pts',(0.134885781319639,-0.0774706067249488,
1.48845040900936));
#17128=CARTESIAN_POINT('Ctrl Pts',(0.134757252569568,-0.0776939623804312,
1.48843184428833));
#17129=CARTESIAN_POINT('Ctrl Pts',(0.134465669142637,-0.0781977720815382,
1.48838999051033));
#17130=CARTESIAN_POINT('Ctrl Pts',(0.134302292186977,-0.0784780354941646,
1.48836672258367));
#17131=CARTESIAN_POINT('Ctrl Pts',(0.133818280215661,-0.0793023909855428,
1.4882983207155));
#17132=CARTESIAN_POINT('Ctrl Pts',(0.133495201828687,-0.0798450528280568,
1.4882533409902));
#17133=CARTESIAN_POINT('Ctrl Pts',(0.13116444263278,-0.0837062405859229,
1.48793353066938));
#17134=CARTESIAN_POINT('Ctrl Pts',(0.129036355577877,-0.0869509694362822,
1.48766600553238));
#17135=CARTESIAN_POINT('Ctrl Pts',(0.119613596422089,-0.100208778496501,
1.48656292868547));
#17136=CARTESIAN_POINT('Ctrl Pts',(0.111257771295966,-0.109411914234389,
1.48576902397183));
#17137=CARTESIAN_POINT('Ctrl Pts',(0.0985606166172678,-0.120420595091738,
1.48464549146989));
#17138=CARTESIAN_POINT('Ctrl Pts',(0.0951016149729839,-0.123170583067822,
1.48434675531116));
#17139=CARTESIAN_POINT('Ctrl Pts',(0.0893674766942415,-0.127343681998074,
1.4838583572797));
#17140=CARTESIAN_POINT('Ctrl Pts',(0.0871643172428911,-0.128861707025169,
1.48367223611274));
#17141=CARTESIAN_POINT('Ctrl Pts',(0.0842500556813007,-0.130760759396556,
1.48342741238877));
#17142=CARTESIAN_POINT('Ctrl Pts',(0.083573511007153,-0.131194193067917,
1.48337067111942));
#17143=CARTESIAN_POINT('Ctrl Pts',(0.0824674293604693,-0.131890785544996,
1.4832780421304));
#17144=CARTESIAN_POINT('Ctrl Pts',(0.0820399120696445,-0.132157137657141,
1.48324227263292));
#17145=CARTESIAN_POINT('Ctrl Pts',(0.081215067482475,-0.132665488135432,
1.48317331874972));
#17146=CARTESIAN_POINT('Ctrl Pts',(0.0808179327809818,-0.132907790068002,
1.48314014595945));
#17147=CARTESIAN_POINT('Ctrl Pts',(0.0799058888868548,-0.133458651874716,
1.48306401884765));
#17148=CARTESIAN_POINT('Ctrl Pts',(0.079390271329594,-0.13376601825027,
1.48302102166397));
#17149=CARTESIAN_POINT('Ctrl Pts',(0.0780153002244631,-0.134574906415282,
1.48290646315729));
#17150=CARTESIAN_POINT('Ctrl Pts',(0.0771529042156,-0.135071173058272,1.48283471366319));
#17151=CARTESIAN_POINT('Ctrl Pts',(0.0706168988435978,-0.138749306670897,
1.4822916159683));
#17152=CARTESIAN_POINT('Ctrl Pts',(0.0647542977002466,-0.141580277692862,
1.48180791387295));
#17153=CARTESIAN_POINT('Ctrl Pts',(0.0490378072537463,-0.147988884587285,
1.48051921234261));
#17154=CARTESIAN_POINT('Ctrl Pts',(0.038969174287163,-0.150952929635953,
1.47969982599384));
#17155=CARTESIAN_POINT('Ctrl Pts',(0.0247427598898267,-0.153621776764717,
1.47858580191837));
#17156=CARTESIAN_POINT('Ctrl Pts',(0.0207775636243955,-0.154208146445459,
1.47828016280414));
#17157=CARTESIAN_POINT('Ctrl Pts',(0.014739926060913,-0.154863828791347,
1.47782590921319));
#17158=CARTESIAN_POINT('Ctrl Pts',(0.0126816152154906,-0.155045956596636,
1.47767299937988));
#17159=CARTESIAN_POINT('Ctrl Pts',(0.0101186113198169,-0.15522135461602,
1.47748549914493));
#17160=CARTESIAN_POINT('Ctrl Pts',(0.00961689504560676,-0.155253246576093,
1.47744893346168));
#17161=CARTESIAN_POINT('Ctrl Pts',(0.00882294108970852,-0.155299851309404,
1.47739129666488));
#17162=CARTESIAN_POINT('Ctrl Pts',(0.00853080739872957,-0.155316172484348,
1.47737013802526));
#17163=CARTESIAN_POINT('Ctrl Pts',(0.00797996845085937,-0.155345388394753,
1.47733033585618));
#17164=CARTESIAN_POINT('Ctrl Pts',(0.00772128030091277,-0.155358461063024,
1.47731168306248));
#17165=CARTESIAN_POINT('Ctrl Pts',(0.00713025432043404,-0.155386848386901,
1.47726915525496));
#17166=CARTESIAN_POINT('Ctrl Pts',(0.00679789938511911,-0.155401743065625,
1.47724530391799));
#17167=CARTESIAN_POINT('Ctrl Pts',(0.00591652592644753,-0.155438409376836,
1.47718221483092));
#17168=CARTESIAN_POINT('Ctrl Pts',(0.00536742875672291,-0.155458338860321,
1.47714307722409));
#17169=CARTESIAN_POINT('Ctrl Pts',(0.00156140291275468,-0.155576288708972,
1.47687288263785));
#17170=CARTESIAN_POINT('Ctrl Pts',(-0.00169809842502759,-0.155574869554208,
1.47664698689106));
#17171=CARTESIAN_POINT('Ctrl Pts',(-0.016995090789953,-0.155087297234471,
1.47560251408687));
#17172=CARTESIAN_POINT('Ctrl Pts',(-0.0289503915960709,-0.153306339930389,
1.47482903575262));
#17173=CARTESIAN_POINT('Ctrl Pts',(-0.0454927493567403,-0.148835805218277,
1.47368908609705));
#17174=CARTESIAN_POINT('Ctrl Pts',(-0.0503357744107182,-0.147268427433021,
1.47334680726373));
#17175=CARTESIAN_POINT('Ctrl Pts',(-0.0578569305323005,-0.144419919534064,
1.47279438291488));
#17176=CARTESIAN_POINT('Ctrl Pts',(-0.0605902921229622,-0.143294633785485,
1.47258911397594));
#17177=CARTESIAN_POINT('Ctrl Pts',(-0.0640498721877315,-0.141753690268276,
1.47232268022847));
#17178=CARTESIAN_POINT('Ctrl Pts',(-0.0648072068765667,-0.141409054591942,
1.47226394151801));
#17179=CARTESIAN_POINT('Ctrl Pts',(-0.0660242433682394,-0.140843395021498,
1.4721688611638));
#17180=CARTESIAN_POINT('Ctrl Pts',(-0.0664856944397882,-0.140626153531635,
1.47213264985675));
#17181=CARTESIAN_POINT('Ctrl Pts',(-0.06736435848372,-0.140207205428986,
1.47206338710323));
#17182=CARTESIAN_POINT('Ctrl Pts',(-0.0677817556138718,-0.140005895752607,
1.47203034968942));
#17183=CARTESIAN_POINT('Ctrl Pts',(-0.0687350800936344,-0.139540847206908,
1.47195457964884));
#17184=CARTESIAN_POINT('Ctrl Pts',(-0.0692703974540884,-0.139275881949594,
1.47191180472571));
#17185=CARTESIAN_POINT('Ctrl Pts',(-0.070664977048832,-0.138575579961187,
1.47179976469628));
#17186=CARTESIAN_POINT('Ctrl Pts',(-0.0715217332533905,-0.138135339206531,
1.47173032896428));
#17187=CARTESIAN_POINT('Ctrl Pts',(-0.0774278834447004,-0.135030811581515,
1.47124738770725));
#17188=CARTESIAN_POINT('Ctrl Pts',(-0.0823306923332227,-0.132098595536396,
1.47082444168715));
#17189=CARTESIAN_POINT('Ctrl Pts',(-0.0991899908242285,-0.120711951329825,
1.46928763740646));
#17190=CARTESIAN_POINT('Ctrl Pts',(-0.11010048399853,-0.11085050504113,
1.4681273943134));
#17191=CARTESIAN_POINT('Ctrl Pts',(-0.121199325080069,-0.0975387340276034,
1.46682219980044));
#17192=CARTESIAN_POINT('Ctrl Pts',(-0.122872931636337,-0.0954218324286447,
1.46662151448217));
#17193=CARTESIAN_POINT('Ctrl Pts',(-0.124817856587308,-0.0928256582437247,
1.46638450832105));
#17194=CARTESIAN_POINT('Ctrl Pts',(-0.125142670933285,-0.0923872939699318,
1.46634479387056));
#17195=CARTESIAN_POINT('Ctrl Pts',(-0.125643695949999,-0.0917036279220294,
1.46628333782497));
#17196=CARTESIAN_POINT('Ctrl Pts',(-0.125821505572221,-0.091459512604308,
1.46626148852585));
#17197=CARTESIAN_POINT('Ctrl Pts',(-0.126149710211356,-0.0910061509644667,
1.46622108829661));
#17198=CARTESIAN_POINT('Ctrl Pts',(-0.126300294845668,-0.0907970507429409,
1.46620252465993));
#17199=CARTESIAN_POINT('Ctrl Pts',(-0.12663913666572,-0.0903240645472233,
1.46616069005108));
#17200=CARTESIAN_POINT('Ctrl Pts',(-0.126827088619721,-0.0900599642971817,
1.46613744012514));
#17201=CARTESIAN_POINT('Ctrl Pts',(-0.127378104741062,-0.0892805593620771,
1.46606914007957));
#17202=CARTESIAN_POINT('Ctrl Pts',(-0.127738869693975,-0.0887636246050923,
1.46602424349131));
#17203=CARTESIAN_POINT('Ctrl Pts',(-0.130279831990909,-0.085075141410753,
1.46570663186922));
#17204=CARTESIAN_POINT('Ctrl Pts',(-0.132345033404127,-0.0818255017189523,
1.46544110840641));
#17205=CARTESIAN_POINT('Ctrl Pts',(-0.140580248884761,-0.0677381545590202,
1.4643341473842));
#17206=CARTESIAN_POINT('Ctrl Pts',(-0.145556096661793,-0.0562559756689722,
1.46353523306249));
#17207=CARTESIAN_POINT('Ctrl Pts',(-0.15081424120074,-0.038558615019287,
1.4623005878519));
#17208=CARTESIAN_POINT('Ctrl Pts',(-0.152187254146884,-0.032721983969422,
1.46189353868082));
#17209=CARTESIAN_POINT('Ctrl Pts',(-0.153467820857172,-0.0254065550269558,
1.46137537860276));
#17210=CARTESIAN_POINT('Ctrl Pts',(-0.153695845333057,-0.0239885798235002,
1.46127459126849));
#17211=CARTESIAN_POINT('Ctrl Pts',(-0.153995958444428,-0.021941907579324,
1.46112852548002));
#17212=CARTESIAN_POINT('Ctrl Pts',(-0.154083901223177,-0.0213155785265165,
1.46108374660701));
#17213=CARTESIAN_POINT('Ctrl Pts',(-0.154230354402046,-0.0202242410176655,
1.46100557647946));
#17214=CARTESIAN_POINT('Ctrl Pts',(-0.154290587972173,-0.0197594685689641,
1.46097223988432));
#17215=CARTESIAN_POINT('Ctrl Pts',(-0.154402771545967,-0.0188620393145703,
1.46090777839004));
#17216=CARTESIAN_POINT('Ctrl Pts',(-0.154455005714666,-0.0184294218775842,
1.46087666276279));
#17217=CARTESIAN_POINT('Ctrl Pts',(-0.154587937220006,-0.0172881705170024,
1.46079446762885));
#17218=CARTESIAN_POINT('Ctrl Pts',(-0.154665578990884,-0.0165791983449027,
1.46074329267338));
#17219=CARTESIAN_POINT('Ctrl Pts',(-0.154921716261145,-0.0140817228979077,
1.46056260428469));
#17220=CARTESIAN_POINT('Ctrl Pts',(-0.155074079500373,-0.0122907466228192,
1.46043227807444));
#17221=CARTESIAN_POINT('Ctrl Pts',(-0.155223278801377,-0.010085000523286,
1.46027077696939));
#17222=CARTESIAN_POINT('Ctrl Pts',(-0.155249541780747,-0.00967229487752725,
1.46024051678374));
#17223=CARTESIAN_POINT('Ctrl Pts',(-0.155361757049497,-0.00779053619728491,
1.46010234740602));
#17224=CARTESIAN_POINT('Ctrl Pts',(-0.155428503039985,-0.00632045743794215,
1.45999386036422));
#17225=CARTESIAN_POINT('Ctrl Pts',(-0.155525890911946,-0.00319834126535703,
1.45976227499357));
#17226=CARTESIAN_POINT('Ctrl Pts',(-0.155551086954946,-0.00154632552727123,
1.4596390326755));
#17227=CARTESIAN_POINT('Ctrl Pts',(-0.155542083644713,0.0116999912811569,
1.45864523099621));
#17228=CARTESIAN_POINT('Ctrl Pts',(-0.154237875836441,0.0232559469567256,
1.45773979922087));
#17229=CARTESIAN_POINT('Ctrl Pts',(-0.150213724972465,0.040916709570916,
1.45634155928028));
#17230=CARTESIAN_POINT('Ctrl Pts',(-0.148366021733034,0.0471793087978687,
1.45584369951952));
#17231=CARTESIAN_POINT('Ctrl Pts',(-0.145890113147153,0.0539663629180312,
1.45531407205644));
#17232=CARTESIAN_POINT('Ctrl Pts',(-0.145645536924261,0.0546229902568069,
1.45526294065231));
#17233=CARTESIAN_POINT('Ctrl Pts',(-0.145277840313227,0.0555901354045607,
1.455187812813));
#17234=CARTESIAN_POINT('Ctrl Pts',(-0.145158148106829,0.0559019327416983,
1.45516362070176));
#17235=CARTESIAN_POINT('Ctrl Pts',(-0.144944021864038,0.0564544051812521,
1.45512080809518));
#17236=CARTESIAN_POINT('Ctrl Pts',(-0.144849991295519,0.0566952322871937,
1.45510216390611));
#17237=CARTESIAN_POINT('Ctrl Pts',(-0.144647309738644,0.0572105359484672,
1.45506231005985));
#17238=CARTESIAN_POINT('Ctrl Pts',(-0.144538477997265,0.0574849373343044,
1.45504111147077));
#17239=CARTESIAN_POINT('Ctrl Pts',(-0.144237821837179,0.0582367406029928,
1.4549830924919));
#17240=CARTESIAN_POINT('Ctrl Pts',(-0.144044406595513,0.0587135091183309,
1.45494636619012));
#17241=CARTESIAN_POINT('Ctrl Pts',(-0.143003457963293,0.0612433411001956,
1.45475180234469));
#17242=CARTESIAN_POINT('Ctrl Pts',(-0.142114333570494,0.0632791702539503,
1.45459633170291));
#17243=CARTESIAN_POINT('Ctrl Pts',(-0.135277085610954,0.0780626828194668,
1.45347045437207));
#17244=CARTESIAN_POINT('Ctrl Pts',(-0.127667147193817,0.0899715609165035,
1.45257557106974));
#17245=CARTESIAN_POINT('Ctrl Pts',(-0.11419699211101,0.105831201253436,
1.45118584178815));
#17246=CARTESIAN_POINT('Ctrl Pts',(-0.109506996859866,0.110676982970521,
1.45072806844399));
#17247=CARTESIAN_POINT('Ctrl Pts',(-0.103777032265685,0.115875499728354,
1.4501860377342));
#17248=CARTESIAN_POINT('Ctrl Pts',(-0.103029454382375,0.116540702374766,
1.45011564141425));
#17249=CARTESIAN_POINT('Ctrl Pts',(-0.101821985733292,0.117594421930672,
1.45000241749149));
#17250=CARTESIAN_POINT('Ctrl Pts',(-0.101366158168923,0.117987570563655,
1.44995978193925));
#17251=CARTESIAN_POINT('Ctrl Pts',(-0.100553828062199,0.118680018648249,
1.4498839835271));
#17252=CARTESIAN_POINT('Ctrl Pts',(-0.100198240235437,0.118980384137098,
1.44985086488177));
#17253=CARTESIAN_POINT('Ctrl Pts',(-0.0994556460677442,0.119601964515796,
1.44978182480859));
#17254=CARTESIAN_POINT('Ctrl Pts',(-0.0990684198671205,0.119922907006395,
1.44974589284215));
#17255=CARTESIAN_POINT('Ctrl Pts',(-0.0980612124555313,0.120749497582212,
1.4496526040471));
#17256=CARTESIAN_POINT('Ctrl Pts',(-0.0974388813301696,0.121252244990941,
1.44959513143233));
#17257=CARTESIAN_POINT('Ctrl Pts',(-0.0947438296693985,0.123395283276602,
1.44934693393863));
#17258=CARTESIAN_POINT('Ctrl Pts',(-0.0926334784519948,0.124987304443538,
1.44915431749672));
#17259=CARTESIAN_POINT('Ctrl Pts',(-0.0869504457183114,0.12905150589219,
1.44863971489913));
#17260=CARTESIAN_POINT('Ctrl Pts',(-0.0833132171826555,0.131428964260243,
1.44831442098161));
#17261=CARTESIAN_POINT('Ctrl Pts',(-0.0744421641491966,0.136711174792291,
1.44753079664743));
#17262=CARTESIAN_POINT('Ctrl Pts',(-0.0691354132859616,0.13946949740905,
1.44706948227971));
#17263=CARTESIAN_POINT('Ctrl Pts',(-0.0636885593981421,0.141913952456372,
1.4466066640002));
#17264=CARTESIAN_POINT('',(-0.155550023928855,6.62725240224652E-5,1.44572602062627));
#17265=CARTESIAN_POINT('Ctrl Pts',(-0.0636886279094242,0.141913921709658,
1.43290478746296));
#17266=CARTESIAN_POINT('Ctrl Pts',(-0.0668602430864753,0.140490553117982,
1.43316879602027));
#17267=CARTESIAN_POINT('Ctrl Pts',(-0.0699841163588671,0.138960872955427,
1.43342939107116));
#17268=CARTESIAN_POINT('Ctrl Pts',(-0.0736672353627304,0.137001540179662,
1.43373518284804));
#17269=CARTESIAN_POINT('Ctrl Pts',(-0.0742774077252028,0.136671688098216,
1.43378579276417));
#17270=CARTESIAN_POINT('Ctrl Pts',(-0.0751768316905237,0.136177667246265,
1.43386029807908));
#17271=CARTESIAN_POINT('Ctrl Pts',(-0.0754677845091119,0.136016640844285,
1.43388438465061));
#17272=CARTESIAN_POINT('Ctrl Pts',(-0.0759774083613463,0.13573245338047,
1.43392654462472));
#17273=CARTESIAN_POINT('Ctrl Pts',(-0.0761962995396099,0.135609695162602,
1.43394464331935));
#17274=CARTESIAN_POINT('Ctrl Pts',(-0.0764155917042016,0.135486013466821,
1.43396276517435));
#17275=CARTESIAN_POINT('Ctrl Pts',(-0.0764162857534264,0.13548562201319,
1.43396282252904));
#17276=CARTESIAN_POINT('Ctrl Pts',(-0.0764176762548998,0.135484837736335,
1.43396293743684));
#17277=CARTESIAN_POINT('Ctrl Pts',(-0.0764183686206453,0.135484447218061,
1.43396299465224));
#17278=CARTESIAN_POINT('Ctrl Pts',(-0.0764197434379997,0.135483671759706,
1.43396310826356));
#17279=CARTESIAN_POINT('Ctrl Pts',(-0.0764204300266164,0.135483284486199,
1.43396316500135));
#17280=CARTESIAN_POINT('Ctrl Pts',(-0.0764217988286091,0.135482512393346,
1.43396327811519));
#17281=CARTESIAN_POINT('Ctrl Pts',(-0.0764224810472205,0.135482127571133,
1.43396333449167));
#17282=CARTESIAN_POINT('Ctrl Pts',(-0.076423841161059,0.135481360351876,
1.43396344688716));
#17283=CARTESIAN_POINT('Ctrl Pts',(-0.0764245190480729,0.135480977959552,
1.4339635029055));
#17284=CARTESIAN_POINT('Ctrl Pts',(-0.0764258705221563,0.135480215587106,
1.43396361458666));
#17285=CARTESIAN_POINT('Ctrl Pts',(-0.0764265441094105,0.135479835606966,
1.4339636702495));
#17286=CARTESIAN_POINT('Ctrl Pts',(-0.0764278869939382,0.135479078053522,
1.43396378122048));
#17287=CARTESIAN_POINT('Ctrl Pts',(-0.0764285563026247,0.135478700473864,
1.43396383652957));
#17288=CARTESIAN_POINT('Ctrl Pts',(-0.076429890685956,0.13547794769008,
1.43396394679769));
#17289=CARTESIAN_POINT('Ctrl Pts',(-0.0764305557548401,0.135477572489285,
1.43396400175623));
#17290=CARTESIAN_POINT('Ctrl Pts',(-0.0764318816780812,0.135476824452463,
1.43396411132488));
#17291=CARTESIAN_POINT('Ctrl Pts',(-0.0764325425344626,0.135476451615376,
1.43396416593515));
#17292=CARTESIAN_POINT('Ctrl Pts',(-0.0764338600625909,0.135475708289349,
1.4339642748097));
#17293=CARTESIAN_POINT('Ctrl Pts',(-0.0764345167354105,0.135475337799884,
1.43396432907408));
#17294=CARTESIAN_POINT('Ctrl Pts',(-0.076686958807072,0.135332909616235,
1.43398518967622));
#17295=CARTESIAN_POINT('Ctrl Pts',(-0.0769383504848944,0.135190148696767,
1.43400595061829));
#17296=CARTESIAN_POINT('Ctrl Pts',(-0.077622914201455,0.134798869008774,
1.43406245367472));
#17297=CARTESIAN_POINT('Ctrl Pts',(-0.0780552949481778,0.134548960769233,
1.43409810790209));
#17298=CARTESIAN_POINT('Ctrl Pts',(-0.0790162257184926,0.133987369047628,
1.43417728809716));
#17299=CARTESIAN_POINT('Ctrl Pts',(-0.0795441536008456,0.133674629795657,
1.43422074941251));
#17300=CARTESIAN_POINT('Ctrl Pts',(-0.0811578847840455,0.13270572594395,
1.43435352128418));
#17301=CARTESIAN_POINT('Ctrl Pts',(-0.0822375542790302,0.132039376247014,
1.43444224421883));
#17302=CARTESIAN_POINT('Ctrl Pts',(-0.0863188856540324,0.129450978327353,
1.43477770445624));
#17303=CARTESIAN_POINT('Ctrl Pts',(-0.0892625256301097,0.127439049537694,
1.43501981488321));
#17304=CARTESIAN_POINT('Ctrl Pts',(-0.103965632118176,0.116630052961153,
1.43624418362759));
#17305=CARTESIAN_POINT('Ctrl Pts',(-0.114505203178463,0.106301487881652,
1.43718053136615));
#17306=CARTESIAN_POINT('Ctrl Pts',(-0.124394528177384,0.0934037576710502,
1.43829306053358));
#17307=CARTESIAN_POINT('Ctrl Pts',(-0.12532961566483,0.0921452535014083,
1.43840100210623));
#17308=CARTESIAN_POINT('Ctrl Pts',(-0.126512023532436,0.0905025886058208,
1.43854124387494));
#17309=CARTESIAN_POINT('Ctrl Pts',(-0.126776919984283,0.0901311444205592,
1.43857291352931));
#17310=CARTESIAN_POINT('Ctrl Pts',(-0.128009439705179,0.0883866918441236,
1.43872146083014));
#17311=CARTESIAN_POINT('Ctrl Pts',(-0.128956384159158,0.0869992790175068,
1.43883906885174));
#17312=CARTESIAN_POINT('Ctrl Pts',(-0.130262094986369,0.0850180546590946,
1.43900640773484));
#17313=CARTESIAN_POINT('Ctrl Pts',(-0.130639666580749,0.0844367248055172,
1.43905543577075));
#17314=CARTESIAN_POINT('Ctrl Pts',(-0.131246189784394,0.0834890816321818,
1.4391352505341));
#17315=CARTESIAN_POINT('Ctrl Pts',(-0.131477526430731,0.083124299224057,
1.43916594857187));
#17316=CARTESIAN_POINT('Ctrl Pts',(-0.131958058826364,0.0823595488234174,
1.43923025511968));
#17317=CARTESIAN_POINT('Ctrl Pts',(-0.132206961996207,0.0819594031357007,
1.43926387398682));
#17318=CARTESIAN_POINT('Ctrl Pts',(-0.132793794704565,0.0810063607224184,
1.43934388116802));
#17319=CARTESIAN_POINT('Ctrl Pts',(-0.133130092845252,0.0804524750707311,
1.43939032851898));
#17320=CARTESIAN_POINT('Ctrl Pts',(-0.13424671203123,0.0785872215250863,
1.43954658591223));
#17321=CARTESIAN_POINT('Ctrl Pts',(-0.135011172449007,0.0772665133395266,
1.43965696656311));
#17322=CARTESIAN_POINT('Ctrl Pts',(-0.139031529309008,0.0700789303461437,
1.44025650117011));
#17323=CARTESIAN_POINT('Ctrl Pts',(-0.141924196325721,0.0640181319700254,
1.44075830936803));
#17324=CARTESIAN_POINT('Ctrl Pts',(-0.149173224157554,0.0459030258503039,
1.44224662345396));
#17325=CARTESIAN_POINT('Ctrl Pts',(-0.152443922324118,0.0334748473956542,
1.44325749513671));
#17326=CARTESIAN_POINT('Ctrl Pts',(-0.154402401088823,0.0189508145755707,
1.44436240359479));
#17327=CARTESIAN_POINT('Ctrl Pts',(-0.154617171674818,0.0171103998377668,
1.44450093548808));
#17328=CARTESIAN_POINT('Ctrl Pts',(-0.154916380755177,0.014076482955724,
1.44472643444083));
#17329=CARTESIAN_POINT('Ctrl Pts',(-0.155020019995029,0.0128851090380782,
1.4448142589062));
#17330=CARTESIAN_POINT('Ctrl Pts',(-0.155142071079203,0.0112660237619248,
1.44493252516681));
#17331=CARTESIAN_POINT('Ctrl Pts',(-0.155172468910344,0.0108392995238594,
1.44496359283506));
#17332=CARTESIAN_POINT('Ctrl Pts',(-0.155217733881369,0.0101646096483685,
1.4450125461272));
#17333=CARTESIAN_POINT('Ctrl Pts',(-0.155233767880125,0.00991672893084847,
1.44503049582247));
#17334=CARTESIAN_POINT('Ctrl Pts',(-0.155264598648404,0.00942168837145768,
1.44506627029735));
#17335=CARTESIAN_POINT('Ctrl Pts',(-0.155279398888671,0.00917453470046273,
1.44508409464911));
#17336=CARTESIAN_POINT('Ctrl Pts',(-0.15530832920788,0.00867128370831169,
1.44512031583044));
#17337=CARTESIAN_POINT('Ctrl Pts',(-0.155322416004253,0.00841518696559419,
1.44513871007935));
#17338=CARTESIAN_POINT('Ctrl Pts',(-0.155353676275033,0.00782003937749486,
1.44518137060307));
#17339=CARTESIAN_POINT('Ctrl Pts',(-0.155370373447767,0.00748096307339606,
1.4452056108182));
#17340=CARTESIAN_POINT('Ctrl Pts',(-0.155426861121103,0.00625195164849051,
1.44529324507949));
#17341=CARTESIAN_POINT('Ctrl Pts',(-0.155460117764408,0.00536171048518981,
1.44535629318325));
#17342=CARTESIAN_POINT('Ctrl Pts',(-0.155527938024698,0.00300326776435513,
1.44552230000122));
#17343=CARTESIAN_POINT('Ctrl Pts',(-0.155549361931428,0.00153474931081583,
1.44562461906036));
#17344=CARTESIAN_POINT('Ctrl Pts',(-0.155549985958724,6.60926688657478E-5,
1.44572609898142));
#17345=CARTESIAN_POINT('Ctrl Pts',(-0.155549985880275,6.62770408882546E-5,
1.44572608624184));
#17346=CARTESIAN_POINT('Ctrl Pts',(-0.155555884261965,-0.0137770264064439,
1.44668261909254));
#17347=CARTESIAN_POINT('Ctrl Pts',(-0.153713842315672,-0.0275617844757425,
1.44756441268068));
#17348=CARTESIAN_POINT('Ctrl Pts',(-0.148397421963137,-0.0470578811843007,
1.44891276289187));
#17349=CARTESIAN_POINT('Ctrl Pts',(-0.146350050898578,-0.0530837628227759,
1.44934377173934));
#17350=CARTESIAN_POINT('Ctrl Pts',(-0.143377844087416,-0.060338998466371,
1.44989049754077));
#17351=CARTESIAN_POINT('Ctrl Pts',(-0.142796199559207,-0.0617028851532562,
1.44999451141723));
#17352=CARTESIAN_POINT('Ctrl Pts',(-0.141935498362046,-0.0636437513946578,
1.45014440564446));
#17353=CARTESIAN_POINT('Ctrl Pts',(-0.141672221417332,-0.0642276766150209,
1.45018974871774));
#17354=CARTESIAN_POINT('Ctrl Pts',(-0.141209554897716,-0.0652371438245133,
1.45026857212844));
#17355=CARTESIAN_POINT('Ctrl Pts',(-0.141011827971094,-0.0656634425854908,
1.45030199507685));
#17356=CARTESIAN_POINT('Ctrl Pts',(-0.140627943276303,-0.0664813665042139,
1.45036638728402));
#17357=CARTESIAN_POINT('Ctrl Pts',(-0.140442073405624,-0.0668731226495726,
1.45039734635409));
#17358=CARTESIAN_POINT('Ctrl Pts',(-0.139950906342907,-0.0678972712266717,
1.45047859273995));
#17359=CARTESIAN_POINT('Ctrl Pts',(-0.139642963495729,-0.0685283761837179,
1.45052897140022));
#17360=CARTESIAN_POINT('Ctrl Pts',(-0.138559903887194,-0.0707104072854445,
1.45070425874791));
#17361=CARTESIAN_POINT('Ctrl Pts',(-0.137763163170063,-0.0722503915897387,
1.45082991799839));
#17362=CARTESIAN_POINT('Ctrl Pts',(-0.131276622364889,-0.0842904099810718,
1.45182826473611));
#17363=CARTESIAN_POINT('Ctrl Pts',(-0.12442160425429,-0.0941146757048641,
1.45274409610553));
#17364=CARTESIAN_POINT('Ctrl Pts',(-0.113115782874773,-0.106896722346074,
1.45406740405386));
#17365=CARTESIAN_POINT('Ctrl Pts',(-0.109531027348519,-0.110566935091132,
1.45446532660342));
#17366=CARTESIAN_POINT('Ctrl Pts',(-0.103385019780831,-0.116266647129765,
1.4551069970546));
#17367=CARTESIAN_POINT('Ctrl Pts',(-0.100929530532689,-0.118404512394445,
1.45535379310498));
#17368=CARTESIAN_POINT('Ctrl Pts',(-0.097484762347844,-0.121218590306139,
1.45568540759061));
#17369=CARTESIAN_POINT('Ctrl Pts',(-0.0965522433164416,-0.121962658432099,
1.4557737769378));
#17370=CARTESIAN_POINT('Ctrl Pts',(-0.0951481141398284,-0.123056830682451,
1.45590465629463));
#17371=CARTESIAN_POINT('Ctrl Pts',(-0.0946829572533972,-0.123415091606327,
1.45594766276057));
#17372=CARTESIAN_POINT('Ctrl Pts',(-0.0938365513568218,-0.124059386055306,
1.45602526836916));
#17373=CARTESIAN_POINT('Ctrl Pts',(-0.0934559977689739,-0.124346315329659,
1.45605992551397));
#17374=CARTESIAN_POINT('Ctrl Pts',(-0.0928439463858557,-0.124803391980281,
1.45611528167249));
#17375=CARTESIAN_POINT('Ctrl Pts',(-0.0926132897209681,-0.124974651833897,
1.45613605645235));
#17376=CARTESIAN_POINT('Ctrl Pts',(-0.0921805918670213,-0.125294069100675,
1.45617486475617));
#17377=CARTESIAN_POINT('Ctrl Pts',(-0.0919786696687933,-0.125442375599448,
1.45619290828136));
#17378=CARTESIAN_POINT('Ctrl Pts',(-0.0915079832365281,-0.125786334765552,
1.45623481462039));
#17379=CARTESIAN_POINT('Ctrl Pts',(-0.0912389495831145,-0.125981614112253,
1.45625865150709));
#17380=CARTESIAN_POINT('Ctrl Pts',(-0.0904071059761214,-0.126581349418227,
1.45633200507005));
#17381=CARTESIAN_POINT('Ctrl Pts',(-0.0898422067906105,-0.12698291522245,
1.45638132790259));
#17382=CARTESIAN_POINT('Ctrl Pts',(-0.0844731044489688,-0.130745844846642,
1.45684569309584));
#17383=CARTESIAN_POINT('Ctrl Pts',(-0.0794844516205588,-0.133837298701754,
1.45724389397698));
#17384=CARTESIAN_POINT('Ctrl Pts',(-0.0654955047627734,-0.141447317290972,
1.45830716768045));
#17385=CARTESIAN_POINT('Ctrl Pts',(-0.0562129904523487,-0.145386087761141,
1.45895811863497));
#17386=CARTESIAN_POINT('Ctrl Pts',(-0.0406558060572818,-0.150272828303824,
1.46004689625182));
#17387=CARTESIAN_POINT('Ctrl Pts',(-0.0345900401560761,-0.151783831623902,
1.46047056160612));
#17388=CARTESIAN_POINT('Ctrl Pts',(-0.0270066512672671,-0.153194646851783,
1.46100852701119));
#17389=CARTESIAN_POINT('Ctrl Pts',(-0.0255592221090781,-0.153442774163672,
1.46111155734078));
#17390=CARTESIAN_POINT('Ctrl Pts',(-0.0234781893404814,-0.153769256504804,
1.46126028305847));
#17391=CARTESIAN_POINT('Ctrl Pts',(-0.0228472455114183,-0.153864268013597,
1.46130545278962));
#17392=CARTESIAN_POINT('Ctrl Pts',(-0.0217510617368836,-0.154022447190428,
1.46138407249907));
#17393=CARTESIAN_POINT('Ctrl Pts',(-0.0212860836033319,-0.154087395854437,
1.46141746591925));
#17394=CARTESIAN_POINT('Ctrl Pts',(-0.0203905331982704,-0.154208356398516,
1.46148187083243));
#17395=CARTESIAN_POINT('Ctrl Pts',(-0.0199600058174525,-0.154264672520849,
1.46151287240982));
#17396=CARTESIAN_POINT('Ctrl Pts',(-0.018829467076732,-0.154407743366576,
1.46159438755667));
#17397=CARTESIAN_POINT('Ctrl Pts',(-0.0181290984750088,-0.154491539574334,
1.46164499364392));
#17398=CARTESIAN_POINT('Ctrl Pts',(-0.0156868821653269,-0.15476690520148,
1.46182184974499));
#17399=CARTESIAN_POINT('Ctrl Pts',(-0.0139424454136736,-0.154933795431414,
1.46194886823718));
#17400=CARTESIAN_POINT('Ctrl Pts',(-0.000967069848389774,-0.155954248321953,
1.46289918150943));
#17401=CARTESIAN_POINT('Ctrl Pts',(0.0103218826449606,-0.155614979710487,
1.46376039466813));
#17402=CARTESIAN_POINT('Ctrl Pts',(0.0309491545747352,-0.15273996312124,
1.46537464278981));
#17403=CARTESIAN_POINT('Ctrl Pts',(0.0402842533858207,-0.150547538675237,
1.46612008562082));
#17404=CARTESIAN_POINT('Ctrl Pts',(0.0502202307510351,-0.147222807003356,
1.46689662719046));
#17405=CARTESIAN_POINT('Ctrl Pts',(0.0510785382727514,-0.146927225203477,
1.46696355276793));
#17406=CARTESIAN_POINT('Ctrl Pts',(0.0523896146094526,-0.146462842278603,
1.46706549354239));
#17407=CARTESIAN_POINT('Ctrl Pts',(0.0528442487279792,-0.146299423374875,
1.46710078934916));
#17408=CARTESIAN_POINT('Ctrl Pts',(0.0535929688179008,-0.146026349307755,
1.46715881978337));
#17409=CARTESIAN_POINT('Ctrl Pts',(0.0538874930350643,-0.145917919043164,
1.46718162239263));
#17410=CARTESIAN_POINT('Ctrl Pts',(0.0544604445138456,-0.145705013354702,
1.46722593019383));
#17411=CARTESIAN_POINT('Ctrl Pts',(0.0547389041125046,-0.145600629510848,
1.46724744057498));
#17412=CARTESIAN_POINT('Ctrl Pts',(0.0552514994867895,-0.145406798747639,
1.46728699164855));
#17413=CARTESIAN_POINT('Ctrl Pts',(0.0554857159518271,-0.145317585461868,
1.46730504551919));
#17414=CARTESIAN_POINT('Ctrl Pts',(0.0560241661246784,-0.145110997655194,
1.46734651011147));
#17415=CARTESIAN_POINT('Ctrl Pts',(0.0563282466725011,-0.144993232471512,
1.46736989717426));
#17416=CARTESIAN_POINT('Ctrl Pts',(0.0572475793965496,-0.144633862058948,
1.46744052137001));
#17417=CARTESIAN_POINT('Ctrl Pts',(0.0578616749148832,-0.144389286370534,
1.4674875849479));
#17418=CARTESIAN_POINT('Ctrl Pts',(0.062588994771145,-0.142471534521782,
1.46784915550281));
#17419=CARTESIAN_POINT('Ctrl Pts',(0.0666309110330868,-0.140626638159003,
1.46815406336401));
#17420=CARTESIAN_POINT('Ctrl Pts',(0.0837838346528959,-0.131891377797621,
1.46945286882374));
#17421=CARTESIAN_POINT('Ctrl Pts',(0.0959518789394761,-0.123322145138005,
1.47039437582479));
#17422=CARTESIAN_POINT('Ctrl Pts',(0.109549190329018,-0.110498160018304,
1.47166801489904));
#17423=CARTESIAN_POINT('Ctrl Pts',(0.112272044791458,-0.107730460295084,
1.47193614076816));
#17424=CARTESIAN_POINT('Ctrl Pts',(0.115501431708237,-0.104192364136783,
1.47227272693303));
#17425=CARTESIAN_POINT('Ctrl Pts',(0.116108576133004,-0.103515351309303,
1.47233686470461));
#17426=CARTESIAN_POINT('Ctrl Pts',(0.117058159788745,-0.102437627347766,
1.4724385673571));
#17427=CARTESIAN_POINT('Ctrl Pts',(0.117404565578478,-0.10204042453194,
1.47247596677038));
#17428=CARTESIAN_POINT('Ctrl Pts',(0.118049777825564,-0.10129296331252,
1.47254619378121));
#17429=CARTESIAN_POINT('Ctrl Pts',(0.118349061666832,-0.100943122873771,
1.47257900119857));
#17430=CARTESIAN_POINT('Ctrl Pts',(0.119014770133553,-0.100157929230913,
1.47265250167308));
#17431=CARTESIAN_POINT('Ctrl Pts',(0.119380366170484,-0.0997218855360148,
1.47269322796467));
#17432=CARTESIAN_POINT('Ctrl Pts',(0.120299497932282,-0.0986133456734842,
1.47279654268661));
#17433=CARTESIAN_POINT('Ctrl Pts',(0.120849786575204,-0.097938195690126,
1.47285926102369));
#17434=CARTESIAN_POINT('Ctrl Pts',(0.123931884101641,-0.0940912375239001,
1.47321551952547));
#17435=CARTESIAN_POINT('Ctrl Pts',(0.12634423975266,-0.0908262092641361,
1.47351373311157));
#17436=CARTESIAN_POINT('Ctrl Pts',(0.129677174229151,-0.0859251260479744,
1.47395599148305));
#17437=CARTESIAN_POINT('Ctrl Pts',(0.130700358120536,-0.0843606110481342,
1.47409639616372));
#17438=CARTESIAN_POINT('Ctrl Pts',(0.139530188385669,-0.0703128715222547,
1.47535011854989));
#17439=CARTESIAN_POINT('Ctrl Pts',(0.145554817728985,-0.0568004479896118,
1.47651773171049));
#17440=CARTESIAN_POINT('Ctrl Pts',(0.150297799419483,-0.0401625635120625,
1.47781904721061));
#17441=CARTESIAN_POINT('Ctrl Pts',(0.150943372028449,-0.037663783351134,
1.47801080598762));
#17442=CARTESIAN_POINT('Ctrl Pts',(0.151648188697762,-0.0346254135198081,
1.4782386517208));
#17443=CARTESIAN_POINT('Ctrl Pts',(0.151767134934008,-0.0341002811383624,
1.47827784040259));
#17444=CARTESIAN_POINT('Ctrl Pts',(0.151948190899554,-0.0332812261503539,
1.4783386556423));
#17445=CARTESIAN_POINT('Ctrl Pts',(0.152012178402532,-0.0329877303434083,
1.47836038643159));
#17446=CARTESIAN_POINT('Ctrl Pts',(0.152129488893868,-0.0324420643481126,
1.47840067185755));
#17447=CARTESIAN_POINT('Ctrl Pts',(0.152183034803574,-0.0321899495197964,
1.47841923864801));
#17448=CARTESIAN_POINT('Ctrl Pts',(0.152302902619557,-0.0316185810926165,
1.47846121270219));
#17449=CARTESIAN_POINT('Ctrl Pts',(0.152368847373672,-0.0312992519392227,
1.47848459826537));
#17450=CARTESIAN_POINT('Ctrl Pts',(0.152565410643715,-0.0303320743832381,
1.47855521345657));
#17451=CARTESIAN_POINT('Ctrl Pts',(0.152692907338625,-0.0296835872399399,
1.4786022695946));
#17452=CARTESIAN_POINT('Ctrl Pts',(0.153646851598111,-0.0246626897207158,
1.47896449404554));
#17453=CARTESIAN_POINT('Ctrl Pts',(0.154289562871379,-0.0202569336694151,
1.4792700215471));
#17454=CARTESIAN_POINT('Ctrl Pts',(0.156250945074814,-0.00108291402047901,
1.48057041607453));
#17455=CARTESIAN_POINT('Ctrl Pts',(0.155643980696658,0.0138032492495018,
1.48151289734109));
#17456=CARTESIAN_POINT('Ctrl Pts',(0.152235093389752,0.032174147735988,
1.48278634181575));
#17457=CARTESIAN_POINT('Ctrl Pts',(0.151389978387864,0.0359411964516643,
1.48305299247909));
#17458=CARTESIAN_POINT('Ctrl Pts',(0.15017419118367,0.0405504488736418,
1.4833879420295));
#17459=CARTESIAN_POINT('Ctrl Pts',(0.149934983553131,0.0414261661999468,
1.48345196957891));
#17460=CARTESIAN_POINT('Ctrl Pts',(0.149544902348627,0.0428065659085886,
1.4835535369468));
#17461=CARTESIAN_POINT('Ctrl Pts',(0.149399104157245,0.0433126721404501,
1.48359091204912));
#17462=CARTESIAN_POINT('Ctrl Pts',(0.149121038802963,0.0442598043363893,
1.48366111740284));
#17463=CARTESIAN_POINT('Ctrl Pts',(0.148989377996394,0.0447010036738334,
1.48369392759408));
#17464=CARTESIAN_POINT('Ctrl Pts',(0.148690485271175,0.045686611111643,
1.48376746552164));
#17465=CARTESIAN_POINT('Ctrl Pts',(0.148522219139039,0.0462306959833868,
1.48380822664702));
#17466=CARTESIAN_POINT('Ctrl Pts',(0.148088593398823,0.0476060118109163,
1.48391168857637));
#17467=CARTESIAN_POINT('Ctrl Pts',(0.147819223451407,0.0484359471460012,
1.48397451993311));
#17468=CARTESIAN_POINT('Ctrl Pts',(0.146250907906993,0.0531330056507727,
1.48433242268847));
#17469=CARTESIAN_POINT('Ctrl Pts',(0.14480733046948,0.0569497641838245,
1.48463221769303));
#17470=CARTESIAN_POINT('Ctrl Pts',(0.142493434724198,0.0624087125628709,
1.4850747108299));
#17471=CARTESIAN_POINT('Ctrl Pts',(0.141740995629489,0.064099266948442,
1.4852137061978));
#17472=CARTESIAN_POINT('Ctrl Pts',(0.134726915753676,0.0791305219141532,
1.48646708409862));
#17473=CARTESIAN_POINT('Ctrl Pts',(0.126630198981664,0.0915297580205269,
1.48763587098451));
#17474=CARTESIAN_POINT('Ctrl Pts',(0.115220403714577,0.104530525350124,
1.48893671597374));
#17475=CARTESIAN_POINT('Ctrl Pts',(0.113482210491339,0.106415046599015,
1.48912718000755));
#17476=CARTESIAN_POINT('Ctrl Pts',(0.111324116088501,0.108641761957279,
1.4893536949623));
#17477=CARTESIAN_POINT('Ctrl Pts',(0.110948127501568,0.109025704725514,
1.48939280626932));
#17478=CARTESIAN_POINT('Ctrl Pts',(0.110359031453347,0.109621059885288,
1.48945352779327));
#17479=CARTESIAN_POINT('Ctrl Pts',(0.110147293978273,0.109833811857386,
1.4894752417319));
#17480=CARTESIAN_POINT('Ctrl Pts',(0.109752580500884,0.110228127154517,
1.48951551194084));
#17481=CARTESIAN_POINT('Ctrl Pts',(0.10956977088265,0.110409846721838,1.48953408028221));
#17482=CARTESIAN_POINT('Ctrl Pts',(0.109154462501349,0.110820631372166,
1.48957607826367));
#17483=CARTESIAN_POINT('Ctrl Pts',(0.108921694425129,0.111049419226494,
1.48959948609944));
#17484=CARTESIAN_POINT('Ctrl Pts',(0.108229627143164,0.111725383075129,
1.48966870239664));
#17485=CARTESIAN_POINT('Ctrl Pts',(0.107768274202797,0.11217046192405,1.48971435105897));
#17486=CARTESIAN_POINT('Ctrl Pts',(0.104320196925757,0.115455998311285,
1.49005200372553));
#17487=CARTESIAN_POINT('Ctrl Pts',(0.101224048397197,0.118179907897032,
1.4903357453819));
#17488=CARTESIAN_POINT('Ctrl Pts',(0.0944537116180991,0.123674695446542,
1.49092574789563));
#17489=CARTESIAN_POINT('Ctrl Pts',(0.0907575486910384,0.126412049213838,
1.49123056583958));
#17490=CARTESIAN_POINT('Ctrl Pts',(0.0802684797198167,0.133482627971982,
1.4920651201986));
#17491=CARTESIAN_POINT('Ctrl Pts',(0.0732524561281435,0.137458039535143,
1.4925909880447));
#17492=CARTESIAN_POINT('Ctrl Pts',(0.0622720201376527,0.142599384165511,
1.49340398158541));
#17493=CARTESIAN_POINT('Ctrl Pts',(0.0585175391296592,0.144180727764252,
1.49368018723737));
#17494=CARTESIAN_POINT('Ctrl Pts',(0.0523437859084846,0.146500156571934,
1.49413503204976));
#17495=CARTESIAN_POINT('Ctrl Pts',(0.0499608954449104,0.147329818643918,
1.4943107294488));
#17496=CARTESIAN_POINT('Ctrl Pts',(0.0468101115165871,0.14834161460208,
1.49454371466506));
#17497=CARTESIAN_POINT('Ctrl Pts',(0.0460594253692922,0.148576412854791,
1.49459927262882));
#17498=CARTESIAN_POINT('Ctrl Pts',(0.0448288119657272,0.148951099299118,
1.49469044343985));
#17499=CARTESIAN_POINT('Ctrl Pts',(0.0443499270738089,0.149094387294051,
1.4947259449938));
#17500=CARTESIAN_POINT('Ctrl Pts',(0.0434229252378279,0.149366895820032,
1.49479471568083));
#17501=CARTESIAN_POINT('Ctrl Pts',(0.0429749008280187,0.149496414315641,
1.49482797470186));
#17502=CARTESIAN_POINT('Ctrl Pts',(0.0419410275847551,0.149790263124095,
1.49490477792963));
#17503=CARTESIAN_POINT('Ctrl Pts',(0.0413547867953527,0.149953173728624,
1.49494836764182));
#17504=CARTESIAN_POINT('Ctrl Pts',(0.0397800928699485,0.150380829341477,
1.49506556808322));
#17505=CARTESIAN_POINT('Ctrl Pts',(0.0387899729541331,0.150639262900873,
1.49513938109479));
#17506=CARTESIAN_POINT('Ctrl Pts',(0.0303222044629162,0.152760437628917,
1.49577178373413));
#17507=CARTESIAN_POINT('Ctrl Pts',(0.0227195059877597,0.154074576238643,
1.49634792594783));
#17508=CARTESIAN_POINT('Ctrl Pts',(0.00542278598953225,0.155756192039893,
1.49767623381201));
#17509=CARTESIAN_POINT('Ctrl Pts',(-0.00427251752851013,0.155791935864253,
1.49843351483685));
#17510=CARTESIAN_POINT('Ctrl Pts',(-0.0175733425171971,0.154597954370988,
1.49945914687245));
#17511=CARTESIAN_POINT('Ctrl Pts',(-0.0212267375298337,0.154138832514533,
1.49973922890827));
#17512=CARTESIAN_POINT('Ctrl Pts',(-0.0267871768189891,0.153238566954269,
1.50015998097054));
#17513=CARTESIAN_POINT('Ctrl Pts',(-0.0287077740239233,0.152890404927404,
1.50030428317809));
#17514=CARTESIAN_POINT('Ctrl Pts',(-0.0311050698127636,0.152409056398671,
1.50048270106527));
#17515=CARTESIAN_POINT('Ctrl Pts',(-0.0315882565704743,0.152309644819597,
1.50051857495411));
#17516=CARTESIAN_POINT('Ctrl Pts',(-0.0323551653793269,0.152148053308166,
1.50057536640989));
#17517=CARTESIAN_POINT('Ctrl Pts',(-0.0326391946659658,0.152087375634961,
1.50059636732096));
#17518=CARTESIAN_POINT('Ctrl Pts',(-0.0331765734398989,0.151970999734814,
1.50063603768734));
#17519=CARTESIAN_POINT('Ctrl Pts',(-0.0334299502935069,0.151915464026069,
1.50065471562645));
#17520=CARTESIAN_POINT('Ctrl Pts',(-0.0340113409566138,0.151786508508554,
1.50069751344723));
#17521=CARTESIAN_POINT('Ctrl Pts',(-0.0343392565427413,0.151712659144659,
1.50072160852585));
#17522=CARTESIAN_POINT('Ctrl Pts',(-0.0352141459113909,0.151512644748447,
1.50078578453248));
#17523=CARTESIAN_POINT('Ctrl Pts',(-0.0357606873851245,0.15138457931469,
1.50082575970356));
#17524=CARTESIAN_POINT('Ctrl Pts',(-0.0397181838498521,0.150434631511984,
1.50111446185025));
#17525=CARTESIAN_POINT('Ctrl Pts',(-0.0431014933384724,0.14950043024761,
1.50135719576532));
#17526=CARTESIAN_POINT('Ctrl Pts',(-0.0510483094276349,0.147013879926685,
1.50192396544413));
#17527=CARTESIAN_POINT('Ctrl Pts',(-0.0555770073255496,0.145362352243247,
1.50224429122203));
#17528=CARTESIAN_POINT('Ctrl Pts',(-0.0612512216731276,0.142989040176923,
1.50265055624028));
#17529=CARTESIAN_POINT('Ctrl Pts',(-0.0624735223751187,0.142459241037525,
1.50273836689477));
#17530=CARTESIAN_POINT('Ctrl Pts',(-0.0636886280167373,0.141913921661498,
1.50282608545586));
#17531=CARTESIAN_POINT('Origin',(0.,0.,-0.129405622560373));
#17532=CARTESIAN_POINT('',(-0.0636885910816305,0.141913938237359,1.58655050058549));
#17533=CARTESIAN_POINT('',(-0.0636886258330468,0.141913922641502,1.57264613271722));
#17534=CARTESIAN_POINT('',(-0.0636886258329924,0.141913922641526,-0.129405622560373));
#17535=CARTESIAN_POINT('',(-0.155549955824825,-0.000117230094128791,1.52948519617329));
#17536=CARTESIAN_POINT('Ctrl Pts',(-0.0636885910816225,0.141913938237362,
1.58655050058549));
#17537=CARTESIAN_POINT('Ctrl Pts',(-0.0556566821640682,0.145518524009616,
1.58596898071156));
#17538=CARTESIAN_POINT('Ctrl Pts',(-0.0473230433865961,0.148439344786728,
1.58539453072637));
#17539=CARTESIAN_POINT('Ctrl Pts',(-0.0369753918880226,0.15110286815688,
1.58467671135735));
#17540=CARTESIAN_POINT('Ctrl Pts',(-0.0351674945549438,0.15153383555548,
1.58455118008554));
#17541=CARTESIAN_POINT('Ctrl Pts',(-0.029377214912228,0.152804924617277,
1.58414806595958));
#17542=CARTESIAN_POINT('Ctrl Pts',(-0.0253696890077411,0.1535211375448,
1.5838674194839));
#17543=CARTESIAN_POINT('Ctrl Pts',(-0.020475120461954,0.154199002900961,
1.58352053583815));
#17544=CARTESIAN_POINT('Ctrl Pts',(-0.0196102935714569,0.154311371533294,
1.58345909242817));
#17545=CARTESIAN_POINT('Ctrl Pts',(-0.0181792653722453,0.154485083758022,
1.58335714966645));
#17546=CARTESIAN_POINT('Ctrl Pts',(-0.0176135821246357,0.154550601753242,
1.58331678168058));
#17547=CARTESIAN_POINT('Ctrl Pts',(-0.0165897724954009,0.154663486526208,
1.5832435885002));
#17548=CARTESIAN_POINT('Ctrl Pts',(-0.0161317690197289,0.154711927904163,
1.58321079744361));
#17549=CARTESIAN_POINT('Ctrl Pts',(-0.0151492142706765,0.154811438748106,
1.58314034474764));
#17550=CARTESIAN_POINT('Ctrl Pts',(-0.0146246064298436,0.154861877602033,
1.58310266374686));
#17551=CARTESIAN_POINT('Ctrl Pts',(-0.0131946410138899,0.15499203196548,
1.58299977156646));
#17552=CARTESIAN_POINT('Ctrl Pts',(-0.012288837353915,0.155066479084393,
1.58293439632498));
#17553=CARTESIAN_POINT('Ctrl Pts',(-0.0075212108637616,0.1554162904106,
1.58258920501048));
#17554=CARTESIAN_POINT('Ctrl Pts',(-0.00365108860593273,0.155555316686229,
1.58230517371162));
#17555=CARTESIAN_POINT('Ctrl Pts',(0.0150428509126474,0.155528890487122,
1.58091321801508));
#17556=CARTESIAN_POINT('Ctrl Pts',(0.0297856744671923,0.153389011804456,
1.5797448052151));
#17557=CARTESIAN_POINT('Ctrl Pts',(0.0482562558965439,0.147942019332466,
1.57827325319499));
#17558=CARTESIAN_POINT('Ctrl Pts',(0.0524588000232345,0.146504575755587,
1.57793874454224));
#17559=CARTESIAN_POINT('Ctrl Pts',(0.0572099228700218,0.144648759804374,
1.57756512209116));
#17560=CARTESIAN_POINT('Ctrl Pts',(0.0578237920587437,0.144404460116962,
1.5775169383558));
#17561=CARTESIAN_POINT('Ctrl Pts',(0.058738299094188,0.144033749690548,
1.57744531147985));
#17562=CARTESIAN_POINT('Ctrl Pts',(0.0590401153383496,0.143910297117811,
1.5774216976075));
#17563=CARTESIAN_POINT('Ctrl Pts',(0.0595798627299743,0.143687539217213,
1.57737951631109));
#17564=CARTESIAN_POINT('Ctrl Pts',(0.0598179361593073,0.143588591073243,
1.57736092785211));
#17565=CARTESIAN_POINT('Ctrl Pts',(0.0603330154932123,0.143373010265121,
1.57732074831686));
#17566=CARTESIAN_POINT('Ctrl Pts',(0.0606099289638933,0.143256166869518,
1.57729917025226));
#17567=CARTESIAN_POINT('Ctrl Pts',(0.0613824117816885,0.142927577618771,
1.57723903520187));
#17568=CARTESIAN_POINT('Ctrl Pts',(0.0618772285626696,0.142714055118859,
1.57720058404964));
#17569=CARTESIAN_POINT('Ctrl Pts',(0.0647401251846981,0.141460973749207,
1.57697845592858));
#17570=CARTESIAN_POINT('Ctrl Pts',(0.0670832736254019,0.140364979302545,
1.57679801237641));
#17571=CARTESIAN_POINT('Ctrl Pts',(0.0825731030057564,0.132643131517349,
1.57560708805293));
#17572=CARTESIAN_POINT('Ctrl Pts',(0.094750267783738,0.124237730949311,
1.57467392033339));
#17573=CARTESIAN_POINT('Ctrl Pts',(0.106960209445948,0.112955408353615,
1.57355700766039));
#17574=CARTESIAN_POINT('Ctrl Pts',(0.108331551213944,0.111640876414733,
1.57342867826927));
#17575=CARTESIAN_POINT('Ctrl Pts',(0.11253190951898,0.107464248395496,1.57302573598501));
#17576=CARTESIAN_POINT('Ctrl Pts',(0.115273968044647,0.104517476238519,
1.57274817229802));
#17577=CARTESIAN_POINT('Ctrl Pts',(0.118465297370982,0.100809378217501,
1.57240470942564));
#17578=CARTESIAN_POINT('Ctrl Pts',(0.119026531521166,0.100146104054536,
1.57234349162891));
#17579=CARTESIAN_POINT('Ctrl Pts',(0.119945717366291,0.0990411557789255,
1.57224184598916));
#17580=CARTESIAN_POINT('Ctrl Pts',(0.120306862379425,0.0986021526204787,
1.57220154816511));
#17581=CARTESIAN_POINT('Ctrl Pts',(0.120956183908531,0.0978039678336131,
1.57212843000783));
#17582=CARTESIAN_POINT('Ctrl Pts',(0.121245188648127,0.0974454656258248,
1.57209564348913));
#17583=CARTESIAN_POINT('Ctrl Pts',(0.121861992679752,0.0966733457073927,
1.57202514263034));
#17584=CARTESIAN_POINT('Ctrl Pts',(0.122189286471885,0.0962593335160649,
1.57198740867769));
#17585=CARTESIAN_POINT('Ctrl Pts',(0.12307650856888,0.0951252206334363,
1.5718842241905));
#17586=CARTESIAN_POINT('Ctrl Pts',(0.123632211881265,0.0944018574052578,
1.57181860801666));
#17587=CARTESIAN_POINT('Ctrl Pts',(0.126540837546597,0.0905459440414115,
1.5714698258673));
#17588=CARTESIAN_POINT('Ctrl Pts',(0.128780943135694,0.0873304936325884,
1.57118233946005));
#17589=CARTESIAN_POINT('Ctrl Pts',(0.138887336311401,0.0715881151431334,
1.56978886304873));
#17590=CARTESIAN_POINT('Ctrl Pts',(0.145060854949176,0.0580667996396583,
1.56862296286742));
#17591=CARTESIAN_POINT('Ctrl Pts',(0.150478939492959,0.0396412815761459,
1.56715551576624));
#17592=CARTESIAN_POINT('Ctrl Pts',(0.151544784499264,0.0353486877907396,
1.56682245053035));
#17593=CARTESIAN_POINT('Ctrl Pts',(0.15255801130537,0.0303692503469366,
1.56645024136146));
#17594=CARTESIAN_POINT('Ctrl Pts',(0.152685509662734,0.0297215975510851,
1.56640210267336));
#17595=CARTESIAN_POINT('Ctrl Pts',(0.152869808344361,0.0287529206726211,
1.56633052945828));
#17596=CARTESIAN_POINT('Ctrl Pts',(0.152929726256561,0.0284325092603508,
1.56630692456872));
#17597=CARTESIAN_POINT('Ctrl Pts',(0.153035229685331,0.0278583459606465,
1.56626475294019));
#17598=CARTESIAN_POINT('Ctrl Pts',(0.153081191748813,0.0276046680979614,
1.56624616520777));
#17599=CARTESIAN_POINT('Ctrl Pts',(0.1531793867987,0.0270549135134226,1.56620597997554));
#17600=CARTESIAN_POINT('Ctrl Pts',(0.15323139204343,0.0267588000823964,
1.56618439551956));
#17601=CARTESIAN_POINT('Ctrl Pts',(0.153374289456989,0.025931075945803,
1.5661242246527));
#17602=CARTESIAN_POINT('Ctrl Pts',(0.153463277064963,0.0253991334819934,
1.56608574427951));
#17603=CARTESIAN_POINT('Ctrl Pts',(0.153964016877278,0.0223071164953629,
1.56586310822235));
#17604=CARTESIAN_POINT('Ctrl Pts',(0.154314502410786,0.0197373354956073,
1.56568220327));
#17605=CARTESIAN_POINT('Ctrl Pts',(0.156223997462395,0.00253380361185688,
1.5644912848206));
#17606=CARTESIAN_POINT('Ctrl Pts',(0.155763942122512,-0.0122499353637323,
1.56355843465293));
#17607=CARTESIAN_POINT('Ctrl Pts',(0.1529045904742,-0.0286291255538685,
1.56244134592911));
#17608=CARTESIAN_POINT('Ctrl Pts',(0.152542051866071,-0.0305018461616655,
1.56231248056851));
#17609=CARTESIAN_POINT('Ctrl Pts',(0.151309670152531,-0.0362947451860791,
1.56190957189021));
#17610=CARTESIAN_POINT('Ctrl Pts',(0.150322477734291,-0.0401879675000319,
1.56163259952195));
#17611=CARTESIAN_POINT('Ctrl Pts',(0.14894005216354,-0.0448711181363862,
1.56128979096042));
#17612=CARTESIAN_POINT('Ctrl Pts',(0.148687271128286,-0.0457017694546805,
1.56122861475013));
#17613=CARTESIAN_POINT('Ctrl Pts',(0.148257561911159,-0.0470725055479746,
1.56112702388317));
#17614=CARTESIAN_POINT('Ctrl Pts',(0.148084601901424,-0.047613822641663,
1.56108673899788));
#17615=CARTESIAN_POINT('Ctrl Pts',(0.147766130500411,-0.0485920283040405,
1.56101363465571));
#17616=CARTESIAN_POINT('Ctrl Pts',(0.147621637264206,-0.0490292437310833,
1.56098084895372));
#17617=CARTESIAN_POINT('Ctrl Pts',(0.147307332476802,-0.0499662983611577,
1.56091033911669));
#17618=CARTESIAN_POINT('Ctrl Pts',(0.147136913947535,-0.0504659262736511,
1.56087259532246));
#17619=CARTESIAN_POINT('Ctrl Pts',(0.146664889008093,-0.0518270780518389,
1.56076935648805));
#17620=CARTESIAN_POINT('Ctrl Pts',(0.14635824139556,-0.05268681805503,1.56070369551455));
#17621=CARTESIAN_POINT('Ctrl Pts',(0.144692481630524,-0.0572302822320028,
1.56035424050756));
#17622=CARTESIAN_POINT('Ctrl Pts',(0.143201939211302,-0.060863937608011,
1.56006610617318));
#17623=CARTESIAN_POINT('Ctrl Pts',(0.135451344610029,-0.0778928958688598,
1.55867234057212));
#17624=CARTESIAN_POINT('Ctrl Pts',(0.127440169506251,-0.0904059070917594,
1.55750690693877));
#17625=CARTESIAN_POINT('Ctrl Pts',(0.114902357022042,-0.104941696078521,
1.55604022870995));
#17626=CARTESIAN_POINT('Ctrl Pts',(0.111875995914586,-0.108162293550515,
1.55570743735417));
#17627=CARTESIAN_POINT('Ctrl Pts',(0.108244311040234,-0.111711266904603,
1.55533549643098));
#17628=CARTESIAN_POINT('Ctrl Pts',(0.107769374344055,-0.112169514670204,
1.55528736634133));
#17629=CARTESIAN_POINT('Ctrl Pts',(0.107055531867526,-0.112849553972302,
1.55521580336939));
#17630=CARTESIAN_POINT('Ctrl Pts',(0.106818830509863,-0.113073631713981,
1.55519220019493));
#17631=CARTESIAN_POINT('Ctrl Pts',(0.106393647576462,-0.113473612434715,
1.55515003041178));
#17632=CARTESIAN_POINT('Ctrl Pts',(0.106205432294646,-0.113649791545102,
1.55513144281756));
#17633=CARTESIAN_POINT('Ctrl Pts',(0.105796764802373,-0.114030423365754,
1.5550912564952));
#17634=CARTESIAN_POINT('Ctrl Pts',(0.105576158176472,-0.114234704553788,
1.55506967081703));
#17635=CARTESIAN_POINT('Ctrl Pts',(0.104958121374668,-0.114803685520051,
1.55500949310048));
#17636=CARTESIAN_POINT('Ctrl Pts',(0.104559379171323,-0.11516696445515,
1.55497100713885));
#17637=CARTESIAN_POINT('Ctrl Pts',(0.102231973945652,-0.117265323800681,
1.55474827376936));
#17638=CARTESIAN_POINT('Ctrl Pts',(0.100261889740756,-0.118954143513077,
1.55456728041599));
#17639=CARTESIAN_POINT('Ctrl Pts',(0.0868424298189114,-0.129887333099358,
1.55337636296554));
#17640=CARTESIAN_POINT('Ctrl Pts',(0.0741724075246528,-0.137516871166556,
1.55244357354668));
#17641=CARTESIAN_POINT('Ctrl Pts',(0.0588595508066705,-0.143996526635533,
1.55132645033646));
#17642=CARTESIAN_POINT('Ctrl Pts',(0.0570880699550032,-0.144707975802186,
1.55119748163509));
#17643=CARTESIAN_POINT('Ctrl Pts',(0.051552664492229,-0.146813602988849,
1.55079457934938));
#17644=CARTESIAN_POINT('Ctrl Pts',(0.0477478216708934,-0.148094739961655,
1.55051772090849));
#17645=CARTESIAN_POINT('Ctrl Pts',(0.0430651036888921,-0.149472248346351,
1.55017503841363));
#17646=CARTESIAN_POINT('Ctrl Pts',(0.0422302225422405,-0.149710268288718,
1.55011387022457));
#17647=CARTESIAN_POINT('Ctrl Pts',(0.040845652384426,-0.150092498424037,
1.55001228992244));
#17648=CARTESIAN_POINT('Ctrl Pts',(0.04029707939573,-0.150240709458207,
1.54997200753299));
#17649=CARTESIAN_POINT('Ctrl Pts',(0.0393025272743941,-0.150503574327373,
1.549898905855));
#17650=CARTESIAN_POINT('Ctrl Pts',(0.038856825538882,-0.150619260508583,
1.54986612030983));
#17651=CARTESIAN_POINT('Ctrl Pts',(0.0384094511441652,-0.150733262965616,
1.54983318460491));
#17652=CARTESIAN_POINT('Ctrl Pts',(0.0384082812240369,-0.150733561076728,
1.5498330984752));
#17653=CARTESIAN_POINT('Ctrl Pts',(0.0384059482241151,-0.150734155527031,
1.54983292671899));
#17654=CARTESIAN_POINT('Ctrl Pts',(0.0384047849173861,-0.150734451924203,
1.5498328410758));
#17655=CARTESIAN_POINT('Ctrl Pts',(0.0384024648054546,-0.150735043033431,
1.54983267026768));
#17656=CARTESIAN_POINT('Ctrl Pts',(0.0384013079879752,-0.150735337748775,
1.54983258510185));
#17657=CARTESIAN_POINT('Ctrl Pts',(0.038399000799677,-0.150735925508802,
1.54983241524446));
#17658=CARTESIAN_POINT('Ctrl Pts',(0.0383978504192419,-0.150736218556093,
1.54983233055217));
#17659=CARTESIAN_POINT('Ctrl Pts',(0.0383955560448425,-0.150736802995819,
1.54983216163743));
#17660=CARTESIAN_POINT('Ctrl Pts',(0.0383944120462634,-0.150737094389585,
1.54983207741463));
#17661=CARTESIAN_POINT('Ctrl Pts',(0.0383921303896934,-0.150737675534414,
1.54983190943548));
#17662=CARTESIAN_POINT('Ctrl Pts',(0.0383909927238457,-0.150737965287632,
1.54983182567856));
#17663=CARTESIAN_POINT('Ctrl Pts',(0.0383887236718577,-0.150738543167327,
1.54983165862668));
#17664=CARTESIAN_POINT('Ctrl Pts',(0.0383875922829476,-0.150738831294662,
1.54983157533152));
#17665=CARTESIAN_POINT('Ctrl Pts',(0.0383853357452364,-0.15073940593313,
1.54983140920027));
#17666=CARTESIAN_POINT('Ctrl Pts',(0.0383842105854601,-0.150739692447207,
1.54983132636337));
#17667=CARTESIAN_POINT('Ctrl Pts',(0.0378784145714043,-0.150868483838546,
1.54979408839843));
#17668=CARTESIAN_POINT('Ctrl Pts',(0.0373731072941603,-0.150994452034455,
1.54975685181441));
#17669=CARTESIAN_POINT('Ctrl Pts',(0.0360039248769304,-0.151328481988625,
1.54965585637752));
#17670=CARTESIAN_POINT('Ctrl Pts',(0.0351388954336563,-0.151531679969435,
1.54959194240574));
#17671=CARTESIAN_POINT('Ctrl Pts',(0.033215670583364,-0.151966097899554,
1.54944958677945));
#17672=CARTESIAN_POINT('Ctrl Pts',(0.0321567139432671,-0.152193696719653,
1.54937103286091));
#17673=CARTESIAN_POINT('Ctrl Pts',(0.0289305899631102,-0.152851906613502,
1.54913116213137));
#17674=CARTESIAN_POINT('Ctrl Pts',(0.0267566307217201,-0.153247401894846,
1.54896875973545));
#17675=CARTESIAN_POINT('Ctrl Pts',(0.00971253633883327,-0.155974418521599,
1.54768915225262));
#17676=CARTESIAN_POINT('Ctrl Pts',(-0.00541511996463198,-0.156182133455611,
1.54650455329011));
#17677=CARTESIAN_POINT('Ctrl Pts',(-0.0213156022871069,-0.154085794186762,
1.54527632582219));
#17678=CARTESIAN_POINT('Ctrl Pts',(-0.0222979999171409,-0.153946699031075,
1.54520055812721));
#17679=CARTESIAN_POINT('Ctrl Pts',(-0.027084322626774,-0.153222237503554,
1.54483216666574));
#17680=CARTESIAN_POINT('Ctrl Pts',(-0.0308673593586107,-0.152505170350796,
1.54454330112266));
#17681=CARTESIAN_POINT('Ctrl Pts',(-0.0352348124117305,-0.151508111477618,
1.54421531433216));
#17682=CARTESIAN_POINT('Ctrl Pts',(-0.035848513556617,-0.151364077513409,
1.54416935515123));
#17683=CARTESIAN_POINT('Ctrl Pts',(-0.0367764532943639,-0.151140332324158,
1.54410007512831));
#17684=CARTESIAN_POINT('Ctrl Pts',(-0.0370913361095948,-0.151063365389453,
1.54407660304249));
#17685=CARTESIAN_POINT('Ctrl Pts',(-0.0376560979925255,-0.150923448088007,
1.54403457379678));
#17686=CARTESIAN_POINT('Ctrl Pts',(-0.037906061975162,-0.150860860953929,
1.54401599625702));
#17687=CARTESIAN_POINT('Ctrl Pts',(-0.0384486518283259,-0.150723571077916,
1.54397572429345));
#17688=CARTESIAN_POINT('Ctrl Pts',(-0.0387412152232905,-0.150648637408858,
1.54395404339664));
#17689=CARTESIAN_POINT('Ctrl Pts',(-0.0395616785001038,-0.150435945653083,
1.54389333129864));
#17690=CARTESIAN_POINT('Ctrl Pts',(-0.0400890817171997,-0.150296259771007,
1.54385440924167));
#17691=CARTESIAN_POINT('Ctrl Pts',(-0.0431834631573669,-0.149459247171671,
1.54362659971488));
#17692=CARTESIAN_POINT('Ctrl Pts',(-0.0457331476969293,-0.148698888836349,
1.54344113449963));
#17693=CARTESIAN_POINT('Ctrl Pts',(-0.0621986944461384,-0.143324937242515,
1.5422504559959));
#17694=CARTESIAN_POINT('Ctrl Pts',(-0.0754234495681357,-0.136828813611224,
1.54132086961655));
#17695=CARTESIAN_POINT('Ctrl Pts',(-0.0891924794692178,-0.127453837113262,
1.54020156738352));
#17696=CARTESIAN_POINT('Ctrl Pts',(-0.0908190090555407,-0.12629998460038,
1.54006678877674));
#17697=CARTESIAN_POINT('Ctrl Pts',(-0.0955754575545617,-0.122786386575669,
1.53966418471888));
#17698=CARTESIAN_POINT('Ctrl Pts',(-0.0986386532251725,-0.12033942185457,
1.53939367059065));
#17699=CARTESIAN_POINT('Ctrl Pts',(-0.102321989093311,-0.117161884816545,
1.5390521152515));
#17700=CARTESIAN_POINT('Ctrl Pts',(-0.103032336512979,-0.116537694623025,
1.5389854596192));
#17701=CARTESIAN_POINT('Ctrl Pts',(-0.104139904084976,-0.115546420695352,
1.53888026126525));
#17702=CARTESIAN_POINT('Ctrl Pts',(-0.104540985114314,-0.115183668010008,
1.53884189974842));
#17703=CARTESIAN_POINT('Ctrl Pts',(-0.105245572700112,-0.114539701059432,
1.53877403230619));
#17704=CARTESIAN_POINT('Ctrl Pts',(-0.105549865940272,-0.114259351852185,
1.53874456317922));
#17705=CARTESIAN_POINT('Ctrl Pts',(-0.106171531832482,-0.113682000611127,
1.53868402889633));
#17706=CARTESIAN_POINT('Ctrl Pts',(-0.106488785044677,-0.113384875919292,
1.53865295865482));
#17707=CARTESIAN_POINT('Ctrl Pts',(-0.107374542791091,-0.112548319597805,
1.53856570780345));
#17708=CARTESIAN_POINT('Ctrl Pts',(-0.107940215108548,-0.112005922184834,
1.53850939976295));
#17709=CARTESIAN_POINT('Ctrl Pts',(-0.110396007242005,-0.109615293510668,
1.53826233353636));
#17710=CARTESIAN_POINT('Ctrl Pts',(-0.112242828511042,-0.107723427538483,
1.53806967550875));
#17711=CARTESIAN_POINT('Ctrl Pts',(-0.117008391145977,-0.102585986612004,
1.53755350668103));
#17712=CARTESIAN_POINT('Ctrl Pts',(-0.119840092423245,-0.0992632562063584,
1.53722663949761));
#17713=CARTESIAN_POINT('Ctrl Pts',(-0.125319458678206,-0.0922570627906749,
1.53655144489211));
#17714=CARTESIAN_POINT('Ctrl Pts',(-0.127953316081791,-0.0885679207499895,
1.53620308667115));
#17715=CARTESIAN_POINT('Ctrl Pts',(-0.136444596427738,-0.0755036163819786,
1.53499794868475));
#17716=CARTESIAN_POINT('Ctrl Pts',(-0.141462839237484,-0.0656218689355162,
1.53413205024323));
#17717=CARTESIAN_POINT('Ctrl Pts',(-0.145801859913025,-0.0542121062604883,
1.53322971772738));
#17718=CARTESIAN_POINT('Ctrl Pts',(-0.14620014266447,-0.0531286487386191,
1.53314498102163));
#17719=CARTESIAN_POINT('Ctrl Pts',(-0.146727444750919,-0.0516433667767692,
1.5330302003167));
#17720=CARTESIAN_POINT('Ctrl Pts',(-0.146866931506856,-0.0512453394583839,
1.53299957590929));
#17721=CARTESIAN_POINT('Ctrl Pts',(-0.147085623620473,-0.0506130710337204,
1.5329511475679));
#17722=CARTESIAN_POINT('Ctrl Pts',(-0.147165890900045,-0.0503792039757457,
1.53293328192992));
#17723=CARTESIAN_POINT('Ctrl Pts',(-0.147330164328206,-0.0498968334491959,
1.5328965314027));
#17724=CARTESIAN_POINT('Ctrl Pts',(-0.147414099533037,-0.0496483088260831,
1.53287765115235));
#17725=CARTESIAN_POINT('Ctrl Pts',(-0.147611973517906,-0.0490574960146327,
1.53283289377293));
#17726=CARTESIAN_POINT('Ctrl Pts',(-0.147725351940766,-0.0487150186508342,
1.53280704956052));
#17727=CARTESIAN_POINT('Ctrl Pts',(-0.148100870838974,-0.0475673376954453,
1.53272076832629));
#17728=CARTESIAN_POINT('Ctrl Pts',(-0.148357633861336,-0.0467603691133015,
1.53266063688858));
#17729=CARTESIAN_POINT('Ctrl Pts',(-0.148956623168405,-0.0448232216206301,
1.53251747722622));
#17730=CARTESIAN_POINT('Ctrl Pts',(-0.149292601094478,-0.0436911460954515,
1.53243477581042));
#17731=CARTESIAN_POINT('Ctrl Pts',(-0.15354171451918,-0.0287521432711609,
1.53135468308444));
#17732=CARTESIAN_POINT('Ctrl Pts',(-0.155539138206286,-0.0144708830394118,
1.53044271801542));
#17733=CARTESIAN_POINT('Ctrl Pts',(-0.155549955824825,-0.000117230094128791,
1.52948519617329));
#17734=CARTESIAN_POINT('Ctrl Pts',(-0.155549955959819,-0.000117050836907798,
1.52948518421517));
#17735=CARTESIAN_POINT('Ctrl Pts',(-0.15555361652718,0.00474751149236398,
1.52916067267151));
#17736=CARTESIAN_POINT('Ctrl Pts',(-0.155329081858837,0.00960927334777459,
1.52883228170288));
#17737=CARTESIAN_POINT('Ctrl Pts',(-0.154667493090214,0.0166991392445401,
1.52834182545603));
#17738=CARTESIAN_POINT('Ctrl Pts',(-0.154408973841275,0.0189410288731022,
1.52818505108391));
#17739=CARTESIAN_POINT('Ctrl Pts',(-0.154002792797181,0.0218968289681659,
1.52797575505208));
#17740=CARTESIAN_POINT('Ctrl Pts',(-0.153898744482907,0.0226165364934278,
1.52792458944346));
#17741=CARTESIAN_POINT('Ctrl Pts',(-0.153713728409857,0.023835862659298,
1.52783754538967));
#17742=CARTESIAN_POINT('Ctrl Pts',(-0.153635360888999,0.0243358690817255,
1.5278017486645));
#17743=CARTESIAN_POINT('Ctrl Pts',(-0.153485598628029,0.0252618297821512,
1.52773526186373));
#17744=CARTESIAN_POINT('Ctrl Pts',(-0.153414867105046,0.0256878876989072,
1.52770459295538));
#17745=CARTESIAN_POINT('Ctrl Pts',(-0.153264775614349,0.0265692425148711,
1.52764098885568));
#17746=CARTESIAN_POINT('Ctrl Pts',(-0.153185159142653,0.0270244907796942,
1.52760804583765));
#17747=CARTESIAN_POINT('Ctrl Pts',(-0.152999854071414,0.0280569327466712,
1.52753312886163));
#17748=CARTESIAN_POINT('Ctrl Pts',(-0.152892926342534,0.0286338938670022,
1.52749111599814));
#17749=CARTESIAN_POINT('Ctrl Pts',(-0.152608376227765,0.0301222199511238,
1.52738235278711));
#17750=CARTESIAN_POINT('Ctrl Pts',(-0.152425855783712,0.0310326126635933,
1.52731544773114));
#17751=CARTESIAN_POINT('Ctrl Pts',(-0.151211072439986,0.0368223830296505,
1.52688749663444));
#17752=CARTESIAN_POINT('Ctrl Pts',(-0.149952909476299,0.0416508209832279,
1.52651930361146));
#17753=CARTESIAN_POINT('Ctrl Pts',(-0.147577486777783,0.0492497716186313,
1.52592093659929));
#17754=CARTESIAN_POINT('Ctrl Pts',(-0.14660854425104,0.0520633037270451,
1.5256951460568));
#17755=CARTESIAN_POINT('Ctrl Pts',(-0.141862381581549,0.0646591989635105,
1.52466587351159));
#17756=CARTESIAN_POINT('Ctrl Pts',(-0.137182830609302,0.0740716023997038,
1.52384325656873));
#17757=CARTESIAN_POINT('Ctrl Pts',(-0.129429928590226,0.0863721085416373,
1.52273207343837));
#17758=CARTESIAN_POINT('Ctrl Pts',(-0.127134049424308,0.0897172657392608,
1.52242607129844));
#17759=CARTESIAN_POINT('Ctrl Pts',(-0.124153766175856,0.0937150487894601,
1.52205895510559));
#17760=CARTESIAN_POINT('Ctrl Pts',(-0.123591023726735,0.0944559526629043,
1.52199085743058));
#17761=CARTESIAN_POINT('Ctrl Pts',(-0.122792336945533,0.0954881400845872,
1.52189595261002));
#17762=CARTESIAN_POINT('Ctrl Pts',(-0.122561951204366,0.095783667889189,
1.52186877616365));
#17763=CARTESIAN_POINT('Ctrl Pts',(-0.122166923059399,0.096286632207899,
1.52182252122679));
#17764=CARTESIAN_POINT('Ctrl Pts',(-0.122002815713996,0.0964944847846486,
1.52180340532849));
#17765=CARTESIAN_POINT('Ctrl Pts',(-0.121686676101729,0.096892800281814,
1.52176677277924));
#17766=CARTESIAN_POINT('Ctrl Pts',(-0.121534726782528,0.0970833254234786,
1.52174925026152));
#17767=CARTESIAN_POINT('Ctrl Pts',(-0.121130027613349,0.097588327612628,
1.5217028025437));
#17768=CARTESIAN_POINT('Ctrl Pts',(-0.120876498573878,0.0979021827039805,
1.52167393265855));
#17769=CARTESIAN_POINT('Ctrl Pts',(-0.119967470267349,0.0990185959212297,
1.52157121424968));
#17770=CARTESIAN_POINT('Ctrl Pts',(-0.119305156555559,0.0998156101702898,
1.52149783582755));
#17771=CARTESIAN_POINT('Ctrl Pts',(-0.11083595244985,0.109802524168907,
1.52057688839368));
#17772=CARTESIAN_POINT('Ctrl Pts',(-0.1019926628234,0.118062709094982,1.51979700344774));
#17773=CARTESIAN_POINT('Ctrl Pts',(-0.0867237757790628,0.129315376007072,
1.51854618159232));
#17774=CARTESIAN_POINT('Ctrl Pts',(-0.0808992164164632,0.133036773350022,
1.518087620436));
#17775=CARTESIAN_POINT('Ctrl Pts',(-0.0727567280229446,0.137506171537307,
1.5174533249823));
#17776=CARTESIAN_POINT('Ctrl Pts',(-0.070640345994748,0.138605300070893,
1.51728908493507));
#17777=CARTESIAN_POINT('Ctrl Pts',(-0.0674723434137778,0.140159175835041,
1.51704361012463));
#17778=CARTESIAN_POINT('Ctrl Pts',(-0.0664395570622591,0.140651686209092,
1.51696364300846));
#17779=CARTESIAN_POINT('Ctrl Pts',(-0.0648320825538602,0.141396596043321,
1.51683921847546));
#17780=CARTESIAN_POINT('Ctrl Pts',(-0.0642611292064625,0.141656992578138,
1.51679503233496));
#17781=CARTESIAN_POINT('Ctrl Pts',(-0.063688625831373,0.141913922642253,
1.51675072916146));
#17782=CARTESIAN_POINT('Ctrl Pts',(-0.0636886280167373,0.141913921661498,
1.50282608545586));
#17783=CARTESIAN_POINT('Ctrl Pts',(-0.069444972190622,0.139330569312872,
1.50324163634357));
#17784=CARTESIAN_POINT('Ctrl Pts',(-0.0750398294545228,0.136398920592801,
1.50365538729071));
#17785=CARTESIAN_POINT('Ctrl Pts',(-0.0858316222556287,0.129878352651127,
1.50449700233988));
#17786=CARTESIAN_POINT('Ctrl Pts',(-0.0910178110036122,0.126298046577962,
1.50492397268563));
#17787=CARTESIAN_POINT('Ctrl Pts',(-0.0971330857956377,0.121503668744037,
1.50546588059912));
#17788=CARTESIAN_POINT('Ctrl Pts',(-0.0982807663767021,0.120577230738902,
1.50556935458113));
#17789=CARTESIAN_POINT('Ctrl Pts',(-0.0999066632205765,0.11922612840304,
1.50571860750275));
#17790=CARTESIAN_POINT('Ctrl Pts',(-0.100395731115997,0.118814595910981,
1.50576385555925));
#17791=CARTESIAN_POINT('Ctrl Pts',(-0.101239754958756,0.118095449204696,
1.50584256726852));
#17792=CARTESIAN_POINT('Ctrl Pts',(-0.101595882549911,0.117789217448042,
1.50587597398802));
#17793=CARTESIAN_POINT('Ctrl Pts',(-0.102278347938201,0.11719697240293,
1.50594037297893));
#17794=CARTESIAN_POINT('Ctrl Pts',(-0.102604887052154,0.116911196826329,
1.50597135521098));
#17795=CARTESIAN_POINT('Ctrl Pts',(-0.10345800454188,0.116158251228628,
1.50605274816537));
#17796=CARTESIAN_POINT('Ctrl Pts',(-0.103982609688192,0.115688871048648,
1.50610325087151));
#17797=CARTESIAN_POINT('Ctrl Pts',(-0.105795760814115,0.114044293669446,
1.50627939666306));
#17798=CARTESIAN_POINT('Ctrl Pts',(-0.107067672047422,0.112851039281774,
1.50640580009945));
#17799=CARTESIAN_POINT('Ctrl Pts',(-0.116677511358743,0.103526774118044,
1.50738336605908));
#17800=CARTESIAN_POINT('Ctrl Pts',(-0.124096874798023,0.0945055082776629,
1.50827533962111));
#17801=CARTESIAN_POINT('Ctrl Pts',(-0.135465062304186,0.0770073141830383,
1.50989323292198));
#17802=CARTESIAN_POINT('Ctrl Pts',(-0.139793357834833,0.068838665034212,
1.51061081365883));
#17803=CARTESIAN_POINT('Ctrl Pts',(-0.143889194726233,0.0591056476709399,
1.5113931951411));
#17804=CARTESIAN_POINT('Ctrl Pts',(-0.144390242499144,0.0578708574297155,
1.51149115765783));
#17805=CARTESIAN_POINT('Ctrl Pts',(-0.145032258433162,0.0562283931100693,
1.51161961860247));
#17806=CARTESIAN_POINT('Ctrl Pts',(-0.145187467966838,0.0558264035680713,
1.51165091411164));
#17807=CARTESIAN_POINT('Ctrl Pts',(-0.145439545192993,0.0551653666251637,
1.51170213316269));
#17808=CARTESIAN_POINT('Ctrl Pts',(-0.145537394643253,0.0549067003613529,
1.51172211433182));
#17809=CARTESIAN_POINT('Ctrl Pts',(-0.145726583888102,0.0544025171063036,
1.51176094030336));
#17810=CARTESIAN_POINT('Ctrl Pts',(-0.145817993731529,0.0541570293206293,
1.51177978905553));
#17811=CARTESIAN_POINT('Ctrl Pts',(-0.146018138485127,0.0536153456280201,
1.51182125968183));
#17812=CARTESIAN_POINT('Ctrl Pts',(-0.146126593882742,0.0533190455508414,
1.51184386498518));
#17813=CARTESIAN_POINT('Ctrl Pts',(-0.146502906194542,0.0522811880439779,
1.51192277572943));
#17814=CARTESIAN_POINT('Ctrl Pts',(-0.146766032147455,0.0515379086126578,
1.51197880876514));
#17815=CARTESIAN_POINT('Ctrl Pts',(-0.147283986004412,0.050038648279442,
1.51209093085876));
#17816=CARTESIAN_POINT('Ctrl Pts',(-0.147538672438769,0.0492826445702359,
1.51214701110478));
#17817=CARTESIAN_POINT('Ctrl Pts',(-0.152918541545005,0.0328976348044611,
1.51335327493306));
#17818=CARTESIAN_POINT('Ctrl Pts',(-0.155539453720288,0.0165532974770953,
1.51438598880801));
#17819=CARTESIAN_POINT('Ctrl Pts',(-0.155553444498373,-0.00534049677197997,
1.51585984431451));
#17820=CARTESIAN_POINT('Ctrl Pts',(-0.155271557712048,-0.0107762398997825,
1.51623210021386));
#17821=CARTESIAN_POINT('Ctrl Pts',(-0.154606664813331,-0.0171314357059268,
1.51668011258868));
#17822=CARTESIAN_POINT('Ctrl Pts',(-0.15449903999975,-0.0180763232433023,
1.51674705151692));
#17823=CARTESIAN_POINT('Ctrl Pts',(-0.154310187101259,-0.0196092048191349,
1.51685620759762));
#17824=CARTESIAN_POINT('Ctrl Pts',(-0.154234244480277,-0.0201978357447761,
1.51689825867686));
#17825=CARTESIAN_POINT('Ctrl Pts',(-0.154093090948979,-0.0212446702859214,
1.51697328991365));
#17826=CARTESIAN_POINT('Ctrl Pts',(-0.154029199895858,-0.021703047360469,
1.51700622814368));
#17827=CARTESIAN_POINT('Ctrl Pts',(-0.153890355103112,-0.0226676642162984,
1.51707572496404));
#17828=CARTESIAN_POINT('Ctrl Pts',(-0.153814946926987,-0.0231738319033319,
1.51711229752432));
#17829=CARTESIAN_POINT('Ctrl Pts',(-0.153609121163664,-0.0245101309648115,
1.51720913354702));
#17830=CARTESIAN_POINT('Ctrl Pts',(-0.153474473709909,-0.0253395835127291,
1.51726952991206));
#17831=CARTESIAN_POINT('Ctrl Pts',(-0.152821097537498,-0.0291681002791789,
1.51754967649849));
#17832=CARTESIAN_POINT('Ctrl Pts',(-0.15222117140047,-0.0321524257371666,
1.51777197528291));
#17833=CARTESIAN_POINT('Ctrl Pts',(-0.148277860043631,-0.0491682716583368,
1.51906327028534));
#17834=CARTESIAN_POINT('Ctrl Pts',(-0.143083300910731,-0.0626964888878243,
1.52019305239524));
#17835=CARTESIAN_POINT('Ctrl Pts',(-0.135880080004464,-0.0757140516487397,
1.52133804497986));
#17836=CARTESIAN_POINT('Ctrl Pts',(-0.135655760700474,-0.0761152307567261,
1.52137338324612));
#17837=CARTESIAN_POINT('Ctrl Pts',(-0.134692032277317,-0.0778209971365417,
1.52152384288372));
#17838=CARTESIAN_POINT('Ctrl Pts',(-0.133935539062451,-0.0791158818654948,
1.52163857524532));
#17839=CARTESIAN_POINT('Ctrl Pts',(-0.131160395055023,-0.0837121619605214,
1.52204723064755));
#17840=CARTESIAN_POINT('Ctrl Pts',(-0.129037241460994,-0.08694924932166,
1.52233769971124));
#17841=CARTESIAN_POINT('Ctrl Pts',(-0.126429796501199,-0.0906184708903705,
1.5226672661327));
#17842=CARTESIAN_POINT('Ctrl Pts',(-0.126061125027223,-0.0911306397614478,
1.52271327554927));
#17843=CARTESIAN_POINT('Ctrl Pts',(-0.125498319491155,-0.0919025540052432,
1.5227826117621));
#17844=CARTESIAN_POINT('Ctrl Pts',(-0.125306479454328,-0.0921639508689246,
1.52280609021135));
#17845=CARTESIAN_POINT('Ctrl Pts',(-0.124960755326893,-0.0926319517778517,
1.52284812073254));
#17846=CARTESIAN_POINT('Ctrl Pts',(-0.124807174878304,-0.0928387740352898,
1.52286669323626));
#17847=CARTESIAN_POINT('Ctrl Pts',(-0.124472577915545,-0.093287035016655,
1.52290694234757));
#17848=CARTESIAN_POINT('Ctrl Pts',(-0.124291372940341,-0.0935283281790202,
1.52292860549018));
#17849=CARTESIAN_POINT('Ctrl Pts',(-0.123781108591073,-0.0942036960613757,
1.52298923756913));
#17850=CARTESIAN_POINT('Ctrl Pts',(-0.123450465241844,-0.0946365777641985,
1.52302809777984));
#17851=CARTESIAN_POINT('Ctrl Pts',(-0.121476589716869,-0.0971928472241987,
1.52325762300377));
#17852=CARTESIAN_POINT('Ctrl Pts',(-0.119780748903356,-0.0992753037702003,
1.52344479717875));
#17853=CARTESIAN_POINT('Ctrl Pts',(-0.10849835884994,-0.112419521216316,
1.52463531288907));
#17854=CARTESIAN_POINT('Ctrl Pts',(-0.0974443086764656,-0.122125975980344,
1.52556355617038));
#17855=CARTESIAN_POINT('Ctrl Pts',(-0.0835241903286924,-0.131238332286373,
1.52668150667753));
#17856=CARTESIAN_POINT('Ctrl Pts',(-0.081832556840949,-0.132299744509495,
1.52681647728102));
#17857=CARTESIAN_POINT('Ctrl Pts',(-0.0767637363690003,-0.135345752809189,
1.52721910217065));
#17858=CARTESIAN_POINT('Ctrl Pts',(-0.0733317325616018,-0.137235551443579,
1.52748943807872));
#17859=CARTESIAN_POINT('Ctrl Pts',(-0.0689876956504054,-0.139418054031481,
1.52783078086008));
#17860=CARTESIAN_POINT('Ctrl Pts',(-0.0681392487230121,-0.139834683302201,
1.52789740828192));
#17861=CARTESIAN_POINT('Ctrl Pts',(-0.066799672897471,-0.140477394785457,
1.52800256433278));
#17862=CARTESIAN_POINT('Ctrl Pts',(-0.0663110618788404,-0.140708698394978,
1.5280409119228));
#17863=CARTESIAN_POINT('Ctrl Pts',(-0.0654464972878158,-0.141112471360968,
1.52810875587328));
#17864=CARTESIAN_POINT('Ctrl Pts',(-0.0650710407117796,-0.141285998016322,
1.52813821546646));
#17865=CARTESIAN_POINT('Ctrl Pts',(-0.0642094402273372,-0.141680045349909,
1.52820581487852));
#17866=CARTESIAN_POINT('Ctrl Pts',(-0.0637228466240425,-0.141899564022123,
1.52824398863043));
#17867=CARTESIAN_POINT('Ctrl Pts',(-0.0623760520317323,-0.142498823781674,
1.52834964274461));
#17868=CARTESIAN_POINT('Ctrl Pts',(-0.0615135353915239,-0.142873270900201,
1.52841730241486));
#17869=CARTESIAN_POINT('Ctrl Pts',(-0.0566509017817775,-0.144932107739253,
1.52879878717056));
#17870=CARTESIAN_POINT('Ctrl Pts',(-0.0525854398684352,-0.146456154268644,
1.52911795621707));
#17871=CARTESIAN_POINT('Ctrl Pts',(-0.0395687427654616,-0.150723946323055,
1.53014180490559));
#17872=CARTESIAN_POINT('Ctrl Pts',(-0.0304316585136157,-0.152830831413686,
1.53086469320528));
#17873=CARTESIAN_POINT('Ctrl Pts',(-0.020797883252986,-0.154153772759252,
1.53161883178106));
#17874=CARTESIAN_POINT('Ctrl Pts',(-0.0204335598364272,-0.154202487776322,
1.53164733682165));
#17875=CARTESIAN_POINT('Ctrl Pts',(-0.0111912446707548,-0.155404982102844,
1.5323700644299));
#17876=CARTESIAN_POINT('Ctrl Pts',(-0.00222902233224552,-0.1557916158411,
1.53306260286976));
#17877=CARTESIAN_POINT('Ctrl Pts',(0.00740435802095051,-0.155375192187848,
1.53376928677472));
#17878=CARTESIAN_POINT('Ctrl Pts',(0.00809081799741246,-0.155340959107295,
1.53381943165361));
#17879=CARTESIAN_POINT('Ctrl Pts',(0.00910781764832401,-0.155283482435782,
1.53389338544108));
#17880=CARTESIAN_POINT('Ctrl Pts',(0.00943853346218654,-0.155263731603161,
1.53391738152706));
#17881=CARTESIAN_POINT('Ctrl Pts',(0.0100268667346512,-0.155226708735474,
1.53395997294424));
#17882=CARTESIAN_POINT('Ctrl Pts',(0.0102845060329824,-0.155209851816248,
1.53397859109114));
#17883=CARTESIAN_POINT('Ctrl Pts',(0.010838168354797,-0.15517224192069,
1.53401852919249));
#17884=CARTESIAN_POINT('Ctrl Pts',(0.0111341735715102,-0.15515128339423,
1.53403983748106));
#17885=CARTESIAN_POINT('Ctrl Pts',(0.0119505053287088,-0.155091135120756,
1.53409848558904));
#17886=CARTESIAN_POINT('Ctrl Pts',(0.0124707040401007,-0.155050173596458,
1.53413572785112));
#17887=CARTESIAN_POINT('Ctrl Pts',(0.0153079241649146,-0.154812393608124,
1.53433818697536));
#17888=CARTESIAN_POINT('Ctrl Pts',(0.0176206745639658,-0.154566241950804,
1.53450080302301));
#17889=CARTESIAN_POINT('Ctrl Pts',(0.0342238390238381,-0.152421572197943,
1.53565645592005));
#17890=CARTESIAN_POINT('Ctrl Pts',(0.0481959687578782,-0.148596326319939,
1.53657171804269));
#17891=CARTESIAN_POINT('Ctrl Pts',(0.0641985574908062,-0.141715723954383,
1.53773801530244));
#17892=CARTESIAN_POINT('Ctrl Pts',(0.0669194130766444,-0.140451385815345,
1.53794050088983));
#17893=CARTESIAN_POINT('Ctrl Pts',(0.069708249892309,-0.13905601942523,
1.53815340403113));
#17894=CARTESIAN_POINT('Ctrl Pts',(0.069814537463293,-0.139002687024802,
1.53816152634118));
#17895=CARTESIAN_POINT('Ctrl Pts',(0.0702831661230713,-0.138766867991926,
1.53819737449482));
#17896=CARTESIAN_POINT('Ctrl Pts',(0.0706448512547139,-0.138583087276658,
1.538225137932));
#17897=CARTESIAN_POINT('Ctrl Pts',(0.0737972682836353,-0.136965722164754,
1.53846797897592));
#17898=CARTESIAN_POINT('Ctrl Pts',(0.0765445746188577,-0.135449516746621,
1.5386855169345));
#17899=CARTESIAN_POINT('Ctrl Pts',(0.0800068983158047,-0.133399717839762,
1.53896833123945));
#17900=CARTESIAN_POINT('Ctrl Pts',(0.0807659013304027,-0.132941557166834,
1.53903087636554));
#17901=CARTESIAN_POINT('Ctrl Pts',(0.0819655073193224,-0.132203368334583,
1.53913062378229));
#17902=CARTESIAN_POINT('Ctrl Pts',(0.082408697213326,-0.131927561944565,
1.539167671321));
#17903=CARTESIAN_POINT('Ctrl Pts',(0.0832016193457557,-0.131428555361072,
1.53923431160548));
#17904=CARTESIAN_POINT('Ctrl Pts',(0.0835518644830371,-0.131206175774389,
1.53926387384011));
#17905=CARTESIAN_POINT('Ctrl Pts',(0.0843684200379183,-0.130683128391871,
1.53933309319188));
#17906=CARTESIAN_POINT('Ctrl Pts',(0.0848340171459703,-0.130381363185524,
1.53937279080153));
#17907=CARTESIAN_POINT('Ctrl Pts',(0.0861659216132569,-0.129507967703471,
1.53948701781686));
#17908=CARTESIAN_POINT('Ctrl Pts',(0.0870281206490416,-0.128930158866643,
1.53956177747625));
#17909=CARTESIAN_POINT('Ctrl Pts',(0.0931353516324097,-0.124748182397607,
1.54009727450012));
#17910=CARTESIAN_POINT('Ctrl Pts',(0.0981598706743632,-0.120834272545009,
1.54056980284225));
#17911=CARTESIAN_POINT('Ctrl Pts',(0.111562080883876,-0.109005767817966,
1.5419250403268));
#17912=CARTESIAN_POINT('Ctrl Pts',(0.119321292594309,-0.100452684296784,
1.54282864467559));
#17913=CARTESIAN_POINT('Ctrl Pts',(0.126743056985038,-0.0901850353215221,
1.54380000538621));
#17914=CARTESIAN_POINT('Ctrl Pts',(0.127410851236553,-0.0892391068311109,
1.54388850193799));
#17915=CARTESIAN_POINT('Ctrl Pts',(0.130277074632733,-0.0850813415508628,
1.54427293294728));
#17916=CARTESIAN_POINT('Ctrl Pts',(0.132365310144968,-0.0817947551773177,
1.54456514531427));
#17917=CARTESIAN_POINT('Ctrl Pts',(0.13464686993893,-0.0778872405679721,
1.54489643957362));
#17918=CARTESIAN_POINT('Ctrl Pts',(0.134962183732542,-0.0773395812411422,
1.54494251417033));
#17919=CARTESIAN_POINT('Ctrl Pts',(0.135434316361647,-0.0765078669353528,
1.54501192901333));
#17920=CARTESIAN_POINT('Ctrl Pts',(0.135593593250301,-0.0762252269661567,
1.54503542141711));
#17921=CARTESIAN_POINT('Ctrl Pts',(0.13587776159334,-0.0757172554511573,
1.54507746686208));
#17922=CARTESIAN_POINT('Ctrl Pts',(0.13600297794591,-0.0754921112565072,
1.54509604039955));
#17923=CARTESIAN_POINT('Ctrl Pts',(0.136273578065135,-0.0750027025446985,
1.54513628022747));
#17924=CARTESIAN_POINT('Ctrl Pts',(0.136418752363205,-0.0747383266842448,
1.54515793310422));
#17925=CARTESIAN_POINT('Ctrl Pts',(0.136823627343831,-0.0739959017149442,
1.54521850751742));
#17926=CARTESIAN_POINT('Ctrl Pts',(0.137081593907283,-0.0735169035363521,
1.54525732066058));
#17927=CARTESIAN_POINT('Ctrl Pts',(0.138592393976546,-0.0706760134066091,
1.54548599512565));
#17928=CARTESIAN_POINT('Ctrl Pts',(0.13978677568173,-0.0682833083686396,
1.54567239570051));
#17929=CARTESIAN_POINT('Ctrl Pts',(0.147120079079251,-0.0525926184865806,
1.54686289783887));
#17930=CARTESIAN_POINT('Ctrl Pts',(0.151416910879703,-0.0385139647951244,
1.54779165672244));
#17931=CARTESIAN_POINT('Ctrl Pts',(0.153987358873573,-0.0220822312958419,
1.54890918710999));
#17932=CARTESIAN_POINT('Ctrl Pts',(0.154256241516254,-0.0201182285771598,
1.54904315331504));
#17933=CARTESIAN_POINT('Ctrl Pts',(0.15494641234157,-0.0142435921607052,
1.54944582064566));
#17934=CARTESIAN_POINT('Ctrl Pts',(0.155256968029684,-0.0103218214161604,
1.54971724428619));
#17935=CARTESIAN_POINT('Ctrl Pts',(0.155457480032245,-0.0054470448734784,
1.55005980348155));
#17936=CARTESIAN_POINT('Ctrl Pts',(0.155487746234464,-0.00450101057047012,
1.55012652140976));
#17937=CARTESIAN_POINT('Ctrl Pts',(0.155521737129451,-0.00301402491509948,
1.55023178937231));
#17938=CARTESIAN_POINT('Ctrl Pts',(0.155531277385485,-0.00247321801681153,
1.55027015772737));
#17939=CARTESIAN_POINT('Ctrl Pts',(0.155543134947022,-0.00151879767110524,
1.55033802189473));
#17940=CARTESIAN_POINT('Ctrl Pts',(0.155546623552833,-0.00110520168523168,
1.55036748084161));
#17941=CARTESIAN_POINT('Ctrl Pts',(0.155550834700325,-0.000158068670969605,
1.55043505910856));
#17942=CARTESIAN_POINT('Ctrl Pts',(0.155550461825959,0.000375465450121448,
1.55047321227224));
#17943=CARTESIAN_POINT('Ctrl Pts',(0.155541856941821,0.00184795701881281,
1.55057875205052));
#17944=CARTESIAN_POINT('Ctrl Pts',(0.155527867702242,0.00278684448913933,
1.55064631733326));
#17945=CARTESIAN_POINT('Ctrl Pts',(0.155401918969186,0.0080440055154591,
1.55102621526338));
#17946=CARTESIAN_POINT('Ctrl Pts',(0.155118626540416,0.0123558618895632,
1.55134383952312));
#17947=CARTESIAN_POINT('Ctrl Pts',(0.153663197767928,0.0258748777886286,
1.55235994877738));
#17948=CARTESIAN_POINT('Ctrl Pts',(0.151846816500051,0.0349912598644559,
1.55307629706358));
#17949=CARTESIAN_POINT('Ctrl Pts',(0.146766439254243,0.0522648696525828,
1.55447266127039));
#17950=CARTESIAN_POINT('Ctrl Pts',(0.143602462384224,0.060418307932727,
1.55514954786331));
#17951=CARTESIAN_POINT('Ctrl Pts',(0.139260916542254,0.0693076386202358,
1.55588090862892));
#17952=CARTESIAN_POINT('Ctrl Pts',(0.138739478815335,0.070345638683965,
1.55596618557241));
#17953=CARTESIAN_POINT('Ctrl Pts',(0.138012428955761,0.0717534021209866,
1.55608157571296));
#17954=CARTESIAN_POINT('Ctrl Pts',(0.137816882122592,0.0721282765326171,
1.55611227716316));
#17955=CARTESIAN_POINT('Ctrl Pts',(0.137504487899386,0.0727212453058917,
1.55616079354087));
#17956=CARTESIAN_POINT('Ctrl Pts',(0.137388646498821,0.0729398623996804,
1.55617867059255));
#17957=CARTESIAN_POINT('Ctrl Pts',(0.137149016359225,0.0733894985907175,
1.55621541664127));
#17958=CARTESIAN_POINT('Ctrl Pts',(0.137025165344152,0.0736204812215321,
1.5562342810999));
#17959=CARTESIAN_POINT('Ctrl Pts',(0.136729901106469,0.0741678239361704,
1.55627895575397));
#17960=CARTESIAN_POINT('Ctrl Pts',(0.136557971456493,0.0744839070050875,
1.55630473332968));
#17961=CARTESIAN_POINT('Ctrl Pts',(0.135980166110081,0.0755374442698578,
1.55639059069942));
#17962=CARTESIAN_POINT('Ctrl Pts',(0.135569391641532,0.0762722177235443,
1.5564503689208));
#17963=CARTESIAN_POINT('Ctrl Pts',(0.131580832986118,0.0832727218406192,
1.55701928367226));
#17964=CARTESIAN_POINT('Ctrl Pts',(0.127576570210791,0.0892866858644213,
1.5575034343084));
#17965=CARTESIAN_POINT('Ctrl Pts',(0.119931106816773,0.0991989453113594,
1.55833258742462));
#17966=CARTESIAN_POINT('Ctrl Pts',(0.116481183418192,0.103228079688648,
1.55867982116881));
#17967=CARTESIAN_POINT('Ctrl Pts',(0.106013084429045,0.114259212070549,
1.55968306451265));
#17968=CARTESIAN_POINT('Ctrl Pts',(0.0985241911643273,0.120776154013316,
1.56034437423262));
#17969=CARTESIAN_POINT('Ctrl Pts',(0.089538363528991,0.127200582193882,
1.56111779693658));
#17970=CARTESIAN_POINT('Ctrl Pts',(0.0886021124757208,0.127854496188725,
1.56119813186994));
#17971=CARTESIAN_POINT('Ctrl Pts',(0.0871761870278595,0.128827233831791,
1.56132015382112));
#17972=CARTESIAN_POINT('Ctrl Pts',(0.0866917615519426,0.129153715485122,
1.56136155129668));
#17973=CARTESIAN_POINT('Ctrl Pts',(0.085821161334806,0.129733357235402,
1.5614358551832));
#17974=CARTESIAN_POINT('Ctrl Pts',(0.0854356745157989,0.129987542572472,
1.56146872268003));
#17975=CARTESIAN_POINT('Ctrl Pts',(0.0850481166150463,0.130240624850765,
1.56150173537069));
#17976=CARTESIAN_POINT('Ctrl Pts',(0.0850471677999097,0.130241244429319,
1.56150181619182));
#17977=CARTESIAN_POINT('Ctrl Pts',(0.0850452782299925,0.130242478293549,
1.56150197714712));
#17978=CARTESIAN_POINT('Ctrl Pts',(0.0850443373587732,0.130243092655502,
1.5615020572912));
#17979=CARTESIAN_POINT('Ctrl Pts',(0.0850424634429056,0.130244316239917,
1.56150221691234));
#17980=CARTESIAN_POINT('Ctrl Pts',(0.0850415304015873,0.130244925460447,
1.5615022963891));
#17981=CARTESIAN_POINT('Ctrl Pts',(0.0850396720898532,0.130246138799087,
1.56150245468034));
#17982=CARTESIAN_POINT('Ctrl Pts',(0.0850387468118492,0.130246742922389,
1.56150253349547));
#17983=CARTESIAN_POINT('Ctrl Pts',(0.0850369039616087,0.130247946109813,
1.56150269046898));
#17984=CARTESIAN_POINT('Ctrl Pts',(0.085035986380576,0.13024854517991,1.56150276862813));
#17985=CARTESIAN_POINT('Ctrl Pts',(0.0850341588439292,0.130249738314079,
1.56150292429654));
#17986=CARTESIAN_POINT('Ctrl Pts',(0.0850332488867652,0.130250332379392,
1.56150300180593));
#17987=CARTESIAN_POINT('Ctrl Pts',(0.0850314365403697,0.130251515542208,
1.56150315617976));
#17988=CARTESIAN_POINT('Ctrl Pts',(0.0850305341430547,0.130252104645214,
1.56150323304487));
#17989=CARTESIAN_POINT('Ctrl Pts',(0.0850289355560498,0.130253148211074,
1.56150336921029));
#17990=CARTESIAN_POINT('Ctrl Pts',(0.0850282393656419,0.130253602679813,
1.56150342851071));
#17991=CARTESIAN_POINT('Ctrl Pts',(0.0850268481085561,0.130254510867813,
1.56150354701565));
#17992=CARTESIAN_POINT('Ctrl Pts',(0.0850261532053007,0.130254964480427,
1.56150360620624));
#17993=CARTESIAN_POINT('Ctrl Pts',(0.0850247647277499,0.130255870822304,
1.56150372447402));
#17994=CARTESIAN_POINT('Ctrl Pts',(0.0850240711573939,0.130256323549025,
1.56150378355087));
#17995=CARTESIAN_POINT('Ctrl Pts',(0.0850226853581879,0.130257228111018,
1.56150390159011));
#17996=CARTESIAN_POINT('Ctrl Pts',(0.085021993122497,0.130257679950786,
1.56150396055308));
#17997=CARTESIAN_POINT('Ctrl Pts',(0.0850206099815398,0.130258582746196,
1.56150407836549));
#17998=CARTESIAN_POINT('Ctrl Pts',(0.0850199190752802,0.130259033702517,
1.56150413721503));
#17999=CARTESIAN_POINT('Ctrl Pts',(0.0850185385898779,0.130259934733284,
1.56150425480085));
#18000=CARTESIAN_POINT('Ctrl Pts',(0.0850178490111873,0.130260384807466,
1.56150431353711));
#18001=CARTESIAN_POINT('Ctrl Pts',(0.0850164711629671,0.130261284085763,
1.56150443089791));
#18002=CARTESIAN_POINT('Ctrl Pts',(0.0850157829010244,0.130261733284957,
1.56150448952181));
#18003=CARTESIAN_POINT('Ctrl Pts',(0.0850144077030382,0.130262630802446,
1.56150460665647));
#18004=CARTESIAN_POINT('Ctrl Pts',(0.0850137207604828,0.130263079125021,
1.5615046651678));
#18005=CARTESIAN_POINT('Ctrl Pts',(0.0850123481892908,0.13026397489718,
1.56150478207833));
#18006=CARTESIAN_POINT('Ctrl Pts',(0.0850116625591765,0.130264422347757,
1.56150484047767));
#18007=CARTESIAN_POINT('Ctrl Pts',(0.0850102926156679,0.130265316374184,
1.56150495716399));
#18008=CARTESIAN_POINT('Ctrl Pts',(0.0850096082961706,0.130265762954044,
1.5615050154515));
#18009=CARTESIAN_POINT('Ctrl Pts',(0.0850082409734261,0.130266655239432,
1.56150513191421));
#18010=CARTESIAN_POINT('Ctrl Pts',(0.0850075579651311,0.130267100948282,
1.56150519008984));
#18011=CARTESIAN_POINT('Ctrl Pts',(0.085006193239945,0.130267991507951,
1.56150530633091));
#18012=CARTESIAN_POINT('Ctrl Pts',(0.0850055115319338,0.130268436353005,
1.56150536439559));
#18013=CARTESIAN_POINT('Ctrl Pts',(0.0850041494113009,0.130269325182566,
1.56150548041443));
#18014=CARTESIAN_POINT('Ctrl Pts',(0.0850034689998191,0.13026976916636,
1.56150553836849));
#18015=CARTESIAN_POINT('Ctrl Pts',(0.0850021094819115,0.130270656267183,
1.56150565416526));
#18016=CARTESIAN_POINT('Ctrl Pts',(0.0850014303686737,0.130271099388686,
1.56150571200855));
#18017=CARTESIAN_POINT('Ctrl Pts',(0.0850000734329893,0.130271984774323,
1.56150582758499));
#18018=CARTESIAN_POINT('Ctrl Pts',(0.0849993956119666,0.130272427037556,
1.56150588531802));
#18019=CARTESIAN_POINT('Ctrl Pts',(0.0849980412531082,0.130273310711701,
1.5615060006746));
#18020=CARTESIAN_POINT('Ctrl Pts',(0.0849973647178349,0.13027375212097,
1.56150605829793));
#18021=CARTESIAN_POINT('Ctrl Pts',(0.0849960129377777,0.130274634082507,
1.56150617343448));
#18022=CARTESIAN_POINT('Ctrl Pts',(0.0849953376882651,0.13027507463789,
1.5615062309481));
#18023=CARTESIAN_POINT('Ctrl Pts',(0.0849939884714945,0.130275954897114,
1.56150634586595));
#18024=CARTESIAN_POINT('Ctrl Pts',(0.0849933145031967,0.130276394601663,
1.56150640327026));
#18025=CARTESIAN_POINT('Ctrl Pts',(0.0849919678425465,0.130277273163421,
1.56150651797001));
#18026=CARTESIAN_POINT('Ctrl Pts',(0.0849912951501145,0.13027771202071,
1.56150657526546));
#18027=CARTESIAN_POINT('Ctrl Pts',(0.0849899510453231,0.130278588885343,
1.56150668974715));
#18028=CARTESIAN_POINT('Ctrl Pts',(0.0849892796286742,0.130279026895512,
1.56150674693375));
#18029=CARTESIAN_POINT('Ctrl Pts',(0.0849879380621388,0.130279902074672,
1.56150686119886));
#18030=CARTESIAN_POINT('Ctrl Pts',(0.0849872679143556,0.130280339242319,
1.5615069182772));
#18031=CARTESIAN_POINT('Ctrl Pts',(0.0849859288870869,0.130281212735516,
1.56150703232567));
#18032=CARTESIAN_POINT('Ctrl Pts',(0.0849852600061635,0.130281649062032,
1.56150708929592));
#18033=CARTESIAN_POINT('Ctrl Pts',(0.0849839235058335,0.130282520877476,
1.56150720312879));
#18034=CARTESIAN_POINT('Ctrl Pts',(0.0849832558862233,0.130282956366564,
1.56150725999143));
#18035=CARTESIAN_POINT('Ctrl Pts',(0.084981921914536,0.13028382650331,1.56150737360856));
#18036=CARTESIAN_POINT('Ctrl Pts',(0.0849812555576062,0.130284261154161,
1.56150743036346));
#18037=CARTESIAN_POINT('Ctrl Pts',(0.0849799240902541,0.130285129628232,
1.56150754376692));
#18038=CARTESIAN_POINT('Ctrl Pts',(0.0849792589851656,0.130285563447999,
1.56150760041502));
#18039=CARTESIAN_POINT('Ctrl Pts',(0.0849779300375986,0.130286430249482,
1.5615077136035));
#18040=CARTESIAN_POINT('Ctrl Pts',(0.0849772661888218,0.130286863235332,
1.56150777014441));
#18041=CARTESIAN_POINT('Ctrl Pts',(0.0849759397301668,0.130287728384529,
1.56150788312054));
#18042=CARTESIAN_POINT('Ctrl Pts',(0.0849752771264454,0.130288160543886,
1.56150793955522));
#18043=CARTESIAN_POINT('Ctrl Pts',(0.0849739531671769,0.130289024034129,
1.56150805231811));
#18044=CARTESIAN_POINT('Ctrl Pts',(0.0849732918071016,0.130289455367994,
1.56150810864669));
#18045=CARTESIAN_POINT('Ctrl Pts',(0.0845396412154296,0.130572274183848,
1.56154504296552));
#18046=CARTESIAN_POINT('Ctrl Pts',(0.0841052518826073,0.130852498318634,
1.56158200121162));
#18047=CARTESIAN_POINT('Ctrl Pts',(0.082927807262822,0.131603781511331,
1.56168207970147));
#18048=CARTESIAN_POINT('Ctrl Pts',(0.0821821488629356,0.132070704074363,
1.56174535160851));
#18049=CARTESIAN_POINT('Ctrl Pts',(0.0805253933788353,0.13308868181175,
1.5618857186583));
#18050=CARTESIAN_POINT('Ctrl Pts',(0.0796125251914252,0.133636753675993,
1.56196291900752));
#18051=CARTESIAN_POINT('Ctrl Pts',(0.0768328353601118,0.135267046982856,
1.5621976046397));
#18052=CARTESIAN_POINT('Ctrl Pts',(0.0749491242085214,0.136319795022483,
1.56235612186252));
#18053=CARTESIAN_POINT('Ctrl Pts',(0.0599444478031621,0.144300432763399,
1.56361513618728));
#18054=CARTESIAN_POINT('Ctrl Pts',(0.0459164366917163,0.149356840055325,
1.56478118003828));
#18055=CARTESIAN_POINT('Ctrl Pts',(0.0301810729871011,0.152598913166574,
1.5660135910902));
#18056=CARTESIAN_POINT('Ctrl Pts',(0.0289694288724993,0.15283356238019,
1.5661079505423));
#18057=CARTESIAN_POINT('Ctrl Pts',(0.0239086094199343,0.153751302093287,
1.56649954020732));
#18058=CARTESIAN_POINT('Ctrl Pts',(0.0200367682716553,0.154303658225789,
1.56679307317728));
#18059=CARTESIAN_POINT('Ctrl Pts',(0.0155186683575466,0.154775235751206,
1.56712567569115));
#18060=CARTESIAN_POINT('Ctrl Pts',(0.0148890874526731,0.15483706849828,
1.567171799314));
#18061=CARTESIAN_POINT('Ctrl Pts',(0.0139359312257882,0.154924812942091,
1.56724127329328));
#18062=CARTESIAN_POINT('Ctrl Pts',(0.0136126336331707,0.154953554509322,
1.56726477618714));
#18063=CARTESIAN_POINT('Ctrl Pts',(0.0130325554285475,0.155003294715676,
1.56730683285849));
#18064=CARTESIAN_POINT('Ctrl Pts',(0.0127758117812956,0.155024667425858,
1.56732540718076));
#18065=CARTESIAN_POINT('Ctrl Pts',(0.0122184880154698,0.155069668061854,
1.56736564006512));
#18066=CARTESIAN_POINT('Ctrl Pts',(0.0119178927641437,0.155093059930054,
1.56738728525196));
#18067=CARTESIAN_POINT('Ctrl Pts',(0.0110752135637488,0.155156171556046,
1.56744781648038));
#18068=CARTESIAN_POINT('Ctrl Pts',(0.0105329793624024,0.155193924806041,
1.56748659437724));
#18069=CARTESIAN_POINT('Ctrl Pts',(0.00733093561575968,0.155400008749324,
1.56771463446037));
#18070=CARTESIAN_POINT('Ctrl Pts',(0.00466714645000089,0.155502814694375,
1.5679004582478));
#18071=CARTESIAN_POINT('Ctrl Pts',(-0.0126493454488499,0.15572568448945,
1.56909095213178));
#18072=CARTESIAN_POINT('Ctrl Pts',(-0.0272550133597357,0.153843311786539,
1.57002009679163));
#18073=CARTESIAN_POINT('Ctrl Pts',(-0.0432831259387198,0.149419743499892,
1.57113732443984));
#18074=CARTESIAN_POINT('Ctrl Pts',(-0.0451732350353517,0.148859219126361,
1.57127055077436));
#18075=CARTESIAN_POINT('Ctrl Pts',(-0.0508121737982156,0.147069668340408,
1.57167325060518));
#18076=CARTESIAN_POINT('Ctrl Pts',(-0.0545251612263234,0.145733889712186,
1.57194547669648));
#18077=CARTESIAN_POINT('Ctrl Pts',(-0.0590618147930818,0.143904142525083,
1.57228893315267));
#18078=CARTESIAN_POINT('Ctrl Pts',(-0.0599372348335434,0.143541729166917,
1.57235571761362));
#18079=CARTESIAN_POINT('Ctrl Pts',(-0.0613073225914843,0.142959810781406,
1.57246106784065));
#18080=CARTESIAN_POINT('Ctrl Pts',(-0.0618042597800819,0.142745678609127,
1.57249945145615));
#18081=CARTESIAN_POINT('Ctrl Pts',(-0.0626790491542835,0.142363304151395,
1.5725673304979));
#18082=CARTESIAN_POINT('Ctrl Pts',(-0.0630573687742955,0.142196138516448,
1.57259678898663));
#18083=CARTESIAN_POINT('Ctrl Pts',(-0.0634381286191023,0.14202607629919,
1.57262654252104));
#18084=CARTESIAN_POINT('Ctrl Pts',(-0.0634412433382933,0.142024685020998,
1.57262678592017));
#18085=CARTESIAN_POINT('Ctrl Pts',(-0.0634473630981949,0.142021951214305,
1.57262726416154));
#18086=CARTESIAN_POINT('Ctrl Pts',(-0.0634503691532165,0.142020608241029,
1.57262749908257));
#18087=CARTESIAN_POINT('Ctrl Pts',(-0.0634562764064302,0.142017968914926,
1.57262796074315));
#18088=CARTESIAN_POINT('Ctrl Pts',(-0.0634591776953348,0.142016672529454,
1.57262818748932));
#18089=CARTESIAN_POINT('Ctrl Pts',(-0.0634648813406012,0.142014123754777,
1.57262863326187));
#18090=CARTESIAN_POINT('Ctrl Pts',(-0.0634676825240292,0.142012871897032,
1.57262885219614));
#18091=CARTESIAN_POINT('Ctrl Pts',(-0.0634731880889014,0.142010411247224,
1.57262928251015));
#18092=CARTESIAN_POINT('Ctrl Pts',(-0.0634758924728102,0.142009202460809,
1.57262949388969));
#18093=CARTESIAN_POINT('Ctrl Pts',(-0.0635486298516659,0.141976688328124,
1.57263517931892));
#18094=CARTESIAN_POINT('Ctrl Pts',(-0.0636186395413799,0.141945331333901,
1.5726406551333));
#18095=CARTESIAN_POINT('Ctrl Pts',(-0.0636886258330468,0.141913922641502,
1.57264613271722));
#18096=CARTESIAN_POINT('Origin',(0.,0.,-0.129405622560373));
#18097=CARTESIAN_POINT('',(-0.0636886255459746,0.141913922770335,1.65651328069486));
#18098=CARTESIAN_POINT('',(-0.0636886598674488,0.141913907367419,1.64281642759095));
#18099=CARTESIAN_POINT('',(-0.0636886258329924,0.141913922641526,-0.129405622560373));
#18100=CARTESIAN_POINT('Ctrl Pts',(-0.0636886255459746,0.141913922770335,
1.65651328069486));
#18101=CARTESIAN_POINT('Ctrl Pts',(-0.0608990448660293,0.143165840523626,
1.65627904268153));
#18102=CARTESIAN_POINT('Ctrl Pts',(-0.0580727927935074,0.144335398020984,
1.65604680844661));
#18103=CARTESIAN_POINT('Ctrl Pts',(-0.0532792558894189,0.146155411082134,
1.65566325401286));
#18104=CARTESIAN_POINT('Ctrl Pts',(-0.0513303839785977,0.146851203993629,
1.65551010689714));
#18105=CARTESIAN_POINT('Ctrl Pts',(-0.048892337343171,0.147667171491005,
1.6553224457726));
#18106=CARTESIAN_POINT('Ctrl Pts',(-0.0484158141915759,0.147824095268433,
1.65528595146716));
#18107=CARTESIAN_POINT('Ctrl Pts',(-0.0476582378689306,0.14806951635225,
1.65522823447466));
#18108=CARTESIAN_POINT('Ctrl Pts',(-0.0473776837606538,0.148159523470421,
1.65520692551255));
#18109=CARTESIAN_POINT('Ctrl Pts',(-0.0468503818960722,0.148327041047081,
1.65516700025293));
#18110=CARTESIAN_POINT('Ctrl Pts',(-0.046603699570519,0.14840473232819,
1.65514837392804));
#18111=CARTESIAN_POINT('Ctrl Pts',(-0.0460371625309225,0.148581608235836,
1.65510571294197));
#18112=CARTESIAN_POINT('Ctrl Pts',(-0.045717180761911,0.14868037539884,
1.65508170286278));
#18113=CARTESIAN_POINT('Ctrl Pts',(-0.0448758194306769,0.148937101191185,
1.65501878744189));
#18114=CARTESIAN_POINT('Ctrl Pts',(-0.0443539184682187,0.149093357399847,
1.65497997884451));
#18115=CARTESIAN_POINT('Ctrl Pts',(-0.0407948483387557,0.150138594078206,
1.65471674004791));
#18116=CARTESIAN_POINT('Ctrl Pts',(-0.0377317114262756,0.150937532491612,
1.65449717498095));
#18117=CARTESIAN_POINT('Ctrl Pts',(-0.0331615458721655,0.151981687012985,
1.65417692292831));
#18118=CARTESIAN_POINT('Ctrl Pts',(-0.031672086360532,0.152299049725731,
1.65407368844555));
#18119=CARTESIAN_POINT('Ctrl Pts',(-0.0289650801959153,0.152834406306263,
1.65388773220125));
#18120=CARTESIAN_POINT('Ctrl Pts',(-0.0277491570929766,0.153059844579423,
1.6538048096822));
#18121=CARTESIAN_POINT('Ctrl Pts',(-0.0123393781655351,0.155727225291964,
1.65276011155914));
#18122=CARTESIAN_POINT('Ctrl Pts',(0.00212350071491233,0.156200920876923,
1.65183866873016));
#18123=CARTESIAN_POINT('Ctrl Pts',(0.0184314283601973,0.154467064384953,
1.65071291298783));
#18124=CARTESIAN_POINT('Ctrl Pts',(0.0204131604714797,0.154217683190534,
1.65057478364117));
#18125=CARTESIAN_POINT('Ctrl Pts',(0.0238302356705591,0.153720662540302,
1.6503339576218));
#18126=CARTESIAN_POINT('Ctrl Pts',(0.0252679441965128,0.153490888875607,
1.65023181555931));
#18127=CARTESIAN_POINT('Ctrl Pts',(0.0273279953237563,0.153131925854066,
1.65008419239853));
#18128=CARTESIAN_POINT('Ctrl Pts',(0.0279531343480862,0.153019045555367,
1.65003922680355));
#18129=CARTESIAN_POINT('Ctrl Pts',(0.0290409301239692,0.152815735752017,
1.64996068157849));
#18130=CARTESIAN_POINT('Ctrl Pts',(0.0295039033391887,0.152727025750853,
1.64992715688427));
#18131=CARTESIAN_POINT('Ctrl Pts',(0.0303904628814731,0.152552971037272,
1.64986277346434));
#18132=CARTESIAN_POINT('Ctrl Pts',(0.0308141115406093,0.152467962960981,
1.64983192574029));
#18133=CARTESIAN_POINT('Ctrl Pts',(0.0318081470859526,0.152264190551568,
1.64975935087931));
#18134=CARTESIAN_POINT('Ctrl Pts',(0.0323782284159838,0.152143985266898,
1.64971757813069));
#18135=CARTESIAN_POINT('Ctrl Pts',(0.0343395720239793,0.151718900773944,
1.64957333084143));
#18136=CARTESIAN_POINT('Ctrl Pts',(0.0357272764128497,0.151398125906685,
1.64947035097586));
#18137=CARTESIAN_POINT('Ctrl Pts',(0.0383481723473096,0.15075425329151,
1.64927404850625));
#18138=CARTESIAN_POINT('Ctrl Pts',(0.0395821865771257,0.150434961147849,
1.64918085502293));
#18139=CARTESIAN_POINT('Ctrl Pts',(0.0419622201260025,0.149787833747246,
1.64899959722581));
#18140=CARTESIAN_POINT('Ctrl Pts',(0.0431086740996831,0.149461918668807,
1.64891159858675));
#18141=CARTESIAN_POINT('Ctrl Pts',(0.0444682074201275,0.149058485998785,
1.64880641742109));
#18142=CARTESIAN_POINT('Ctrl Pts',(0.0446850315587759,0.148993629639146,
1.6487896175478));
#18143=CARTESIAN_POINT('Ctrl Pts',(0.0477825914626118,0.148059718869342,
1.64854925400293));
#18144=CARTESIAN_POINT('Ctrl Pts',(0.0506374859098835,0.147107781428493,
1.64832324982666));
#18145=CARTESIAN_POINT('Ctrl Pts',(0.0670354821435085,0.14110613213863,
1.64699946975092));
#18146=CARTESIAN_POINT('Ctrl Pts',(0.0798478749821994,0.134271947911623,
1.6458533670116));
#18147=CARTESIAN_POINT('Ctrl Pts',(0.0934185158888525,0.124395442551841,
1.64459418947251));
#18148=CARTESIAN_POINT('Ctrl Pts',(0.0952738298962443,0.122980259278891,
1.64442114330223));
#18149=CARTESIAN_POINT('Ctrl Pts',(0.0975048878654918,0.121197657906949,
1.644212612415));
#18150=CARTESIAN_POINT('Ctrl Pts',(0.0979114048193897,0.120869484433413,
1.64417459824159));
#18151=CARTESIAN_POINT('Ctrl Pts',(0.0985463757246321,0.120351578744076,
1.64411520245888));
#18152=CARTESIAN_POINT('Ctrl Pts',(0.0987759477626466,0.12016323407049,
1.64409372425862));
#18153=CARTESIAN_POINT('Ctrl Pts',(0.0992041761750668,0.119809851966965,
1.64405365534143));
#18154=CARTESIAN_POINT('Ctrl Pts',(0.099402958605543,0.119644979088099,
1.644035053748));
#18155=CARTESIAN_POINT('Ctrl Pts',(0.0998557774768346,0.119267497402749,
1.64399267485924));
#18156=CARTESIAN_POINT('Ctrl Pts',(0.100109545671274,0.119054571954386,
1.64396892095671));
#18157=CARTESIAN_POINT('Ctrl Pts',(0.100887317786163,0.118397733259442,
1.64389609851998));
#18158=CARTESIAN_POINT('Ctrl Pts',(0.101409073416943,0.117951150932913,
1.64384721973603));
#18159=CARTESIAN_POINT('Ctrl Pts',(0.10872128947443,0.111608074310811,1.64316153026293));
#18160=CARTESIAN_POINT('Ctrl Pts',(0.114992101339153,0.105135885224328,
1.64256480800013));
#18161=CARTESIAN_POINT('Ctrl Pts',(0.126736238818706,0.0906982327804394,
1.64133787331371));
#18162=CARTESIAN_POINT('Ctrl Pts',(0.13209835676458,0.0826937244621174,
1.64071013236468));
#18163=CARTESIAN_POINT('Ctrl Pts',(0.1387894139837,0.0703754215808663,1.63975882676826));
#18164=CARTESIAN_POINT('Ctrl Pts',(0.140726172301134,0.0664179164084416,
1.63945547254118));
#18165=CARTESIAN_POINT('Ctrl Pts',(0.142871091869294,0.0615186612949306,
1.63907988628775));
#18166=CARTESIAN_POINT('Ctrl Pts',(0.143241990890116,0.0606500334301699,
1.63901329769885));
#18167=CARTESIAN_POINT('Ctrl Pts',(0.14381049156699,0.0592843240338944,
1.63890858107055));
#18168=CARTESIAN_POINT('Ctrl Pts',(0.144013483480364,0.05878949841387,1.63887063555498));
#18169=CARTESIAN_POINT('Ctrl Pts',(0.14436898269628,0.057910021110664,1.63880318066238));
#18170=CARTESIAN_POINT('Ctrl Pts',(0.14452251560409,0.0575257871496899,
1.63877370615406));
#18171=CARTESIAN_POINT('Ctrl Pts',(0.144872839991548,0.0566388048512115,
1.63870565367149));
#18172=CARTESIAN_POINT('Ctrl Pts',(0.1450685497369,0.0561356379303422,1.63866703984484));
#18173=CARTESIAN_POINT('Ctrl Pts',(0.145598419287832,0.0547520735697982,
1.63856083193652));
#18174=CARTESIAN_POINT('Ctrl Pts',(0.14592720518945,0.0538696572518743,
1.63849305973633));
#18175=CARTESIAN_POINT('Ctrl Pts',(0.147566469274839,0.0493449416341665,
1.63814532036692));
#18176=CARTESIAN_POINT('Ctrl Pts',(0.148748560080375,0.0456579353734974,
1.63786116083493));
#18177=CARTESIAN_POINT('Ctrl Pts',(0.150341403995638,0.0399677495943722,
1.63742092773571));
#18178=CARTESIAN_POINT('Ctrl Pts',(0.150852294287511,0.0379939919776107,
1.63726793120321));
#18179=CARTESIAN_POINT('Ctrl Pts',(0.154712733765083,0.0217717087940917,
1.63600828353048));
#18180=CARTESIAN_POINT('Ctrl Pts',(0.156074187606125,0.00712789092104505,
1.6348480177686));
#18181=CARTESIAN_POINT('Ctrl Pts',(0.155239727571641,-0.0101836218114814,
1.63354283366155));
#18182=CARTESIAN_POINT('Ctrl Pts',(0.155039772122432,-0.0128744175193736,
1.63334217459848));
#18183=CARTESIAN_POINT('Ctrl Pts',(0.154715338728085,-0.0161016797795056,
1.63310519529515));
#18184=CARTESIAN_POINT('Ctrl Pts',(0.154657913323084,-0.0166442182149594,
1.63306548232412));
#18185=CARTESIAN_POINT('Ctrl Pts',(0.154564266180585,-0.0174866041143586,
1.6330040280689));
#18186=CARTESIAN_POINT('Ctrl Pts',(0.154530024400451,-0.0177866597884741,
1.63298217909055));
#18187=CARTESIAN_POINT('Ctrl Pts',(0.154464946537715,-0.0183425513784935,
1.63294177915638));
#18188=CARTESIAN_POINT('Ctrl Pts',(0.15443434890426,-0.018598408007981,
1.63292321549553));
#18189=CARTESIAN_POINT('Ctrl Pts',(0.154363824260655,-0.0191759572147144,
1.63288138045559));
#18190=CARTESIAN_POINT('Ctrl Pts',(0.154323527480886,-0.0194976010454009,
1.63285813012462));
#18191=CARTESIAN_POINT('Ctrl Pts',(0.154201906116936,-0.0204443642792246,
1.63278982778873));
#18192=CARTESIAN_POINT('Ctrl Pts',(0.154117785318179,-0.0210691282638834,
1.63274492933054));
#18193=CARTESIAN_POINT('Ctrl Pts',(0.153493036751052,-0.0255050413541026,
1.63242726852459));
#18194=CARTESIAN_POINT('Ctrl Pts',(0.152814846553349,-0.029295877355782,
1.63216170028516));
#18195=CARTESIAN_POINT('Ctrl Pts',(0.149346229066439,-0.0452441415977786,
1.6310545253876));
#18196=CARTESIAN_POINT('Ctrl Pts',(0.145239883189182,-0.0570679676901702,
1.63025545384045));
#18197=CARTESIAN_POINT('Ctrl Pts',(0.137841738755214,-0.0722126059881266,
1.6291282522567));
#18198=CARTESIAN_POINT('Ctrl Pts',(0.13575292830234,-0.0760666996721423,
1.6288318105809));
#18199=CARTESIAN_POINT('Ctrl Pts',(0.132139286810853,-0.0821102106241265,
1.62834681508476));
#18200=CARTESIAN_POINT('Ctrl Pts',(0.130715962735821,-0.0843576518202812,
1.62816173812118));
#18201=CARTESIAN_POINT('Ctrl Pts',(0.128789548325315,-0.0872335812082629,
1.62791809706117));
#18202=CARTESIAN_POINT('Ctrl Pts',(0.128338167522774,-0.0878963034601271,
1.62786147038103));
#18203=CARTESIAN_POINT('Ctrl Pts',(0.12759513557189,-0.0889693049913206,
1.62776898193407));
#18204=CARTESIAN_POINT('Ctrl Pts',(0.127306576884649,-0.0893817169409214,
1.62773323770841));
#18205=CARTESIAN_POINT('Ctrl Pts',(0.126747403762903,-0.090172693644091,
1.62766430033181));
#18206=CARTESIAN_POINT('Ctrl Pts',(0.126477081824213,-0.0905514594263828,
1.62763111863301));
#18207=CARTESIAN_POINT('Ctrl Pts',(0.125853700756244,-0.0914166822604713,
1.62755492553131));
#18208=CARTESIAN_POINT('Ctrl Pts',(0.12549951531312,-0.091902314589759,
1.6275118710144));
#18209=CARTESIAN_POINT('Ctrl Pts',(0.124549973800148,-0.0931885287988769,
1.62739706011512));
#18210=CARTESIAN_POINT('Ctrl Pts',(0.123949723620422,-0.0939854446256672,
1.62732511424198));
#18211=CARTESIAN_POINT('Ctrl Pts',(0.119311853432945,-0.100021154511619,
1.62677388799046));
#18212=CARTESIAN_POINT('Ctrl Pts',(0.114952059642142,-0.105002619974225,
1.62628182057047));
#18213=CARTESIAN_POINT('Ctrl Pts',(0.100301786128063,-0.119732780894116,
1.62470339456722));
#18214=CARTESIAN_POINT('Ctrl Pts',(0.0889910152439483,-0.128362542830679,
1.62358093978354));
#18215=CARTESIAN_POINT('Ctrl Pts',(0.0747092684357749,-0.136452933630983,
1.62235060537937));
#18216=CARTESIAN_POINT('Ctrl Pts',(0.0727250401928938,-0.137520717940809,
1.62218360900416));
#18217=CARTESIAN_POINT('Ctrl Pts',(0.0702578804341241,-0.138780041118213,
1.62198136918977));
#18218=CARTESIAN_POINT('Ctrl Pts',(0.0697964062257403,-0.139012701845162,
1.62194376953812));
#18219=CARTESIAN_POINT('Ctrl Pts',(0.0690690724596102,-0.139374865623461,
1.62188487680579));
#18220=CARTESIAN_POINT('Ctrl Pts',(0.0688039943269213,-0.139505914952153,
1.62186348976599));
#18221=CARTESIAN_POINT('Ctrl Pts',(0.0683065312387699,-0.13975008796814,
1.62182349886584));
#18222=CARTESIAN_POINT('Ctrl Pts',(0.0680742408054287,-0.139863387050623,
1.62180488458511));
#18223=CARTESIAN_POINT('Ctrl Pts',(0.0675418477765219,-0.140121419859923,
1.62176235664602));
#18224=CARTESIAN_POINT('Ctrl Pts',(0.0672415621391036,-0.140265768565776,
1.6217384670107));
#18225=CARTESIAN_POINT('Ctrl Pts',(0.0664541678305077,-0.140641162994019,
1.62167607329915));
#18226=CARTESIAN_POINT('Ctrl Pts',(0.0659663120283192,-0.140870645808377,
1.6216376633919));
#18227=CARTESIAN_POINT('Ctrl Pts',(0.0627064436900205,-0.142383409102036,
1.62138259153232));
#18228=CARTESIAN_POINT('Ctrl Pts',(0.0598980985505228,-0.143587445112446,
1.62117045865516));
#18229=CARTESIAN_POINT('Ctrl Pts',(0.0561656990506188,-0.145059065001976,
1.62089604740292));
#18230=CARTESIAN_POINT('Ctrl Pts',(0.0552722903491997,-0.145401829718346,
1.62083091813414));
#18231=CARTESIAN_POINT('Ctrl Pts',(0.0427160679497486,-0.150086688148569,
1.61992257091531));
#18232=CARTESIAN_POINT('Ctrl Pts',(0.0305758766177735,-0.153022345700376,
1.61912506603374));
#18233=CARTESIAN_POINT('Ctrl Pts',(0.0139089090212142,-0.154987558843089,
1.61800229009047));
#18234=CARTESIAN_POINT('Ctrl Pts',(0.00958397355394749,-0.155314982099894,
1.61770887540659));
#18235=CARTESIAN_POINT('Ctrl Pts',(0.00261304499458369,-0.155550450607335,
1.6172283732642));
#18236=CARTESIAN_POINT('Ctrl Pts',(-2.6877447953494E-5,-0.155572389983154,
1.61704467941598));
#18237=CARTESIAN_POINT('Ctrl Pts',(-0.00346548728426643,-0.155513447477885,
1.6168026055892));
#18238=CARTESIAN_POINT('Ctrl Pts',(-0.00426489386183244,-0.155493577314534,
1.61674613164135));
#18239=CARTESIAN_POINT('Ctrl Pts',(-0.00556669045004523,-0.155451173440848,
1.6166538304993));
#18240=CARTESIAN_POINT('Ctrl Pts',(-0.00606919463109662,-0.15543236545974,
1.61661811994087));
#18241=CARTESIAN_POINT('Ctrl Pts',(-0.00703667833054223,-0.155391455198736,
1.61654920434037));
#18242=CARTESIAN_POINT('Ctrl Pts',(-0.00750166788576647,-0.155369701554002,
1.61651601055884));
#18243=CARTESIAN_POINT('Ctrl Pts',(-0.00856789683317475,-0.155315022502935,
1.61643972852662));
#18244=CARTESIAN_POINT('Ctrl Pts',(-0.00916905339990963,-0.15528069265723,
1.61639659682268));
#18245=CARTESIAN_POINT('Ctrl Pts',(-0.0107693250207461,-0.155179981856469,
1.61628144583911));
#18246=CARTESIAN_POINT('Ctrl Pts',(-0.0117680094202036,-0.155107443397999,
1.61620923528349));
#18247=CARTESIAN_POINT('Ctrl Pts',(-0.0195048804513893,-0.154470333450239,
1.61564702504305));
#18248=CARTESIAN_POINT('Ctrl Pts',(-0.0261994534767621,-0.153476668823616,
1.61514364061818));
#18249=CARTESIAN_POINT('Ctrl Pts',(-0.0465427341251147,-0.149087292981438,
1.61356109177057));
#18250=CARTESIAN_POINT('Ctrl Pts',(-0.0598118587421958,-0.144276643097595,
1.61244770586571));
#18251=CARTESIAN_POINT('Ctrl Pts',(-0.0742153613327783,-0.136721567354128,
1.61122909042333));
#18252=CARTESIAN_POINT('Ctrl Pts',(-0.0761544684454786,-0.135651041840217,
1.61106498337927));
#18253=CARTESIAN_POINT('Ctrl Pts',(-0.0785147694634054,-0.134281412300164,
1.61086575619115));
#18254=CARTESIAN_POINT('Ctrl Pts',(-0.0789580834437356,-0.134021221424974,
1.61082836053673));
#18255=CARTESIAN_POINT('Ctrl Pts',(-0.079653855175316,-0.133608206827305,
1.61076971546948));
#18256=CARTESIAN_POINT('Ctrl Pts',(-0.0799071762423404,-0.133456857316653,
1.61074837338163));
#18257=CARTESIAN_POINT('Ctrl Pts',(-0.0803816446792122,-0.133171545564208,
1.61070842040982));
#18258=CARTESIAN_POINT('Ctrl Pts',(-0.0806028860838241,-0.133037754437413,
1.61068979933147));
#18259=CARTESIAN_POINT('Ctrl Pts',(-0.0811092948571913,-0.132729787315012,
1.61064719541816));
#18260=CARTESIAN_POINT('Ctrl Pts',(-0.0813942350286625,-0.132555243814392,
1.61062323692579));
#18261=CARTESIAN_POINT('Ctrl Pts',(-0.082275654491854,-0.132011406080598,
1.61054915921582));
#18262=CARTESIAN_POINT('Ctrl Pts',(-0.0828702109502639,-0.131638986793843,
1.61049923935756));
#18263=CARTESIAN_POINT('Ctrl Pts',(-0.0889730323680434,-0.127758556568765,
1.60998711866178));
#18264=CARTESIAN_POINT('Ctrl Pts',(-0.0942585466354453,-0.123910455787155,
1.60954585498792));
#18265=CARTESIAN_POINT('Ctrl Pts',(-0.106475918302234,-0.113780014484492,
1.60849026713087));
#18266=CARTESIAN_POINT('Ctrl Pts',(-0.113113290732006,-0.107183956619845,
1.60788436084267));
#18267=CARTESIAN_POINT('Ctrl Pts',(-0.123157428193711,-0.0952233449593448,
1.60684173613532));
#18268=CARTESIAN_POINT('Ctrl Pts',(-0.126900462689203,-0.0901748015851321,
1.60641588726636));
#18269=CARTESIAN_POINT('Ctrl Pts',(-0.131131959578575,-0.0836802319201613,
1.60587530442445));
#18270=CARTESIAN_POINT('Ctrl Pts',(-0.131918436185703,-0.0824348104279719,
1.60577196781285));
#18271=CARTESIAN_POINT('Ctrl Pts',(-0.133020543422085,-0.0806334036975268,
1.60562286950216));
#18272=CARTESIAN_POINT('Ctrl Pts',(-0.133350635522648,-0.0800863206037155,
1.60557763701917));
#18273=CARTESIAN_POINT('Ctrl Pts',(-0.133917548202222,-0.0791335166894393,
1.60549893528809));
#18274=CARTESIAN_POINT('Ctrl Pts',(-0.134155920706063,-0.0787287248136627,
1.60546552286574));
#18275=CARTESIAN_POINT('Ctrl Pts',(-0.13461107059375,-0.0779477432779104,
1.60540110065436));
#18276=CARTESIAN_POINT('Ctrl Pts',(-0.134828114049524,-0.0775717130358765,
1.60537010086352));
#18277=CARTESIAN_POINT('Ctrl Pts',(-0.135393310042289,-0.0765829662989665,
1.60528863410829));
#18278=CARTESIAN_POINT('Ctrl Pts',(-0.135738874513178,-0.0759687899531634,
1.60523807489396));
#18279=CARTESIAN_POINT('Ctrl Pts',(-0.136926926855174,-0.0738232619916477,
1.60506159470033));
#18280=CARTESIAN_POINT('Ctrl Pts',(-0.137747740716487,-0.072280127098607,
1.60493490971184));
#18281=CARTESIAN_POINT('Ctrl Pts',(-0.143773936652353,-0.0604752419742803,
1.6039672214554));
#18282=CARTESIAN_POINT('Ctrl Pts',(-0.147851177544411,-0.0496802116189772,
1.6030864788912));
#18283=CARTESIAN_POINT('Ctrl Pts',(-0.152010189535636,-0.0334161921619007,
1.60178501563297));
#18284=CARTESIAN_POINT('Ctrl Pts',(-0.153057848066806,-0.0282318594119336,
1.60137443230578));
#18285=CARTESIAN_POINT('Ctrl Pts',(-0.154347217967444,-0.0196092291115015,
1.60070605620649));
#18286=CARTESIAN_POINT('Ctrl Pts',(-0.154742391955338,-0.0161981870267941,
1.60044537289847));
#18287=CARTESIAN_POINT('Ctrl Pts',(-0.155125986029771,-0.0115438708860894,
1.60009691644077));
#18288=CARTESIAN_POINT('Ctrl Pts',(-0.155212881636932,-0.0103099034523768,
1.60000522377524));
#18289=CARTESIAN_POINT('Ctrl Pts',(-0.155336268681461,-0.00819858687494373,
1.59984965990898));
#18290=CARTESIAN_POINT('Ctrl Pts',(-0.155380067408009,-0.00732174454646084,
1.59978544256913));
#18291=CARTESIAN_POINT('Ctrl Pts',(-0.155431607352676,-0.00607881011711824,
1.59969500816238));
#18292=CARTESIAN_POINT('Ctrl Pts',(-0.15544548242148,-0.00571301136625637,
1.59966846599659));
#18293=CARTESIAN_POINT('Ctrl Pts',(-0.155467115126977,-0.0050840836155134,
1.59962296049571));
#18294=CARTESIAN_POINT('Ctrl Pts',(-0.155475496322718,-0.004820979126039,
1.59960396269339));
#18295=CARTESIAN_POINT('Ctrl Pts',(-0.155490412169377,-0.00431215066376854,
1.59956729864621));
#18296=CARTESIAN_POINT('Ctrl Pts',(-0.155497032284993,-0.00406643244278431,
1.59954962755572));
#18297=CARTESIAN_POINT('Ctrl Pts',(-0.155511551798444,-0.00347548561179453,
1.59950720929809));
#18298=CARTESIAN_POINT('Ctrl Pts',(-0.155518884167485,-0.00313024224005751,
1.59948249358364));
#18299=CARTESIAN_POINT('Ctrl Pts',(-0.155541455586974,-0.00186975543433769,
1.59939248742674));
#18300=CARTESIAN_POINT('Ctrl Pts',(-0.155549765843993,-0.000954381856539534,
1.59932756922752));
#18301=CARTESIAN_POINT('Ctrl Pts',(-0.155551134068566,0.00450845599433179,
1.59894251175487));
#18302=CARTESIAN_POINT('Ctrl Pts',(-0.155352860170298,0.00905426146478352,
1.5986318572618));
#18303=CARTESIAN_POINT('Ctrl Pts',(-0.154448678088801,0.0193674575730714,
1.59793608506419));
#18304=CARTESIAN_POINT('Ctrl Pts',(-0.153618477239644,0.0251169824458964,
1.59755456985286));
#18305=CARTESIAN_POINT('Ctrl Pts',(-0.150286555365268,0.0416072564119696,
1.59644737583076));
#18306=CARTESIAN_POINT('Ctrl Pts',(-0.146963300510667,0.0521436018595768,
1.59572128706499));
#18307=CARTESIAN_POINT('Ctrl Pts',(-0.141853017373797,0.0638482912150727,
1.59483381564902));
#18308=CARTESIAN_POINT('Ctrl Pts',(-0.141123612738972,0.0654446966530539,
1.59471100082097));
#18309=CARTESIAN_POINT('Ctrl Pts',(-0.140063169080135,0.0676654236340094,
1.59453748856884));
#18310=CARTESIAN_POINT('Ctrl Pts',(-0.139754630913405,0.0683003952916319,
1.59448756631896));
#18311=CARTESIAN_POINT('Ctrl Pts',(-0.139249274571283,0.0693226567645971,
1.59440668226401));
#18312=CARTESIAN_POINT('Ctrl Pts',(-0.139055134896915,0.0697112663874624,
1.59437581388086));
#18313=CARTESIAN_POINT('Ctrl Pts',(-0.138647746111038,0.0705182637366695,
1.59431145754517));
#18314=CARTESIAN_POINT('Ctrl Pts',(-0.1384342253951,0.070936508600774,1.59427796034206));
#18315=CARTESIAN_POINT('Ctrl Pts',(-0.137926161880283,0.0719206742820159,
1.59419879667209));
#18316=CARTESIAN_POINT('Ctrl Pts',(-0.1376300267808,0.0724857587810418,
1.59415307456456));
#18317=CARTESIAN_POINT('Ctrl Pts',(-0.136641325530374,0.0743444942841696,
1.59400178093749));
#18318=CARTESIAN_POINT('Ctrl Pts',(-0.13593394908114,0.0756301321293891,
1.59389568731288));
#18319=CARTESIAN_POINT('Ctrl Pts',(-0.132125460839137,0.0823258798620948,
1.59333530373664));
#18320=CARTESIAN_POINT('Ctrl Pts',(-0.128719697480759,0.0875551708774029,
1.59287013634606));
#18321=CARTESIAN_POINT('Ctrl Pts',(-0.118992645195992,0.100691575591468,
1.59162704895687));
#18322=CARTESIAN_POINT('Ctrl Pts',(-0.112197685779111,0.108211341500411,
1.59083604402017));
#18323=CARTESIAN_POINT('Ctrl Pts',(-0.103439407548259,0.116185629617623,
1.58992415061848));
#18324=CARTESIAN_POINT('Ctrl Pts',(-0.102137268875093,0.117331965792144,
1.58979109670331));
#18325=CARTESIAN_POINT('Ctrl Pts',(-0.0976508970352144,0.121150242182378,
1.58934176515385));
#18326=CARTESIAN_POINT('Ctrl Pts',(-0.0943785271117786,0.123716531480324,
1.58902913788554));
#18327=CARTESIAN_POINT('Ctrl Pts',(-0.0904858430417309,0.12652481003959,
1.58867762143987));
#18328=CARTESIAN_POINT('Ctrl Pts',(-0.0899624225478717,0.126897509488944,
1.58863076554809));
#18329=CARTESIAN_POINT('Ctrl Pts',(-0.0891693495499287,0.127454840521981,
1.58856040451098));
#18330=CARTESIAN_POINT('Ctrl Pts',(-0.0889014089021963,0.127641877031725,
1.58853674112355));
#18331=CARTESIAN_POINT('Ctrl Pts',(-0.0884209665925671,0.127975004054119,
1.58849450645339));
#18332=CARTESIAN_POINT('Ctrl Pts',(-0.0882086901163782,0.128121411119852,
1.58847591390732));
#18333=CARTESIAN_POINT('Ctrl Pts',(-0.0877486162166966,0.12843703860928,
1.58843576539972));
#18334=CARTESIAN_POINT('Ctrl Pts',(-0.0875006936127996,0.128606069670505,
1.58841422227375));
#18335=CARTESIAN_POINT('Ctrl Pts',(-0.0868080096992661,0.129075404092504,
1.58835428290342));
#18336=CARTESIAN_POINT('Ctrl Pts',(-0.0863621752602171,0.12937412877617,
1.58831599138052));
#18337=CARTESIAN_POINT('Ctrl Pts',(-0.0837893738352354,0.131078769604917,
1.58809661187422));
#18338=CARTESIAN_POINT('Ctrl Pts',(-0.081629483383893,0.132434634746554,
1.58791866445991));
#18339=CARTESIAN_POINT('Ctrl Pts',(-0.0743414998873913,0.136763553021572,
1.58733513929074));
#18340=CARTESIAN_POINT('Ctrl Pts',(-0.0690831115522936,0.139492968087388,
1.58694107036115));
#18341=CARTESIAN_POINT('Ctrl Pts',(-0.0636885910816225,0.141913938237362,
1.58655050058549));
#18342=CARTESIAN_POINT('',(-0.155549951835907,-0.000122408525016587,1.5855045602941));
#18343=CARTESIAN_POINT('Ctrl Pts',(-0.0636886258330468,0.141913922641502,
1.57264613271722));
#18344=CARTESIAN_POINT('Ctrl Pts',(-0.0641009893096017,0.141728860720327,
1.57267840697396));
#18345=CARTESIAN_POINT('Ctrl Pts',(-0.0645125404901902,0.141542004026234,
1.572710742672));
#18346=CARTESIAN_POINT('Ctrl Pts',(-0.0657682771443213,0.140965247108265,
1.57280979326616));
#18347=CARTESIAN_POINT('Ctrl Pts',(-0.066609771862077,0.140569574921234,
1.57287670606264));
#18348=CARTESIAN_POINT('Ctrl Pts',(-0.0684762451562442,0.139671433497722,
1.57302634481513));
#18349=CARTESIAN_POINT('Ctrl Pts',(-0.0694993329444581,0.139165182704767,
1.57310919892679));
#18350=CARTESIAN_POINT('Ctrl Pts',(-0.0726354278548155,0.137570153615389,
1.57336579223499));
#18351=CARTESIAN_POINT('Ctrl Pts',(-0.0747290332704821,0.136444212032398,
1.57354080031439));
#18352=CARTESIAN_POINT('Ctrl Pts',(-0.0827711363756286,0.13187855044631,
1.57422788854089));
#18353=CARTESIAN_POINT('Ctrl Pts',(-0.088514280696203,0.128094549558014,
1.57475129930091));
#18354=CARTESIAN_POINT('Ctrl Pts',(-0.103637280342916,0.116626620711548,
1.57621574777035));
#18355=CARTESIAN_POINT('Ctrl Pts',(-0.112399649295948,0.108207267080965,
1.57716846422573));
#18356=CARTESIAN_POINT('Ctrl Pts',(-0.120754353733163,0.0980574257201111,
1.57813834724618));
#18357=CARTESIAN_POINT('Ctrl Pts',(-0.121403843831507,0.0972521441515603,
1.57821418932147));
#18358=CARTESIAN_POINT('Ctrl Pts',(-0.122295194171986,0.0961241409372753,
1.57831882957718));
#18359=CARTESIAN_POINT('Ctrl Pts',(-0.122543887254475,0.0958068927318171,
1.57834808641387));
#18360=CARTESIAN_POINT('Ctrl Pts',(-0.122940871744623,0.0952964001535855,
1.57839488291515));
#18361=CARTESIAN_POINT('Ctrl Pts',(-0.123089945057767,0.095103770984556,
1.57841247723702));
#18362=CARTESIAN_POINT('Ctrl Pts',(-0.123400122205798,0.0947010160723929,
1.57844912955671));
#18363=CARTESIAN_POINT('Ctrl Pts',(-0.123561142518773,0.0944908284784867,
1.57846818133122));
#18364=CARTESIAN_POINT('Ctrl Pts',(-0.123948777951951,0.0939821440320722,
1.57851410848399));
#18365=CARTESIAN_POINT('Ctrl Pts',(-0.124174854625687,0.0936832345687884,
1.57854094615465));
#18366=CARTESIAN_POINT('Ctrl Pts',(-0.124958856351856,0.0926388349516308,
1.57863420915078));
#18367=CARTESIAN_POINT('Ctrl Pts',(-0.125511181178498,0.0918891344735284,
1.57870025732461));
#18368=CARTESIAN_POINT('Ctrl Pts',(-0.128439987064137,0.0878380254440191,
1.57905263748089));
#18369=CARTESIAN_POINT('Ctrl Pts',(-0.130693245446137,0.0844489874748747,
1.57933147835119));
#18370=CARTESIAN_POINT('Ctrl Pts',(-0.138703349340222,0.0713112319659295,
1.58036948929031));
#18371=CARTESIAN_POINT('Ctrl Pts',(-0.143523343782884,0.061032705977832,
1.58109818109095));
#18372=CARTESIAN_POINT('Ctrl Pts',(-0.148132973116123,0.0475500180583476,
1.58204864027409));
#18373=CARTESIAN_POINT('Ctrl Pts',(-0.149002034925602,0.0447523651002227,
1.58224542028539));
#18374=CARTESIAN_POINT('Ctrl Pts',(-0.150942859024143,0.0378192491131736,
1.58273422236917));
#18375=CARTESIAN_POINT('Ctrl Pts',(-0.151924184315183,0.0336612365864171,
1.58302839554287));
#18376=CARTESIAN_POINT('Ctrl Pts',(-0.15290082213847,0.0285993782884959,
1.58339022061924));
#18377=CARTESIAN_POINT('Ctrl Pts',(-0.153061072270756,0.0277289369942959,
1.58345256806181));
#18378=CARTESIAN_POINT('Ctrl Pts',(-0.153312881779592,0.0262924236948839,
1.58355569402839));
#18379=CARTESIAN_POINT('Ctrl Pts',(-0.153408756414912,0.0257271199821655,
1.58359633569648));
#18380=CARTESIAN_POINT('Ctrl Pts',(-0.153576028521563,0.0247066435513975,
1.5836698136023));
#18381=CARTESIAN_POINT('Ctrl Pts',(-0.153648533684215,0.0242516568578654,
1.58370261440413));
#18382=CARTESIAN_POINT('Ctrl Pts',(-0.153785235291465,0.0233685958684075,
1.58376635668532));
#18383=CARTESIAN_POINT('Ctrl Pts',(-0.153849668423592,0.0229405620130406,
1.58379729035895));
#18384=CARTESIAN_POINT('Ctrl Pts',(-0.153986700382066,0.0220036992745516,
1.58386507966919));
#18385=CARTESIAN_POINT('Ctrl Pts',(-0.154058565256427,0.021494769961388,
1.58390195811923));
#18386=CARTESIAN_POINT('Ctrl Pts',(-0.154228627503786,0.0202457485549701,
1.58399260116161));
#18387=CARTESIAN_POINT('Ctrl Pts',(-0.154324020593649,0.0195052943559023,
1.58404645332476));
#18388=CARTESIAN_POINT('Ctrl Pts',(-0.155175713289649,0.0124965551309151,
1.5845573346251));
#18389=CARTESIAN_POINT('Ctrl Pts',(-0.155554918866201,0.00618941757411276,
1.58502610640015));
#18390=CARTESIAN_POINT('Ctrl Pts',(-0.155549951835907,-0.000122408525016587,
1.5855045602941));
#18391=CARTESIAN_POINT('Ctrl Pts',(-0.155549951984829,-0.000122219136381302,
1.58550454593792));
#18392=CARTESIAN_POINT('Ctrl Pts',(-0.155538491446423,-0.0147082017546809,
1.58661020339111));
#18393=CARTESIAN_POINT('Ctrl Pts',(-0.153475709607054,-0.0292190019038337,
1.58776745108562));
#18394=CARTESIAN_POINT('Ctrl Pts',(-0.148802379594176,-0.0453720922747867,
1.58902755176202));
#18395=CARTESIAN_POINT('Ctrl Pts',(-0.148136618725812,-0.0475007213513245,
1.58919281443146));
#18396=CARTESIAN_POINT('Ctrl Pts',(-0.147260995464319,-0.0501025644401173,
1.58939323892886));
#18397=CARTESIAN_POINT('Ctrl Pts',(-0.147094296660472,-0.0505898770390524,
1.5894307085037));
#18398=CARTESIAN_POINT('Ctrl Pts',(-0.146828229298458,-0.0513552407590471,
1.58948943906636));
#18399=CARTESIAN_POINT('Ctrl Pts',(-0.146730486280146,-0.0516338461893166,
1.58951079321163));
#18400=CARTESIAN_POINT('Ctrl Pts',(-0.146545704910844,-0.0521557825658739,
1.58955074911237));
#18401=CARTESIAN_POINT('Ctrl Pts',(-0.14645885448696,-0.0523991720044517,
1.58956936115171));
#18402=CARTESIAN_POINT('Ctrl Pts',(-0.14625849122999,-0.0529562795384037,
1.58961191829856));
#18403=CARTESIAN_POINT('Ctrl Pts',(-0.146144575521072,-0.0532698493600022,
1.58963583921745));
#18404=CARTESIAN_POINT('Ctrl Pts',(-0.14578881330739,-0.0542394064791313,
1.58970970910822));
#18405=CARTESIAN_POINT('Ctrl Pts',(-0.145543547778571,-0.0548941440404258,
1.5897594602705));
#18406=CARTESIAN_POINT('Ctrl Pts',(-0.143021884688049,-0.0614900128456147,
1.5902595289591));
#18407=CARTESIAN_POINT('Ctrl Pts',(-0.140387082166975,-0.0672887219819591,
1.59068998170838));
#18408=CARTESIAN_POINT('Ctrl Pts',(-0.134297636723575,-0.0787646396975859,
1.59155484140726));
#18409=CARTESIAN_POINT('Ctrl Pts',(-0.130820217965645,-0.0844144462868939,
1.59198789187369));
#18410=CARTESIAN_POINT('Ctrl Pts',(-0.123490325215985,-0.094777276869097,
1.59282579115613));
#18411=CARTESIAN_POINT('Ctrl Pts',(-0.119701331001564,-0.0995197194283522,
1.59322917291949));
#18412=CARTESIAN_POINT('Ctrl Pts',(-0.113893444138414,-0.105976168084892,
1.59382046568316));
#18413=CARTESIAN_POINT('Ctrl Pts',(-0.112092678362978,-0.107879075754502,
1.59400046833136));
#18414=CARTESIAN_POINT('Ctrl Pts',(-0.109381273124607,-0.110603064638166,
1.5942674716509));
#18415=CARTESIAN_POINT('Ctrl Pts',(-0.108507551249869,-0.111460360634871,
1.59435292497363));
#18416=CARTESIAN_POINT('Ctrl Pts',(-0.106915725200688,-0.112985804704476,
1.59450764301884));
#18417=CARTESIAN_POINT('Ctrl Pts',(-0.106201239844089,-0.113657647947922,
1.59457674620904));
#18418=CARTESIAN_POINT('Ctrl Pts',(-0.105082341619254,-0.114690005718117,
1.5946844662465));
#18419=CARTESIAN_POINT('Ctrl Pts',(-0.104682308369287,-0.115055248610404,
1.59472288191528));
#18420=CARTESIAN_POINT('Ctrl Pts',(-0.104276848401272,-0.115421581214919,
1.59476172424332));
#18421=CARTESIAN_POINT('Ctrl Pts',(-0.104273316613153,-0.115424771886918,
1.594762062575));
#18422=CARTESIAN_POINT('Ctrl Pts',(-0.104266188632333,-0.115431210820863,
1.59476274539356));
#18423=CARTESIAN_POINT('Ctrl Pts',(-0.104262592433992,-0.115434459077119,
1.59476308988071));
#18424=CARTESIAN_POINT('Ctrl Pts',(-0.10425533355106,-0.115441015027213,
1.59476378520881));
#18425=CARTESIAN_POINT('Ctrl Pts',(-0.104251670860391,-0.115444322715207,
1.59476413605006));
#18426=CARTESIAN_POINT('Ctrl Pts',(-0.104244276822995,-0.115450999453986,
1.59476484429339));
#18427=CARTESIAN_POINT('Ctrl Pts',(-0.104240545471063,-0.115454368497553,
1.59476520169566));
#18428=CARTESIAN_POINT('Ctrl Pts',(-0.104233011856434,-0.115461169947195,
1.5947659232761));
#18429=CARTESIAN_POINT('Ctrl Pts',(-0.104229209586497,-0.115464602347268,
1.59476628745466));
#18430=CARTESIAN_POINT('Ctrl Pts',(-0.104221531629341,-0.115471532734658,
1.59476702282681));
#18431=CARTESIAN_POINT('Ctrl Pts',(-0.104217655935357,-0.115475030714798,
1.59476739402075));
#18432=CARTESIAN_POINT('Ctrl Pts',(-0.104209829464429,-0.11548209372588,
1.59476814358221));
#18433=CARTESIAN_POINT('Ctrl Pts',(-0.104205878220374,-0.115485659164419,
1.59476852199414));
#18434=CARTESIAN_POINT('Ctrl Pts',(-0.104197897533482,-0.115492859861755,
1.59476928628899));
#18435=CARTESIAN_POINT('Ctrl Pts',(-0.104193868131432,-0.115496495069185,
1.59476967216763));
#18436=CARTESIAN_POINT('Ctrl Pts',(-0.104187081761086,-0.115502616887622,
1.59477032205367));
#18437=CARTESIAN_POINT('Ctrl Pts',(-0.10418432528971,-0.11550510325396,
1.59477058601844));
#18438=CARTESIAN_POINT('Ctrl Pts',(-0.104178555092443,-0.115510307658326,
1.59477113857399));
#18439=CARTESIAN_POINT('Ctrl Pts',(-0.104175541349362,-0.115513025676923,
1.59477142716557));
#18440=CARTESIAN_POINT('Ctrl Pts',(-0.104169230240371,-0.115518717058501,
1.59477203149712));
#18441=CARTESIAN_POINT('Ctrl Pts',(-0.104165932852789,-0.115521690398911,
1.59477234723813));
#18442=CARTESIAN_POINT('Ctrl Pts',(-0.104159024941802,-0.115527918906233,
1.59477300869137));
#18443=CARTESIAN_POINT('Ctrl Pts',(-0.104155414394165,-0.115531174044115,
1.59477335440467));
#18444=CARTESIAN_POINT('Ctrl Pts',(-0.104147847062779,-0.115537995830658,
1.59477407896804));
#18445=CARTESIAN_POINT('Ctrl Pts',(-0.104143890247432,-0.115541562446195,
1.59477445781963));
#18446=CARTESIAN_POINT('Ctrl Pts',(-0.103798001153679,-0.115853309617982,
1.59480757473686));
#18447=CARTESIAN_POINT('Ctrl Pts',(-0.103454706161338,-0.116159967965073,
1.59484037625974));
#18448=CARTESIAN_POINT('Ctrl Pts',(-0.102684789330843,-0.116841598537461,
1.59491379539122));
#18449=CARTESIAN_POINT('Ctrl Pts',(-0.102257466540345,-0.117215765277699,
1.59495444589779));
#18450=CARTESIAN_POINT('Ctrl Pts',(-0.10117222881644,-0.118155555915076,
1.59505744051841));
#18451=CARTESIAN_POINT('Ctrl Pts',(-0.100511620385407,-0.118718024697535,
1.59511991313928));
#18452=CARTESIAN_POINT('Ctrl Pts',(-0.0967726047640296,-0.121847995796988,
1.5954723086324));
#18453=CARTESIAN_POINT('Ctrl Pts',(-0.0936008302561725,-0.124301046747286,
1.59576678718968));
#18454=CARTESIAN_POINT('Ctrl Pts',(-0.0887801218319639,-0.127740186614871,
1.59620847516393));
#18455=CARTESIAN_POINT('Ctrl Pts',(-0.0872017938363406,-0.128822792743492,
1.59635219285179));
#18456=CARTESIAN_POINT('Ctrl Pts',(-0.0733365962841737,-0.137961632791901,
1.59760686314945));
#18457=CARTESIAN_POINT('Ctrl Pts',(-0.0599875829553543,-0.14426739288354,
1.59877186826312));
#18458=CARTESIAN_POINT('Ctrl Pts',(-0.0434518173529107,-0.149380718370231,
1.60007426281184));
#18459=CARTESIAN_POINT('Ctrl Pts',(-0.0409307752605421,-0.150091083329582,
1.60026893035934));
#18460=CARTESIAN_POINT('Ctrl Pts',(-0.0378687789950389,-0.150870972998337,
1.60049976261099));
#18461=CARTESIAN_POINT('Ctrl Pts',(-0.0373440511814109,-0.151001711184865,
1.60053912285829));
#18462=CARTESIAN_POINT('Ctrl Pts',(-0.0365262973534834,-0.151200934651514,
1.60060014585674));
#18463=CARTESIAN_POINT('Ctrl Pts',(-0.0362337434210195,-0.151271308845205,
1.60062191397313));
#18464=CARTESIAN_POINT('Ctrl Pts',(-0.0356902669833577,-0.151400375649145,
1.60066223325285));
#18465=CARTESIAN_POINT('Ctrl Pts',(-0.0354394052980914,-0.151459293072542,
1.60068079675295));
#18466=CARTESIAN_POINT('Ctrl Pts',(-0.0348714535585298,-0.151591193987663,
1.60072271846523));
#18467=CARTESIAN_POINT('Ctrl Pts',(-0.0345542808419705,-0.151663805994165,
1.60074605520443));
#18468=CARTESIAN_POINT('Ctrl Pts',(-0.0337358981894035,-0.151848462068656,
1.60080608342902));
#18469=CARTESIAN_POINT('Ctrl Pts',(-0.0332343515683297,-0.151959021301206,
1.60084269197597));
#18470=CARTESIAN_POINT('Ctrl Pts',(-0.0301791796583233,-0.152616643331872,
1.601064651903));
#18471=CARTESIAN_POINT('Ctrl Pts',(-0.0276124635346965,-0.15310185080803,
1.60124670734571));
#18472=CARTESIAN_POINT('Ctrl Pts',(-0.013087507785053,-0.155470404943941,
1.60225847370539));
#18473=CARTESIAN_POINT('Ctrl Pts',(-0.000952604160578558,-0.156017600948628,
1.60303630552406));
#18474=CARTESIAN_POINT('Ctrl Pts',(0.0185569001430925,-0.154618803304722,
1.60433387041633));
#18475=CARTESIAN_POINT('Ctrl Pts',(0.0259408193680818,-0.153552544362755,
1.60483550064718));
#18476=CARTESIAN_POINT('Ctrl Pts',(0.0342923725770274,-0.151726867270332,
1.60543071201355));
#18477=CARTESIAN_POINT('Ctrl Pts',(0.0353629313006877,-0.151480929663042,
1.60550753120635));
#18478=CARTESIAN_POINT('Ctrl Pts',(0.037304855217024,-0.151013107507209,
1.60564787829376));
#18479=CARTESIAN_POINT('Ctrl Pts',(0.0381770793018721,-0.150794964826758,
1.60571128590364));
#18480=CARTESIAN_POINT('Ctrl Pts',(0.0395534839803293,-0.150438019821967,
1.60581195401872));
#18481=CARTESIAN_POINT('Ctrl Pts',(0.0400589500622079,-0.1503042128841,
1.60584905339225));
#18482=CARTESIAN_POINT('Ctrl Pts',(0.0409630275035369,-0.150060001176227,
1.60591564753866));
#18483=CARTESIAN_POINT('Ctrl Pts',(0.0413618933100495,-0.149950549685586,
1.60594511122004));
#18484=CARTESIAN_POINT('Ctrl Pts',(0.0422813648041068,-0.149694292716365,
1.60601322638313));
#18485=CARTESIAN_POINT('Ctrl Pts',(0.042801648105003,-0.14954636066248,
1.60605191408833));
#18486=CARTESIAN_POINT('Ctrl Pts',(0.0442302732157723,-0.149132093953987,
1.6061585498992));
#18487=CARTESIAN_POINT('Ctrl Pts',(0.045136958731249,-0.148860180702317,
1.60622667856557));
#18488=CARTESIAN_POINT('Ctrl Pts',(0.0497985951275568,-0.147415660652176,
1.60657934372105));
#18489=CARTESIAN_POINT('Ctrl Pts',(0.0535102374539595,-0.146109296074309,
1.60686821576001));
#18490=CARTESIAN_POINT('Ctrl Pts',(0.0590109264500262,-0.143935539167679,
1.60730910289901));
#18491=CARTESIAN_POINT('Ctrl Pts',(0.0608396022899218,-0.143172172850268,
1.6074578508425));
#18492=CARTESIAN_POINT('Ctrl Pts',(0.0760617286545473,-0.136473526198417,
1.60871425493073));
#18493=CARTESIAN_POINT('Ctrl Pts',(0.0885675115807059,-0.128709470481681,
1.60987562209073));
#18494=CARTESIAN_POINT('Ctrl Pts',(0.101852403437895,-0.117596919525811,
1.61117959919475));
#18495=CARTESIAN_POINT('Ctrl Pts',(0.103858326047605,-0.115829176009994,
1.61137839771205));
#18496=CARTESIAN_POINT('Ctrl Pts',(0.106216566638279,-0.1136403951341,1.61161346385528));
#18497=CARTESIAN_POINT('Ctrl Pts',(0.106613354810553,-0.113268226058625,
1.61165306250203));
#18498=CARTESIAN_POINT('Ctrl Pts',(0.10722708436266,-0.112686493611665,
1.6117143740992));
#18499=CARTESIAN_POINT('Ctrl Pts',(0.107445377135773,-0.11247837303137,
1.61173619399909));
#18500=CARTESIAN_POINT('Ctrl Pts',(0.107849008024455,-0.112091303579534,
1.61177656056892));
#18501=CARTESIAN_POINT('Ctrl Pts',(0.108034505150202,-0.111912530884119,
1.61179511982888));
#18502=CARTESIAN_POINT('Ctrl Pts',(0.108452606383653,-0.111507577885951,
1.61183697040504));
#18503=CARTESIAN_POINT('Ctrl Pts',(0.108684947048038,-0.11128113069057,
1.61186024055892));
#18504=CARTESIAN_POINT('Ctrl Pts',(0.109367769416864,-0.110611450109255,
1.61192867542775));
#18505=CARTESIAN_POINT('Ctrl Pts',(0.109816267856839,-0.110166189155547,
1.61197368565408));
#18506=CARTESIAN_POINT('Ctrl Pts',(0.113008144300139,-0.106958491154229,
1.61229456172564));
#18507=CARTESIAN_POINT('Ctrl Pts',(0.115649962477262,-0.104096360051836,
1.61256306584535));
#18508=CARTESIAN_POINT('Ctrl Pts',(0.118973248598713,-0.100213023861677,
1.61290965119603));
#18509=CARTESIAN_POINT('Ctrl Pts',(0.119753790463617,-0.0992789697551679,
1.61299173799172));
#18510=CARTESIAN_POINT('Ctrl Pts',(0.129916160190895,-0.0868236684504053,
1.61407107780314));
#18511=CARTESIAN_POINT('Ctrl Pts',(0.137611047442096,-0.0740255833049523,
1.61501769906086));
#18512=CARTESIAN_POINT('Ctrl Pts',(0.144647674180816,-0.0573030255549669,
1.61626024620509));
#18513=CARTESIAN_POINT('Ctrl Pts',(0.1458250664502,-0.0542368295019263,
1.61648787510743));
#18514=CARTESIAN_POINT('Ctrl Pts',(0.147187876624879,-0.0503217111952048,
1.61677937258711));
#18515=CARTESIAN_POINT('Ctrl Pts',(0.147464493213308,-0.0495052404372288,
1.61684020634253));
#18516=CARTESIAN_POINT('Ctrl Pts',(0.147895991165963,-0.0481959038810381,
1.6169378520534));
#18517=CARTESIAN_POINT('Ctrl Pts',(0.148055231497199,-0.0477044837354233,
1.6169745204323));
#18518=CARTESIAN_POINT('Ctrl Pts',(0.148352194074432,-0.0467722385928116,
1.61704412414389));
#18519=CARTESIAN_POINT('Ctrl Pts',(0.148490407000467,-0.0463315746555803,
1.61707704298228));
#18520=CARTESIAN_POINT('Ctrl Pts',(0.148799230140329,-0.045331377578911,
1.61715180424851));
#18521=CARTESIAN_POINT('Ctrl Pts',(0.148968649719736,-0.0447714872094166,
1.61719368503133));
#18522=CARTESIAN_POINT('Ctrl Pts',(0.149460536441214,-0.0431122159625067,
1.61731790106654));
#18523=CARTESIAN_POINT('Ctrl Pts',(0.149774013737616,-0.0420102344294362,
1.61740052666116));
#18524=CARTESIAN_POINT('Ctrl Pts',(0.15260073891637,-0.0316393156406922,
1.61817950146115));
#18525=CARTESIAN_POINT('Ctrl Pts',(0.154262194263629,-0.0221616663302259,
1.61890361821304));
#18526=CARTESIAN_POINT('Ctrl Pts',(0.155498454352139,-0.0069415028431265,
1.62008027058633));
#18527=CARTESIAN_POINT('Ctrl Pts',(0.155648131324104,-0.00126910782265343,
1.62052131682621));
#18528=CARTESIAN_POINT('Ctrl Pts',(0.155285799835476,0.0115390096794103,
1.62151272711295));
#18529=CARTESIAN_POINT('Ctrl Pts',(0.154592155718011,0.0186580014901159,
1.62206070911721));
#18530=CARTESIAN_POINT('Ctrl Pts',(0.153272328652688,0.0265349597668693,
1.62264779499802));
#18531=CARTESIAN_POINT('Ctrl Pts',(0.153126511334706,0.02736388919834,1.62270933041169));
#18532=CARTESIAN_POINT('Ctrl Pts',(0.15290876174406,0.0285454467125072,
1.62279665258911));
#18533=CARTESIAN_POINT('Ctrl Pts',(0.15284232639969,0.0288990521284464,
1.62282273548038));
#18534=CARTESIAN_POINT('Ctrl Pts',(0.152725376908729,0.0295098362577918,
1.62286769830176));
#18535=CARTESIAN_POINT('Ctrl Pts',(0.15267543885169,0.0297671221949332,
1.62288661060182));
#18536=CARTESIAN_POINT('Ctrl Pts',(0.152577093417965,0.030267049393774,
1.62292330340858));
#18537=CARTESIAN_POINT('Ctrl Pts',(0.152528757467485,0.0305097011235796,
1.62294108799456));
#18538=CARTESIAN_POINT('Ctrl Pts',(0.152396246944083,0.0311667324322055,
1.62298917796088));
#18539=CARTESIAN_POINT('Ctrl Pts',(0.152310960507785,0.0315808900069481,
1.62301942056542));
#18540=CARTESIAN_POINT('Ctrl Pts',(0.151985024893486,0.0331316223537152,
1.62313241057119));
#18541=CARTESIAN_POINT('Ctrl Pts',(0.151733325781553,0.0342658759284377,
1.62321455594131));
#18542=CARTESIAN_POINT('Ctrl Pts',(0.149489407706759,0.0438678618898174,
1.62390654670031));
#18543=CARTESIAN_POINT('Ctrl Pts',(0.146802490387278,0.0521588710615691,
1.62448196320056));
#18544=CARTESIAN_POINT('Ctrl Pts',(0.139837337937942,0.0687591919449881,
1.62566791106308));
#18545=CARTESIAN_POINT('Ctrl Pts',(0.135477172078487,0.0769949797846055,
1.62627630484703));
#18546=CARTESIAN_POINT('Ctrl Pts',(0.128049777669527,0.0884181414269208,
1.62720152331419));
#18547=CARTESIAN_POINT('Ctrl Pts',(0.125541825453071,0.0919443171454096,
1.62749958074425));
#18548=CARTESIAN_POINT('Ctrl Pts',(0.122314515324278,0.0961032998971747,
1.62786930134601));
#18549=CARTESIAN_POINT('Ctrl Pts',(0.121731929724715,0.096840188592139,
1.62793553181913));
#18550=CARTESIAN_POINT('Ctrl Pts',(0.120807993965982,0.0979873249105489,
1.62803980184016));
#18551=CARTESIAN_POINT('Ctrl Pts',(0.120471138713455,0.0984011787195175,
1.62807766137335));
#18552=CARTESIAN_POINT('Ctrl Pts',(0.119869415365946,0.0991327233402488,
1.62814501919019));
#18553=CARTESIAN_POINT('Ctrl Pts',(0.119605395605289,0.0994511081540412,
1.62817448296013));
#18554=CARTESIAN_POINT('Ctrl Pts',(0.118993242028814,0.100183348538964,
1.62824259096909));
#18555=CARTESIAN_POINT('Ctrl Pts',(0.118644215225826,0.100596447018815,
1.62828127139845));
#18556=CARTESIAN_POINT('Ctrl Pts',(0.117678659710625,0.101727236933942,
1.62838786824827));
#18557=CARTESIAN_POINT('Ctrl Pts',(0.11705773498536,0.10244112598021,1.62845596501337));
#18558=CARTESIAN_POINT('Ctrl Pts',(0.113825380935251,0.106089663973962,
1.62880820151027));
#18559=CARTESIAN_POINT('Ctrl Pts',(0.111110201860496,0.108930032774784,
1.62909666427657));
#18560=CARTESIAN_POINT('Ctrl Pts',(0.106864621967582,0.113047340626661,
1.62953749603657));
#18561=CARTESIAN_POINT('Ctrl Pts',(0.10541227774224,0.114402796107027,1.62968661436019));
#18562=CARTESIAN_POINT('Ctrl Pts',(0.0930373740300897,0.125516408366512,
1.63094315755684));
#18563=CARTESIAN_POINT('Ctrl Pts',(0.0808145956572658,0.133713293366128,
1.63210426934996));
#18564=CARTESIAN_POINT('Ctrl Pts',(0.0652165164700719,0.141243669643269,
1.63340836092647));
#18565=CARTESIAN_POINT('Ctrl Pts',(0.0627760123512031,0.142345153953356,
1.63360745264081));
#18566=CARTESIAN_POINT('Ctrl Pts',(0.0598064430301666,0.143594178342537,
1.63384281895697));
#18567=CARTESIAN_POINT('Ctrl Pts',(0.0593036714474582,0.143802549554729,
1.6338824342949));
#18568=CARTESIAN_POINT('Ctrl Pts',(0.0585205380821814,0.144122309569973,
1.63394376609378));
#18569=CARTESIAN_POINT('Ctrl Pts',(0.0582409352313616,0.144235526001098,
1.63396558961549));
#18570=CARTESIAN_POINT('Ctrl Pts',(0.0577219348874819,0.144443923723307,
1.63400595950676));
#18571=CARTESIAN_POINT('Ctrl Pts',(0.0574826325525906,0.14453932276196,
1.63402451848401));
#18572=CARTESIAN_POINT('Ctrl Pts',(0.0569414823546903,0.144753498411835,
1.63406636414789));
#18573=CARTESIAN_POINT('Ctrl Pts',(0.0566394999374847,0.144871925393607,
1.63408962969368));
#18574=CARTESIAN_POINT('Ctrl Pts',(0.0557483655392799,0.145218184950564,
1.63415803848032));
#18575=CARTESIAN_POINT('Ctrl Pts',(0.0551581839969529,0.145443378244983,
1.63420302740827));
#18576=CARTESIAN_POINT('Ctrl Pts',(0.050928096019057,0.147027984704399,
1.6345233349603));
#18577=CARTESIAN_POINT('Ctrl Pts',(0.0472393694787453,0.1482543344237,1.63479132151644));
#18578=CARTESIAN_POINT('Ctrl Pts',(0.0382617588238942,0.150869817069479,
1.63542543736143));
#18579=CARTESIAN_POINT('Ctrl Pts',(0.0329380507054243,0.15212086218133,
1.63578683279977));
#18580=CARTESIAN_POINT('Ctrl Pts',(0.0183162213266262,0.154753094581853,
1.63676575034025));
#18581=CARTESIAN_POINT('Ctrl Pts',(0.00894222820702628,0.15557642651765,
1.63737974698278));
#18582=CARTESIAN_POINT('Ctrl Pts',(-0.00479705107421926,0.155536816711758,
1.63831252813579));
#18583=CARTESIAN_POINT('Ctrl Pts',(-0.00914283221186623,0.155341931498338,
1.63861213383822));
#18584=CARTESIAN_POINT('Ctrl Pts',(-0.0144117077594486,0.154883796176454,
1.63898356514615));
#18585=CARTESIAN_POINT('Ctrl Pts',(-0.0153482117848556,0.154793798209709,
1.63904989686948));
#18586=CARTESIAN_POINT('Ctrl Pts',(-0.0168148261158964,0.154639416742765,
1.63915429104215));
#18587=CARTESIAN_POINT('Ctrl Pts',(-0.017345531104498,0.154580788345859,
1.63919217275941));
#18588=CARTESIAN_POINT('Ctrl Pts',(-0.0182867992969613,0.15447189567868,
1.63925955317337));
#18589=CARTESIAN_POINT('Ctrl Pts',(-0.0186974859233309,0.154422723707281,
1.6392890172563));
#18590=CARTESIAN_POINT('Ctrl Pts',(-0.0196443511186888,0.154305521884548,
1.6393571016759));
#18591=CARTESIAN_POINT('Ctrl Pts',(-0.0201803782875225,0.154236334673412,
1.63939575809348));
#18592=CARTESIAN_POINT('Ctrl Pts',(-0.0216523074370992,0.154038542356466,
1.63950222639143));
#18593=CARTESIAN_POINT('Ctrl Pts',(-0.0225874018261968,0.153904204472222,
1.6395702179044));
#18594=CARTESIAN_POINT('Ctrl Pts',(-0.0273865823106737,0.153170063832257,
1.63992104413842));
#18595=CARTESIAN_POINT('Ctrl Pts',(-0.0312279455946206,0.152433276152811,
1.64020816085631));
#18596=CARTESIAN_POINT('Ctrl Pts',(-0.0369886077255515,0.151101479231752,
1.64064881192362));
#18597=CARTESIAN_POINT('Ctrl Pts',(-0.0389310677558046,0.150612700262753,
1.64079914989949));
#18598=CARTESIAN_POINT('Ctrl Pts',(-0.0486830380937218,0.147957569881437,
1.64156267073385));
#18599=CARTESIAN_POINT('Ctrl Pts',(-0.0563140102735931,0.145223530492718,
1.6421896099303));
#18600=CARTESIAN_POINT('Ctrl Pts',(-0.0636886598674488,0.141913907367419,
1.64281642759095));
#18601=CARTESIAN_POINT('Origin',(0.,0.,-0.129405622560373));
#18602=CARTESIAN_POINT('',(-0.0636886248462869,0.141913923084343,1.72674034350975));
#18603=CARTESIAN_POINT('',(-0.0636886260955797,0.141913922523681,1.71290984779881));
#18604=CARTESIAN_POINT('',(-0.0636886258329924,0.141913922641526,-0.129405622560373));
#18605=CARTESIAN_POINT('',(-0.155549925504284,0.000142733485857199,1.66943656442265));
#18606=CARTESIAN_POINT('Ctrl Pts',(-0.0636886248462869,0.141913923084343,
1.72674034350975));
#18607=CARTESIAN_POINT('Ctrl Pts',(-0.0621902796711602,0.142586355652444,
1.72661900977629));
#18608=CARTESIAN_POINT('Ctrl Pts',(-0.0606812720557253,0.143235064542905,
1.72649690634238));
#18609=CARTESIAN_POINT('Ctrl Pts',(-0.0502628428185461,0.147519630401365,
1.72565450019174));
#18610=CARTESIAN_POINT('Ctrl Pts',(-0.0410442217624049,0.150345333593974,
1.72491025279256));
#18611=CARTESIAN_POINT('Ctrl Pts',(-0.0228284591095591,0.154127809374507,
1.72346757472166));
#18612=CARTESIAN_POINT('Ctrl Pts',(-0.0138888489024449,0.155189123259374,
1.72277247368547));
#18613=CARTESIAN_POINT('Ctrl Pts',(-0.00422002387772398,0.155494262660439,
1.72206350403877));
#18614=CARTESIAN_POINT('Ctrl Pts',(-0.0035333195842798,0.15551138228955,
1.7220133882769));
#18615=CARTESIAN_POINT('Ctrl Pts',(-0.0025152771248716,0.155530015210193,
1.72193946442735));
#18616=CARTESIAN_POINT('Ctrl Pts',(-0.00218402404886312,0.155535019512673,
1.72191546943375));
#18617=CARTESIAN_POINT('Ctrl Pts',(-0.00159451054005605,0.155542041695949,
1.72187287391598));
#18618=CARTESIAN_POINT('Ctrl Pts',(-0.00133625934049361,0.15554447471248,
1.7218542506026));
#18619=CARTESIAN_POINT('Ctrl Pts',(-0.000781080073054311,0.155548322324139,
1.72181429434771));
#18620=CARTESIAN_POINT('Ctrl Pts',(-0.000484154410688755,0.155549529933284,
1.72179297311045));
#18621=CARTESIAN_POINT('Ctrl Pts',(0.000335130299288034,0.155550516044807,
1.72173427231057));
#18622=CARTESIAN_POINT('Ctrl Pts',(0.000857494205561969,0.155548513585851,
1.7216969905533));
#18623=CARTESIAN_POINT('Ctrl Pts',(0.00371153867656535,0.155523195020484,
1.72149403721382));
#18624=CARTESIAN_POINT('Ctrl Pts',(0.00604263981905059,0.155450081347442,
1.72133098112));
#18625=CARTESIAN_POINT('Ctrl Pts',(0.0227955254658225,0.154547167001268,
1.72017293357849));
#18626=CARTESIAN_POINT('Ctrl Pts',(0.0370426749005134,0.151764344056263,
1.71925593674634));
#18627=CARTESIAN_POINT('Ctrl Pts',(0.0535441078097416,0.146074862506836,
1.71808701521844));
#18628=CARTESIAN_POINT('Ctrl Pts',(0.0563565522332939,0.145013014471313,
1.71788407502271));
#18629=CARTESIAN_POINT('Ctrl Pts',(0.0593257138165678,0.143792573158951,
1.71766483809867));
#18630=CARTESIAN_POINT('Ctrl Pts',(0.0595149195771825,0.143714365192403,
1.71765084568062));
#18631=CARTESIAN_POINT('Ctrl Pts',(0.060628188029096,0.143251621550014,
1.71756838539903));
#18632=CARTESIAN_POINT('Ctrl Pts',(0.0615486600053697,0.142858554662465,
1.71749967638848));
#18633=CARTESIAN_POINT('Ctrl Pts',(0.0645049474021633,0.141562263683949,
1.71727719848676));
#18634=CARTESIAN_POINT('Ctrl Pts',(0.0665250987980878,0.140624226602029,
1.71712238342063));
#18635=CARTESIAN_POINT('Ctrl Pts',(0.0693242904106561,0.139250634783446,
1.71690356064034));
#18636=CARTESIAN_POINT('Ctrl Pts',(0.070120846455336,0.138851227442003,
1.71684079425987));
#18637=CARTESIAN_POINT('Ctrl Pts',(0.0714259751798809,0.13818271806797,
1.71673711024488));
#18638=CARTESIAN_POINT('Ctrl Pts',(0.0719365725886382,0.137917595001939,
1.71669633199495));
#18639=CARTESIAN_POINT('Ctrl Pts',(0.072853656223835,0.13743492941285,1.71662269659871));
#18640=CARTESIAN_POINT('Ctrl Pts',(0.0732606704849775,0.137218399639411,
1.7165898754797));
#18641=CARTESIAN_POINT('Ctrl Pts',(0.0741272961890235,0.136752403758898,
1.71651968749743));
#18642=CARTESIAN_POINT('Ctrl Pts',(0.0745866231069483,0.13650242347777,
1.71648230269036));
#18643=CARTESIAN_POINT('Ctrl Pts',(0.0758245583202079,0.135820586011575,
1.71638104257065));
#18644=CARTESIAN_POINT('Ctrl Pts',(0.0766007232022802,0.135384357931939,
1.71631701188344));
#18645=CARTESIAN_POINT('Ctrl Pts',(0.0805180282808756,0.133138243997113,
1.71599104083602));
#18646=CARTESIAN_POINT('Ctrl Pts',(0.0835987048773317,0.13122574963496,
1.7157254247197));
#18647=CARTESIAN_POINT('Ctrl Pts',(0.0990752212562384,0.120851633452506,
1.71434095445131));
#18648=CARTESIAN_POINT('Ctrl Pts',(0.110264933582334,0.110736177202784,
1.71315843172312));
#18649=CARTESIAN_POINT('Ctrl Pts',(0.122719629522112,0.0956882025727495,
1.71166485677054));
#18650=CARTESIAN_POINT('Ctrl Pts',(0.125455521444773,0.0920720441788441,
1.71132314837159));
#18651=CARTESIAN_POINT('Ctrl Pts',(0.128406743986182,0.0877949372396135,
1.71094248750993));
#18652=CARTESIAN_POINT('Ctrl Pts',(0.128780148148875,0.0872462972929728,
1.71089408581105));
#18653=CARTESIAN_POINT('Ctrl Pts',(0.129332110189271,0.0864240388497398,
1.71082219936142));
#18654=CARTESIAN_POINT('Ctrl Pts',(0.129513329272134,0.0861522301701557,
1.71079854208761));
#18655=CARTESIAN_POINT('Ctrl Pts',(0.129836059376996,0.0856648508895601,
1.71075631401498));
#18656=CARTESIAN_POINT('Ctrl Pts',(0.129977891278066,0.0854494983891286,
1.71073772198102));
#18657=CARTESIAN_POINT('Ctrl Pts',(0.130283640625665,0.0849827368135727,
1.71069756967657));
#18658=CARTESIAN_POINT('Ctrl Pts',(0.130447365756298,0.0847312064259459,
1.71067602226329));
#18659=CARTESIAN_POINT('Ctrl Pts',(0.130901967046047,0.0840283631318044,
1.71061605889121));
#18660=CARTESIAN_POINT('Ctrl Pts',(0.131191239832641,0.0835760097218225,
1.71057774778998));
#18661=CARTESIAN_POINT('Ctrl Pts',(0.132842999884799,0.080963344304532,
1.71035803352663));
#18662=CARTESIAN_POINT('Ctrl Pts',(0.134154559932035,0.0787710722785302,
1.71017978216496));
#18663=CARTESIAN_POINT('Ctrl Pts',(0.142668881122267,0.0637093034277671,
1.70898881459483));
#18664=CARTESIAN_POINT('Ctrl Pts',(0.148064372925472,0.0499032798740733,
1.70805412698548));
#18665=CARTESIAN_POINT('Ctrl Pts',(0.151860681372334,0.0337284438750968,
1.7069379584023));
#18666=CARTESIAN_POINT('Ctrl Pts',(0.152253800459681,0.0319069637616406,
1.70681209572631));
#18667=CARTESIAN_POINT('Ctrl Pts',(0.153400017014601,0.0260913009158145,
1.7064090056545));
#18668=CARTESIAN_POINT('Ctrl Pts',(0.154029287767484,0.0220747544083784,
1.70612872805264));
#18669=CARTESIAN_POINT('Ctrl Pts',(0.154601630055619,0.0171726061421569,
1.70578225223314));
#18670=CARTESIAN_POINT('Ctrl Pts',(0.154695438831028,0.016305936568474,
1.70572083424175));
#18671=CARTESIAN_POINT('Ctrl Pts',(0.154838465462932,0.0148719964267047,
1.70561892495261));
#18672=CARTESIAN_POINT('Ctrl Pts',(0.15489186297775,0.0143051540458542,
1.70557856486868));
#18673=CARTESIAN_POINT('Ctrl Pts',(0.154982822217146,0.01327928559562,1.70550538014689));
#18674=CARTESIAN_POINT('Ctrl Pts',(0.155021459761912,0.012820359325902,
1.70547258961052));
#18675=CARTESIAN_POINT('Ctrl Pts',(0.15509994685119,0.0118358283690187,
1.70540213153404));
#18676=CARTESIAN_POINT('Ctrl Pts',(0.155139163817248,0.0113101805414122,
1.70536444460437));
#18677=CARTESIAN_POINT('Ctrl Pts',(0.155238745155906,0.0098773073973731,
1.70526151970379));
#18678=CARTESIAN_POINT('Ctrl Pts',(0.155293827139638,0.00896974838637173,
1.70519611749477));
#18679=CARTESIAN_POINT('Ctrl Pts',(0.155541871189152,0.00419023123780119,
1.70485052656883));
#18680=CARTESIAN_POINT('Ctrl Pts',(0.155597971960112,0.000312878410750554,
1.70456611098715));
#18681=CARTESIAN_POINT('Ctrl Pts',(0.155169831926513,-0.0183776312293385,
1.70317398794097));
#18682=CARTESIAN_POINT('Ctrl Pts',(0.152714794916144,-0.0330674755562086,
1.7020058566634));
#18683=CARTESIAN_POINT('Ctrl Pts',(0.146875203436004,-0.05141170805286,
1.70053476160677));
#18684=CARTESIAN_POINT('Ctrl Pts',(0.145348872480629,-0.0555806033333861,
1.70020041206912));
#18685=CARTESIAN_POINT('Ctrl Pts',(0.143392726748624,-0.0602890107288308,
1.69982694537498));
#18686=CARTESIAN_POINT('Ctrl Pts',(0.143135386460692,-0.0608974554787733,
1.69977876658327));
#18687=CARTESIAN_POINT('Ctrl Pts',(0.142745243939314,-0.0618037551798422,
1.69970714559602));
#18688=CARTESIAN_POINT('Ctrl Pts',(0.142615373296841,-0.0621028511932481,
1.69968353270926));
#18689=CARTESIAN_POINT('Ctrl Pts',(0.142381134503401,-0.0626377003586985,
1.69964135247382));
#18690=CARTESIAN_POINT('Ctrl Pts',(0.142277120340909,-0.0628736033621158,
1.69962276409479));
#18691=CARTESIAN_POINT('Ctrl Pts',(0.142050574907161,-0.0633839648923704,
1.6995825839355));
#18692=CARTESIAN_POINT('Ctrl Pts',(0.141927834871523,-0.0636583264764555,
1.69956100517044));
#18693=CARTESIAN_POINT('Ctrl Pts',(0.141582785348254,-0.0644236591788939,
1.69950086619507));
#18694=CARTESIAN_POINT('Ctrl Pts',(0.14135871533123,-0.0649138397557635,
1.6994624118407));
#18695=CARTESIAN_POINT('Ctrl Pts',(0.140044389966331,-0.0677500079083123,
1.69924022813088));
#18696=CARTESIAN_POINT('Ctrl Pts',(0.138898211917177,-0.0700698478122041,
1.69905973408469));
#18697=CARTESIAN_POINT('Ctrl Pts',(0.130846717308816,-0.0853910809206949,
1.69786881045817));
#18698=CARTESIAN_POINT('Ctrl Pts',(0.122183178584942,-0.0973852161518665,
1.69693567752971));
#18699=CARTESIAN_POINT('Ctrl Pts',(0.110642208770475,-0.109351340065427,
1.69581874591437));
#18700=CARTESIAN_POINT('Ctrl Pts',(0.109298041309343,-0.110694858485372,
1.69569035814836));
#18701=CARTESIAN_POINT('Ctrl Pts',(0.105032569139117,-0.114804821627704,
1.69528741956143));
#18702=CARTESIAN_POINT('Ctrl Pts',(0.102028540804921,-0.117482593256126,
1.69500992031412));
#18703=CARTESIAN_POINT('Ctrl Pts',(0.0982538541989605,-0.120593272780645,
1.69466652874491));
#18704=CARTESIAN_POINT('Ctrl Pts',(0.0975787844512952,-0.121140158805345,
1.69460531547638));
#18705=CARTESIAN_POINT('Ctrl Pts',(0.096454506142932,-0.122035461544504,
1.69450367580057));
#18706=CARTESIAN_POINT('Ctrl Pts',(0.0960078991214324,-0.122387127265827,
1.69446337938529));
#18707=CARTESIAN_POINT('Ctrl Pts',(0.0951960336694066,-0.123019225009838,
1.6943902627325));
#18708=CARTESIAN_POINT('Ctrl Pts',(0.0948314366721004,-0.123300499426217,
1.69435747630302));
#18709=CARTESIAN_POINT('Ctrl Pts',(0.0940462976561442,-0.123900665627293,
1.69428697446816));
#18710=CARTESIAN_POINT('Ctrl Pts',(0.0936253719542922,-0.124219043465397,
1.69424923944512));
#18711=CARTESIAN_POINT('Ctrl Pts',(0.0924724870374513,-0.12508186849218,
1.69414604904736));
#18712=CARTESIAN_POINT('Ctrl Pts',(0.091737355735077,-0.12562202108412,
1.69408042800136));
#18713=CARTESIAN_POINT('Ctrl Pts',(0.087819326678101,-0.128448140427465,
1.69373157275498));
#18714=CARTESIAN_POINT('Ctrl Pts',(0.0845559194517856,-0.130619486613579,
1.69344401596673));
#18715=CARTESIAN_POINT('Ctrl Pts',(0.0686006736491443,-0.140386888143415,
1.69205050820341));
#18716=CARTESIAN_POINT('Ctrl Pts',(0.0549510210868276,-0.146269513419567,
1.69088465877147));
#18717=CARTESIAN_POINT('Ctrl Pts',(0.0364148689997084,-0.151292089567808,
1.68941729520283));
#18718=CARTESIAN_POINT('Ctrl Pts',(0.0321008433189015,-0.152265833028252,
1.68908425966835));
#18719=CARTESIAN_POINT('Ctrl Pts',(0.0271012745242674,-0.153172318264588,
1.68871207958855));
#18720=CARTESIAN_POINT('Ctrl Pts',(0.0264510568042694,-0.153285941296637,
1.68866394183213));
#18721=CARTESIAN_POINT('Ctrl Pts',(0.0254786767409904,-0.153449489345264,
1.68859236972694));
#18722=CARTESIAN_POINT('Ctrl Pts',(0.0251570602629359,-0.153502544190706,
1.68856876502321));
#18723=CARTESIAN_POINT('Ctrl Pts',(0.0245807756505278,-0.15359575004806,
1.68852659359464));
#18724=CARTESIAN_POINT('Ctrl Pts',(0.0243261734729441,-0.153636279088315,
1.6885080058772));
#18725=CARTESIAN_POINT('Ctrl Pts',(0.0237744438685795,-0.153722700682457,
1.68846782052689));
#18726=CARTESIAN_POINT('Ctrl Pts',(0.0234772846073057,-0.153768364750389,
1.68844623593852));
#18727=CARTESIAN_POINT('Ctrl Pts',(0.0226825125674879,-0.153888138690049,
1.68838865982359));
#18728=CARTESIAN_POINT('Ctrl Pts',(0.022184663753379,-0.15396069731827,
1.68835275437093));
#18729=CARTESIAN_POINT('Ctrl Pts',(0.0207276994924552,-0.15416582767185,
1.68824812194769));
#18730=CARTESIAN_POINT('Ctrl Pts',(0.0197676656421202,-0.154291864548211,
1.68817974064249));
#18731=CARTESIAN_POINT('Ctrl Pts',(0.0117002595409241,-0.155274447353317,
1.6876093631198));
#18732=CARTESIAN_POINT('Ctrl Pts',(0.00454170618044673,-0.155648488354195,
1.68713068333181));
#18733=CARTESIAN_POINT('Ctrl Pts',(-0.0151857048727512,-0.155316411781556,
1.68582582001257));
#18734=CARTESIAN_POINT('Ctrl Pts',(-0.0276801780676523,-0.153582471245924,
1.68501150631254));
#18735=CARTESIAN_POINT('Ctrl Pts',(-0.0418752221184455,-0.149822383142834,
1.68400173179385));
#18736=CARTESIAN_POINT('Ctrl Pts',(-0.0439094940949159,-0.149238856601813,
1.68385504424759));
#18737=CARTESIAN_POINT('Ctrl Pts',(-0.0471129417140584,-0.148248788398493,
1.68362052776947));
#18738=CARTESIAN_POINT('Ctrl Pts',(-0.0482903037082227,-0.147869465916276,
1.68353357278228));
#18739=CARTESIAN_POINT('Ctrl Pts',(-0.0500274918601302,-0.147286819065948,
1.68340408039277));
#18740=CARTESIAN_POINT('Ctrl Pts',(-0.0505908975013504,-0.147094248985235,
1.68336189641236));
#18741=CARTESIAN_POINT('Ctrl Pts',(-0.0515905862066681,-0.146746136037554,
1.68328670693969));
#18742=CARTESIAN_POINT('Ctrl Pts',(-0.0520273089034335,-0.146591869306822,
1.68325374395372));
#18743=CARTESIAN_POINT('Ctrl Pts',(-0.0529444080338,-0.146263301270018,
1.68318427577034));
#18744=CARTESIAN_POINT('Ctrl Pts',(-0.0534246266353773,-0.146088578943822,
1.68314775693024));
#18745=CARTESIAN_POINT('Ctrl Pts',(-0.0546787698962851,-0.145625261773817,
1.68305200312311));
#18746=CARTESIAN_POINT('Ctrl Pts',(-0.0554512631295895,-0.145332866594336,
1.68299264218823));
#18747=CARTESIAN_POINT('Ctrl Pts',(-0.0589214847480966,-0.14398766350857,
1.68272422422411));
#18748=CARTESIAN_POINT('Ctrl Pts',(-0.0615916560628935,-0.142865861636052,
1.68251287238652));
#18749=CARTESIAN_POINT('Ctrl Pts',(-0.0687469479031943,-0.1396218791372,
1.68193280630791));
#18750=CARTESIAN_POINT('Ctrl Pts',(-0.07316405003253,-0.137358744072712,
1.68155961454382));
#18751=CARTESIAN_POINT('Ctrl Pts',(-0.0837218573212822,-0.131295509928521,
1.6806308223803));
#18752=CARTESIAN_POINT('Ctrl Pts',(-0.0897206945410314,-0.127271541947837,
1.68007022374981));
#18753=CARTESIAN_POINT('Ctrl Pts',(-0.0987082351388976,-0.120290654484318,
1.67918843258652));
#18754=CARTESIAN_POINT('Ctrl Pts',(-0.101894438825308,-0.11760392757248,
1.67886664288369));
#18755=CARTESIAN_POINT('Ctrl Pts',(-0.105730888838739,-0.114095781323018,
1.67847045657023));
#18756=CARTESIAN_POINT('Ctrl Pts',(-0.106485776219649,-0.113391568151434,
1.6783920583149));
#18757=CARTESIAN_POINT('Ctrl Pts',(-0.109469377391134,-0.110552176207903,
1.67808059380407));
#18758=CARTESIAN_POINT('Ctrl Pts',(-0.111641529068101,-0.108358205449172,
1.67785019934036));
#18759=CARTESIAN_POINT('Ctrl Pts',(-0.114115999024375,-0.105705410009279,
1.67758481793004));
#18760=CARTESIAN_POINT('Ctrl Pts',(-0.114482805595466,-0.105308034758351,
1.67754540036274));
#18761=CARTESIAN_POINT('Ctrl Pts',(-0.115072580211439,-0.10466238636816,
1.67748190641606));
#18762=CARTESIAN_POINT('Ctrl Pts',(-0.115296830485323,-0.104415299274141,
1.67745773664183));
#18763=CARTESIAN_POINT('Ctrl Pts',(-0.115693396686145,-0.103975512911542,
1.67741494872579));
#18764=CARTESIAN_POINT('Ctrl Pts',(-0.115866028711086,-0.103783104196319,
1.67739630699268));
#18765=CARTESIAN_POINT('Ctrl Pts',(-0.116234898285699,-0.103369909412223,
1.6773564419577));
#18766=CARTESIAN_POINT('Ctrl Pts',(-0.116430986365507,-0.103148994998968,
1.67733522979475));
#18767=CARTESIAN_POINT('Ctrl Pts',(-0.116832064831628,-0.102694535824578,
1.67729179746501));
#18768=CARTESIAN_POINT('Ctrl Pts',(-0.117036987233973,-0.102460932480184,
1.67726958231469));
#18769=CARTESIAN_POINT('Ctrl Pts',(-0.117975589053052,-0.101384473995773,
1.67716770979881));
#18770=CARTESIAN_POINT('Ctrl Pts',(-0.118700898655694,-0.100534312698694,
1.67708864586632));
#18771=CARTESIAN_POINT('Ctrl Pts',(-0.124017663084639,-0.0941645775738576,
1.67650586116718));
#18772=CARTESIAN_POINT('Ctrl Pts',(-0.12823187938772,-0.0883400418125101,
1.67602561287012));
#18773=CARTESIAN_POINT('Ctrl Pts',(-0.135105043945632,-0.0773063737489884,
1.67516577306635));
#18774=CARTESIAN_POINT('Ctrl Pts',(-0.137901615269926,-0.0721996784829089,
1.67478508094758));
#18775=CARTESIAN_POINT('Ctrl Pts',(-0.14429005042737,-0.0588017038235194,
1.67380353963478));
#18776=CARTESIAN_POINT('Ctrl Pts',(-0.14745756184697,-0.0503337688795338,
1.67319805828984));
#18777=CARTESIAN_POINT('Ctrl Pts',(-0.150179245924141,-0.0405377002749772,
1.67248620391373));
#18778=CARTESIAN_POINT('Ctrl Pts',(-0.150473291748599,-0.0394322126766379,
1.67240573522298));
#18779=CARTESIAN_POINT('Ctrl Pts',(-0.1508991655586,-0.0377569358248633,
1.67228354188828));
#18780=CARTESIAN_POINT('Ctrl Pts',(-0.151040021851116,-0.0371894629089671,
1.67224210792303));
#18781=CARTESIAN_POINT('Ctrl Pts',(-0.151286427096358,-0.0361722664439251,
1.67216775443045));
#18782=CARTESIAN_POINT('Ctrl Pts',(-0.15139317903366,-0.0357228388698459,
1.67213487394908));
#18783=CARTESIAN_POINT('Ctrl Pts',(-0.151615167547079,-0.0347693943048376,
1.6720650546568));
#18784=CARTESIAN_POINT('Ctrl Pts',(-0.151729896008312,-0.0342652660291548,
1.67202810000512));
#18785=CARTESIAN_POINT('Ctrl Pts',(-0.151958238584241,-0.0332382689430707,
1.67195273538521));
#18786=CARTESIAN_POINT('Ctrl Pts',(-0.152071672269328,-0.0327153675799722,
1.67191432018145));
#18787=CARTESIAN_POINT('Ctrl Pts',(-0.152347430496839,-0.0314117615938241,
1.67181843846283));
#18788=CARTESIAN_POINT('Ctrl Pts',(-0.152506452286314,-0.0306303821785156,
1.67176086756998));
#18789=CARTESIAN_POINT('Ctrl Pts',(-0.154591595367232,-0.0199657264572257,
1.67097367949842));
#18790=CARTESIAN_POINT('Ctrl Pts',(-0.155559175245397,-0.00992182041362863,
1.67021316201263));
#18791=CARTESIAN_POINT('Ctrl Pts',(-0.155549934436305,0.000142817580648246,
1.66943657356483));
#18792=CARTESIAN_POINT('Ctrl Pts',(-0.155549934512386,0.000142734692933504,
1.66943657996045));
#18793=CARTESIAN_POINT('Ctrl Pts',(-0.155539137165992,0.0119095062458819,
1.6685286547989));
#18794=CARTESIAN_POINT('Ctrl Pts',(-0.154193252094498,0.0236380265554001,
1.6676035159115));
#18795=CARTESIAN_POINT('Ctrl Pts',(-0.151337655230667,0.0359652464455898,
1.66666617482456));
#18796=CARTESIAN_POINT('Ctrl Pts',(-0.151130694450945,0.0368252376739049,
1.66660098940656));
#18797=CARTESIAN_POINT('Ctrl Pts',(-0.150801489054699,0.0381436547827868,
1.66650142185785));
#18798=CARTESIAN_POINT('Ctrl Pts',(-0.150684468554527,0.0386033476928826,
1.66646677418678));
#18799=CARTESIAN_POINT('Ctrl Pts',(-0.150487433397983,0.0393628142365004,
1.66640965369194));
#18800=CARTESIAN_POINT('Ctrl Pts',(-0.150408622536469,0.0396628923111269,
1.66638711588306));
#18801=CARTESIAN_POINT('Ctrl Pts',(-0.150253114584839,0.040247870811502,
1.66634324428768));
#18802=CARTESIAN_POINT('Ctrl Pts',(-0.150176503741395,0.0405327925916355,
1.66632190575373));
#18803=CARTESIAN_POINT('Ctrl Pts',(-0.150031233585902,0.041066997726144,
1.66628195576479));
#18804=CARTESIAN_POINT('Ctrl Pts',(-0.149962764227588,0.0413163248639212,
1.66626333413331));
#18805=CARTESIAN_POINT('Ctrl Pts',(-0.149804362163746,0.0418875552102819,
1.66622072414155));
#18806=CARTESIAN_POINT('Ctrl Pts',(-0.149714013519591,0.0422093397995702,
1.66619676014939));
#18807=CARTESIAN_POINT('Ctrl Pts',(-0.149430701463523,0.0432060259544392,
1.66612264852466));
#18808=CARTESIAN_POINT('Ctrl Pts',(-0.14923420267766,0.0438799272961263,
1.66607270051438));
#18809=CARTESIAN_POINT('Ctrl Pts',(-0.147171696164676,0.0507792456934329,
1.66556278043678));
#18810=CARTESIAN_POINT('Ctrl Pts',(-0.144921546684449,0.0568841835550285,
1.66512353976677));
#18811=CARTESIAN_POINT('Ctrl Pts',(-0.14050220428334,0.0668927945026448,
1.66439574086609));
#18812=CARTESIAN_POINT('Ctrl Pts',(-0.138535671451816,0.0708758427997087,
1.66410392300456));
#18813=CARTESIAN_POINT('Ctrl Pts',(-0.133991836450683,0.0791651363283613,
1.66348177255836));
#18814=CARTESIAN_POINT('Ctrl Pts',(-0.131371266710808,0.0834417067831042,
1.66315166620737));
#18815=CARTESIAN_POINT('Ctrl Pts',(-0.12517581927803,0.0925348804722615,
1.66241681467428));
#18816=CARTESIAN_POINT('Ctrl Pts',(-0.121519943266147,0.0972860727935802,
1.66201061047322));
#18817=CARTESIAN_POINT('Ctrl Pts',(-0.116553790789091,0.103022177224845,
1.66148235382466));
#18818=CARTESIAN_POINT('Ctrl Pts',(-0.115489513312837,0.104213852873291,
1.66137039643182));
#18819=CARTESIAN_POINT('Ctrl Pts',(-0.114058271967494,0.105767566756887,
1.66122134764429));
#18820=CARTESIAN_POINT('Ctrl Pts',(-0.113707567033721,0.106144508900237,
1.66118494228352));
#18821=CARTESIAN_POINT('Ctrl Pts',(-0.113010548470682,0.106886254705663,
1.66111281232678));
#18822=CARTESIAN_POINT('Ctrl Pts',(-0.112664323758821,0.107251133568759,
1.66107709178419));
#18823=CARTESIAN_POINT('Ctrl Pts',(-0.111994324880774,0.107950406854623,
1.66100816975163));
#18824=CARTESIAN_POINT('Ctrl Pts',(-0.111670807098616,0.108285040420481,
1.66097497957913));
#18825=CARTESIAN_POINT('Ctrl Pts',(-0.110925552528462,0.109049009557853,
1.66089872404221));
#18826=CARTESIAN_POINT('Ctrl Pts',(-0.110502818544229,0.109477357312976,
1.66085561532559));
#18827=CARTESIAN_POINT('Ctrl Pts',(-0.109370904472022,0.110611067350389,
1.6607405656587));
#18828=CARTESIAN_POINT('Ctrl Pts',(-0.108657398884225,0.111312050318993,
1.66066843396511));
#18829=CARTESIAN_POINT('Ctrl Pts',(-0.103099606565561,0.116667942460483,
1.66010946271525));
#18830=CARTESIAN_POINT('Ctrl Pts',(-0.0979658329955401,0.121010779089143,
1.6596094160886));
#18831=CARTESIAN_POINT('Ctrl Pts',(-0.0843613742516448,0.131084872809554,
1.65832247287911));
#18832=CARTESIAN_POINT('Ctrl Pts',(-0.0755763720173321,0.136338799584819,
1.65752347763966));
#18833=CARTESIAN_POINT('Ctrl Pts',(-0.0654607327810812,0.141108618882644,
1.65666259874332));
#18834=CARTESIAN_POINT('Ctrl Pts',(-0.0645765368292703,0.141515442845773,
1.65658783762612));
#18835=CARTESIAN_POINT('Ctrl Pts',(-0.0636886255459746,0.141913922770335,
1.65651328069486));
#18836=CARTESIAN_POINT('Ctrl Pts',(-0.0636886598674488,0.141913907367419,
1.64281642759095));
#18837=CARTESIAN_POINT('Ctrl Pts',(-0.0696330708281112,0.139246152143079,
1.64332168031176));
#18838=CARTESIAN_POINT('Ctrl Pts',(-0.0754109669663114,0.136204428267244,
1.64382658077215));
#18839=CARTESIAN_POINT('Ctrl Pts',(-0.0832833891595775,0.131403626069983,
1.64452090893243));
#18840=CARTESIAN_POINT('Ctrl Pts',(-0.0855430853569352,0.129943906277431,
1.64472095711442));
#18841=CARTESIAN_POINT('Ctrl Pts',(-0.0882139005972584,0.12811872317121,
1.64495730235532));
#18842=CARTESIAN_POINT('Ctrl Pts',(-0.0886622273260183,0.12780887666781,
1.64499697193528));
#18843=CARTESIAN_POINT('Ctrl Pts',(-0.0893563051957705,0.127323777480203,
1.64505836938074));
#18844=CARTESIAN_POINT('Ctrl Pts',(-0.08960318421742,0.12715015915208,1.64508020466903));
#18845=CARTESIAN_POINT('Ctrl Pts',(-0.0900598428983295,0.126827022189883,
1.64512058536336));
#18846=CARTESIAN_POINT('Ctrl Pts',(-0.0902697544971528,0.126677702400157,
1.64513914343452));
#18847=CARTESIAN_POINT('Ctrl Pts',(-0.0907429770297453,0.126339303854352,
1.64518097319549));
#18848=CARTESIAN_POINT('Ctrl Pts',(-0.0910060678913912,0.12614992346714,
1.64520422381417));
#18849=CARTESIAN_POINT('Ctrl Pts',(-0.0917792790783532,0.125589665965622,
1.64527254814335));
#18850=CARTESIAN_POINT('Ctrl Pts',(-0.0922877464173775,0.125216501161205,
1.64531746810929));
#18851=CARTESIAN_POINT('Ctrl Pts',(-0.0958922898108027,0.122537238655754,
1.64563594524948));
#18852=CARTESIAN_POINT('Ctrl Pts',(-0.0989041643992458,0.120119435183958,
1.64590226541571));
#18853=CARTESIAN_POINT('Ctrl Pts',(-0.111212056617696,0.109461978895362,
1.64700659241976));
#18854=CARTESIAN_POINT('Ctrl Pts',(-0.119593975365025,0.100236594805785,
1.64780253800066));
#18855=CARTESIAN_POINT('Ctrl Pts',(-0.129343642028543,0.0865185434543424,
1.648927809384));
#18856=CARTESIAN_POINT('Ctrl Pts',(-0.131743353118494,0.0828185961175443,
1.64922596428644));
#18857=CARTESIAN_POINT('Ctrl Pts',(-0.135339569960334,0.0767211732355931,
1.64971348892717));
#18858=CARTESIAN_POINT('Ctrl Pts',(-0.136636999311302,0.0743859297701268,
1.64989933389391));
#18859=CARTESIAN_POINT('Ctrl Pts',(-0.13824533020108,0.0713069127118367,
1.65014383348089));
#18860=CARTESIAN_POINT('Ctrl Pts',(-0.138611538128635,0.0705924116116407,
1.65020053306397));
#18861=CARTESIAN_POINT('Ctrl Pts',(-0.139198355740396,0.0694253104936047,
1.65029310342311));
#18862=CARTESIAN_POINT('Ctrl Pts',(-0.139422331690481,0.0689744111471147,
1.65032885619316));
#18863=CARTESIAN_POINT('Ctrl Pts',(-0.139848993042136,0.068104904046188,
1.65039778430641));
#18864=CARTESIAN_POINT('Ctrl Pts',(-0.140051998053364,0.0676864583403743,
1.65043094809085));
#18865=CARTESIAN_POINT('Ctrl Pts',(-0.140512695921535,0.0667258951248426,
1.65050706362396));
#18866=CARTESIAN_POINT('Ctrl Pts',(-0.140769132144931,0.0661831867759373,
1.65055005825754));
#18867=CARTESIAN_POINT('Ctrl Pts',(-0.141442373725473,0.0647367580688794,
1.65066462960091));
#18868=CARTESIAN_POINT('Ctrl Pts',(-0.141853652048706,0.0638305118669644,
1.65073639462226));
#18869=CARTESIAN_POINT('Ctrl Pts',(-0.144894198105596,0.0569561672351944,
1.65128071634126));
#18870=CARTESIAN_POINT('Ctrl Pts',(-0.147154115014761,0.0508328387688611,
1.65176569269126));
#18871=CARTESIAN_POINT('Ctrl Pts',(-0.152609498950707,0.0325991504708884,
1.65321090196849));
#18872=CARTESIAN_POINT('Ctrl Pts',(-0.154736235093912,0.0202242079391262,
1.65419674266683));
#18873=CARTESIAN_POINT('Ctrl Pts',(-0.155486463517174,0.00514398693103164,
1.65534527268703));
#18874=CARTESIAN_POINT('Ctrl Pts',(-0.155550535912096,0.00255606724769628,
1.65554031219657));
#18875=CARTESIAN_POINT('Ctrl Pts',(-0.155549684800338,-0.00152922855669905,
1.65584381983182));
#18876=CARTESIAN_POINT('Ctrl Pts',(-0.155527767599779,-0.00302604029328143,
1.65595409233396));
#18877=CARTESIAN_POINT('Ctrl Pts',(-0.155470640415711,-0.00499013556192593,
1.65609737461512));
#18878=CARTESIAN_POINT('Ctrl Pts',(-0.15545492428974,-0.00545783964186859,
1.65613138851678));
#18879=CARTESIAN_POINT('Ctrl Pts',(-0.15542624885748,-0.00621005391579775,
1.65618591631687));
#18880=CARTESIAN_POINT('Ctrl Pts',(-0.155414618645756,-0.00649460686367938,
1.6562065026805));
#18881=CARTESIAN_POINT('Ctrl Pts',(-0.155390829282578,-0.00703994525832174,
1.65624587568077));
#18882=CARTESIAN_POINT('Ctrl Pts',(-0.155378795250698,-0.00730072886467567,
1.6562646686136));
#18883=CARTESIAN_POINT('Ctrl Pts',(-0.155348921076262,-0.00791455449382164,
1.6563088215818));
#18884=CARTESIAN_POINT('Ctrl Pts',(-0.155330533965986,-0.00826756777560345,
1.65633415087878));
#18885=CARTESIAN_POINT('Ctrl Pts',(-0.155266286447439,-0.00942507830682467,
1.65641700591314));
#18886=CARTESIAN_POINT('Ctrl Pts',(-0.155215377120556,-0.010229300459691,
1.65647425819608));
#18887=CARTESIAN_POINT('Ctrl Pts',(-0.155079624390963,-0.0121383854708783,
1.65660949677501));
#18888=CARTESIAN_POINT('Ctrl Pts',(-0.154989219180336,-0.0132428249859943,
1.65668720227188));
#18889=CARTESIAN_POINT('Ctrl Pts',(-0.154617457942235,-0.0172564884077534,
1.65696796573091));
#18890=CARTESIAN_POINT('Ctrl Pts',(-0.154265910475499,-0.0201587693636289,
1.65716787423104));
#18891=CARTESIAN_POINT('Ctrl Pts',(-0.152660455799996,-0.0308735473163772,
1.6579000569243));
#18892=CARTESIAN_POINT('Ctrl Pts',(-0.150892899133274,-0.0385971554754417,
1.65841670732667));
#18893=CARTESIAN_POINT('Ctrl Pts',(-0.145417038713349,-0.0562213604750931,
1.65963272517138));
#18894=CARTESIAN_POINT('Ctrl Pts',(-0.14127393965906,-0.0659437576669107,
1.66033395098969));
#18895=CARTESIAN_POINT('Ctrl Pts',(-0.135630689927324,-0.0761669931610973,
1.66115162361125));
#18896=CARTESIAN_POINT('Ctrl Pts',(-0.135070416611611,-0.0771561879066619,
1.66123159960294));
#18897=CARTESIAN_POINT('Ctrl Pts',(-0.13420646198002,-0.0786432962058877,
1.66135318233756));
#18898=CARTESIAN_POINT('Ctrl Pts',(-0.133910731248095,-0.0791458054172151,
1.66139450267861));
#18899=CARTESIAN_POINT('Ctrl Pts',(-0.133375814087743,-0.0800431622486336,
1.66146872148062));
#18900=CARTESIAN_POINT('Ctrl Pts',(-0.133137680665298,-0.0804386324161293,
1.66150158138257));
#18901=CARTESIAN_POINT('Ctrl Pts',(-0.132628757659542,-0.0812753540107831,
1.66157143026112));
#18902=CARTESIAN_POINT('Ctrl Pts',(-0.132357519081919,-0.081716324308003,
1.6616084353776));
#18903=CARTESIAN_POINT('Ctrl Pts',(-0.131626074080158,-0.0828922862668488,
1.66170764307559));
#18904=CARTESIAN_POINT('Ctrl Pts',(-0.131161920090704,-0.0836247879630223,
1.66176999046477));
#18905=CARTESIAN_POINT('Ctrl Pts',(-0.128878585763506,-0.087162439543451,
1.66207383103529));
#18906=CARTESIAN_POINT('Ctrl Pts',(-0.126975542748679,-0.0899121186349089,
1.66231842819615));
#18907=CARTESIAN_POINT('Ctrl Pts',(-0.116045692141403,-0.104664819909547,
1.66367941556095));
#18908=CARTESIAN_POINT('Ctrl Pts',(-0.105406201266564,-0.115371964736592,
1.66486106855164));
#18909=CARTESIAN_POINT('Ctrl Pts',(-0.0927583720169072,-0.124869270264632,
1.6660726566817));
#18910=CARTESIAN_POINT('Ctrl Pts',(-0.0921110448530989,-0.12534753962072,
1.66613416883196));
#18911=CARTESIAN_POINT('Ctrl Pts',(-0.0904911099740408,-0.126525081974917,
1.66628682152846));
#18912=CARTESIAN_POINT('Ctrl Pts',(-0.0895140652474005,-0.1272181969108,
1.66637775821602));
#18913=CARTESIAN_POINT('Ctrl Pts',(-0.0860956409361392,-0.129584342684377,
1.66669178116432));
#18914=CARTESIAN_POINT('Ctrl Pts',(-0.0836143996295749,-0.131199072049607,
1.66691249641876));
#18915=CARTESIAN_POINT('Ctrl Pts',(-0.0806327420107087,-0.133020481491082,
1.66716805035641));
#18916=CARTESIAN_POINT('Ctrl Pts',(-0.0801756623993111,-0.133296476927886,
1.66720696381084));
#18917=CARTESIAN_POINT('Ctrl Pts',(-0.0794324578715335,-0.133740035384074,
1.66726980156947));
#18918=CARTESIAN_POINT('Ctrl Pts',(-0.0791472077299594,-0.133909043541375,
1.66729381626074));
#18919=CARTESIAN_POINT('Ctrl Pts',(-0.0786388476163664,-0.134208050502176,
1.66733642809792));
#18920=CARTESIAN_POINT('Ctrl Pts',(-0.0784159528092604,-0.134338406730369,
1.66735504814494));
#18921=CARTESIAN_POINT('Ctrl Pts',(-0.0779363488900173,-0.134617294500187,
1.66739497625711));
#18922=CARTESIAN_POINT('Ctrl Pts',(-0.0776795399353789,-0.134765646721615,
1.66741627271742));
#18923=CARTESIAN_POINT('Ctrl Pts',(-0.0769703944147217,-0.135172602115724,
1.66747485499864));
#18924=CARTESIAN_POINT('Ctrl Pts',(-0.0765171746668741,-0.135429671715231,
1.66751204362349));
#18925=CARTESIAN_POINT('Ctrl Pts',(-0.0740438155234889,-0.136816199528646,
1.66771367587367));
#18926=CARTESIAN_POINT('Ctrl Pts',(-0.0719998140710258,-0.137902818643324,
1.66787554369753));
#18927=CARTESIAN_POINT('Ctrl Pts',(-0.0570948028164132,-0.145404716711965,
1.66902758374665));
#18928=CARTESIAN_POINT('Ctrl Pts',(-0.0434225200963941,-0.150056473541935,
1.6699402891408));
#18929=CARTESIAN_POINT('Ctrl Pts',(-0.0263668142056738,-0.153328210403919,
1.67110271705952));
#18930=CARTESIAN_POINT('Ctrl Pts',(-0.023413799724451,-0.153806831536226,
1.67130453543832));
#18931=CARTESIAN_POINT('Ctrl Pts',(-0.0168406777585501,-0.15467851383071,
1.67175701362771));
#18932=CARTESIAN_POINT('Ctrl Pts',(-0.0132169975193409,-0.155030185554693,
1.67200863604789));
#18933=CARTESIAN_POINT('Ctrl Pts',(-0.00866347803873654,-0.155311294684052,
1.6723290736954));
#18934=CARTESIAN_POINT('Ctrl Pts',(-0.00774193572927483,-0.155359957755644,
1.67239413894371));
#18935=CARTESIAN_POINT('Ctrl Pts',(-0.00628508900860785,-0.155423894146872,
1.67249736250885));
#18936=CARTESIAN_POINT('Ctrl Pts',(-0.00575003410384543,-0.155444608495739,
1.67253535068103));
#18937=CARTESIAN_POINT('Ctrl Pts',(-0.00475537792328659,-0.155477973580735,
1.67260611849973));
#18938=CARTESIAN_POINT('Ctrl Pts',(-0.00429580540813051,-0.155491350034431,
1.67263887510052));
#18939=CARTESIAN_POINT('Ctrl Pts',(-0.00327810358583532,-0.155516456303218,
1.6727115468847));
#18940=CARTESIAN_POINT('Ctrl Pts',(-0.00271995908620184,-0.15552721932762,
1.6727514918256));
#18941=CARTESIAN_POINT('Ctrl Pts',(-0.00110780371142387,-0.155549626620776,
1.67286713403311));
#18942=CARTESIAN_POINT('Ctrl Pts',(-5.37351301366745E-5,-0.155553561777881,
1.67294307053711));
#18943=CARTESIAN_POINT('Ctrl Pts',(0.0078371315832451,-0.155502818304252,
1.67351408898011));
#18944=CARTESIAN_POINT('Ctrl Pts',(0.0146625772559204,-0.155008161139295,
1.67402284845758));
#18945=CARTESIAN_POINT('Ctrl Pts',(0.0322087304461537,-0.152567279615475,
1.67536978566281));
#18946=CARTESIAN_POINT('Ctrl Pts',(0.0427976767973349,-0.149941669114859,
1.67622289292575));
#18947=CARTESIAN_POINT('Ctrl Pts',(0.0542038428614482,-0.145805758563602,
1.6771537820205));
#18948=CARTESIAN_POINT('Ctrl Pts',(0.0553778441067607,-0.14536392376341,
1.67724970476158));
#18949=CARTESIAN_POINT('Ctrl Pts',(0.0602028331178171,-0.143481102364144,
1.67764407956139));
#18950=CARTESIAN_POINT('Ctrl Pts',(0.0638043615254592,-0.141916235491553,
1.67793882653811));
#18951=CARTESIAN_POINT('Ctrl Pts',(0.067913959592622,-0.139942479369938,
1.67827263124267));
#18952=CARTESIAN_POINT('Ctrl Pts',(0.068483073974055,-0.139664856194405,
1.67831879968475));
#18953=CARTESIAN_POINT('Ctrl Pts',(0.0693414430730594,-0.139239621522635,
1.67838832772092));
#18954=CARTESIAN_POINT('Ctrl Pts',(0.0696319475470539,-0.139094571480213,
1.67841184020019));
#18955=CARTESIAN_POINT('Ctrl Pts',(0.0701521421251393,-0.138832798119229,
1.67845390713552));
#18956=CARTESIAN_POINT('Ctrl Pts',(0.0703819971923152,-0.138716413423375,
1.67847248218063));
#18957=CARTESIAN_POINT('Ctrl Pts',(0.0708801245158005,-0.138462635000128,
1.67851270874644));
#18958=CARTESIAN_POINT('Ctrl Pts',(0.0711482862031795,-0.138325032865015,
1.67853434692692));
#18959=CARTESIAN_POINT('Ctrl Pts',(0.0718985058007074,-0.137937312925557,
1.6785948388176));
#18960=CARTESIAN_POINT('Ctrl Pts',(0.0723796627695605,-0.137685445397633,
1.67863358460929));
#18961=CARTESIAN_POINT('Ctrl Pts',(0.0752073851927819,-0.13618631961288,
1.67886104884831));
#18962=CARTESIAN_POINT('Ctrl Pts',(0.0775231779717367,-0.134881516871162,
1.6790463491165));
#18963=CARTESIAN_POINT('Ctrl Pts',(0.0923867584467787,-0.125997451889897,
1.68023683690014));
#18964=CARTESIAN_POINT('Ctrl Pts',(0.103843963428959,-0.116735633874203,
1.68116633271599));
#18965=CARTESIAN_POINT('Ctrl Pts',(0.115172767310384,-0.104569996036062,
1.68228329354739));
#18966=CARTESIAN_POINT('Ctrl Pts',(0.116482263970444,-0.103109321267012,
1.68241585518357));
#18967=CARTESIAN_POINT('Ctrl Pts',(0.120348004786674,-0.0986296439602964,
1.68281858515854));
#18968=CARTESIAN_POINT('Ctrl Pts',(0.12281687951383,-0.0955377331799848,
1.68309153308614));
#18969=CARTESIAN_POINT('Ctrl Pts',(0.125678045156998,-0.0916601215768736,
1.6834298729078));
#18970=CARTESIAN_POINT('Ctrl Pts',(0.126185195648886,-0.0909606797874612,
1.68349074897831));
#18971=CARTESIAN_POINT('Ctrl Pts',(0.127015395210541,-0.0897953963022938,
1.68359193766495));
#18972=CARTESIAN_POINT('Ctrl Pts',(0.127341776185319,-0.089331941880324,
1.68363212225834));
#18973=CARTESIAN_POINT('Ctrl Pts',(0.127928551282849,-0.0884889828633044,
1.68370510988962));
#18974=CARTESIAN_POINT('Ctrl Pts',(0.128189809387703,-0.0881100850204399,
1.68373787959695));
#18975=CARTESIAN_POINT('Ctrl Pts',(0.128747535538402,-0.0872934937996512,
1.68380842776158));
#18976=CARTESIAN_POINT('Ctrl Pts',(0.129043460713491,-0.0868554385246392,
1.68384622618183));
#18977=CARTESIAN_POINT('Ctrl Pts',(0.129846409855484,-0.0856536786309938,
1.68394980090174));
#18978=CARTESIAN_POINT('Ctrl Pts',(0.130348917824022,-0.0848869976536648,
1.68401574503198));
#18979=CARTESIAN_POINT('Ctrl Pts',(0.132999277386099,-0.080764291726573,
1.68436969391954));
#18980=CARTESIAN_POINT('Ctrl Pts',(0.13502416931733,-0.0773314096988657,
1.68466217351912));
#18981=CARTESIAN_POINT('Ctrl Pts',(0.143909515226997,-0.0608527305361322,
1.68605747249563));
#18982=CARTESIAN_POINT('Ctrl Pts',(0.14902438131944,-0.046953113821582,
1.6872193210833));
#18983=CARTESIAN_POINT('Ctrl Pts',(0.153027406998455,-0.0282447476203451,
1.68868092412717));
#18984=CARTESIAN_POINT('Ctrl Pts',(0.153765034917613,-0.0239055639275688,
1.68901232356463));
#18985=CARTESIAN_POINT('Ctrl Pts',(0.154400573580371,-0.0188865011680879,
1.68938288971926));
#18986=CARTESIAN_POINT('Ctrl Pts',(0.154479227788622,-0.0182319848580721,
1.68943096519793));
#18987=CARTESIAN_POINT('Ctrl Pts',(0.154590527217519,-0.017253332784338,
1.68950245856718));
#18988=CARTESIAN_POINT('Ctrl Pts',(0.154626317708848,-0.0169295739653336,
1.68952604632471));
#18989=CARTESIAN_POINT('Ctrl Pts',(0.154688603530453,-0.0163494603590062,
1.68956819405555));
#18990=CARTESIAN_POINT('Ctrl Pts',(0.154715478881031,-0.0160931511633394,
1.6895867749655));
#18991=CARTESIAN_POINT('Ctrl Pts',(0.154772325683636,-0.0155376987664653,
1.68962695276701));
#18992=CARTESIAN_POINT('Ctrl Pts',(0.154802066870917,-0.0152385359251876,
1.68964853659093));
#18993=CARTESIAN_POINT('Ctrl Pts',(0.15488276067512,-0.0144022243222315,
1.68970872356026));
#18994=CARTESIAN_POINT('Ctrl Pts',(0.154931786791348,-0.0138648867450967,
1.68974722053324));
#18995=CARTESIAN_POINT('Ctrl Pts',(0.155200676341018,-0.0107380728470826,
1.6899702854882));
#18996=CARTESIAN_POINT('Ctrl Pts',(0.155358431275879,-0.00814347085545896,
1.69015158768149));
#18997=CARTESIAN_POINT('Ctrl Pts',(0.155975385435482,0.00914959567733008,
1.69134207364734));
#18998=CARTESIAN_POINT('Ctrl Pts',(0.154413352523018,0.0238466180257112,
1.69227428366037));
#18999=CARTESIAN_POINT('Ctrl Pts',(0.15034687495937,0.0399398757435825,
1.6933894720056));
#19000=CARTESIAN_POINT('Ctrl Pts',(0.149850374205536,0.0417641165950445,
1.69351718634346));
#19001=CARTESIAN_POINT('Ctrl Pts',(0.148190441517036,0.0474517992128966,
1.69392019827623));
#19002=CARTESIAN_POINT('Ctrl Pts',(0.146909960643382,0.0512790292291801,
1.69419847241471));
#19003=CARTESIAN_POINT('Ctrl Pts',(0.145174573974553,0.0558650286124685,
1.69454270902867));
#19004=CARTESIAN_POINT('Ctrl Pts',(0.144860073122485,0.0566755459689623,
1.69460396422499));
#19005=CARTESIAN_POINT('Ctrl Pts',(0.144328698412257,0.0580116587106637,
1.69470565229256));
#19006=CARTESIAN_POINT('Ctrl Pts',(0.144115704695172,0.0585387852315177,
1.69474595488943));
#19007=CARTESIAN_POINT('Ctrl Pts',(0.143725023936878,0.0594906036513178,
1.6948190683612));
#19008=CARTESIAN_POINT('Ctrl Pts',(0.143548331354511,0.0599156989898146,
1.69485184536161));
#19009=CARTESIAN_POINT('Ctrl Pts',(0.143165169928412,0.0608261027120477,
1.69492231089825));
#19010=CARTESIAN_POINT('Ctrl Pts',(0.142958115235106,0.0613111566319243,
1.69496001897018));
#19011=CARTESIAN_POINT('Ctrl Pts',(0.142386678232713,0.0626311929415151,
1.6950630946148));
#19012=CARTESIAN_POINT('Ctrl Pts',(0.142017425788805,0.0634640305538876,
1.69512862731331));
#19013=CARTESIAN_POINT('Ctrl Pts',(0.1400270637585,0.0678488653660929,1.69547635632691));
#19014=CARTESIAN_POINT('Ctrl Pts',(0.138280100457666,0.0713418241189861,
1.69576284263471));
#19015=CARTESIAN_POINT('Ctrl Pts',(0.12929312704414,0.0877379337101477,
1.69715543865748));
#19016=CARTESIAN_POINT('Ctrl Pts',(0.120368473044545,0.0996290235350693,
1.69832156987168));
#19017=CARTESIAN_POINT('Ctrl Pts',(0.106766568743113,0.113209292569439,
1.69979027804044));
#19018=CARTESIAN_POINT('Ctrl Pts',(0.103497486430046,0.116205522633102,
1.70012423338428));
#19019=CARTESIAN_POINT('Ctrl Pts',(0.0995991367852806,0.119483264264915,
1.70049730306448));
#19020=CARTESIAN_POINT('Ctrl Pts',(0.0990910336566504,0.119904985628396,
1.70054545890344));
#19021=CARTESIAN_POINT('Ctrl Pts',(0.0983281183143945,0.120530037289042,
1.70061704800486));
#19022=CARTESIAN_POINT('Ctrl Pts',(0.098075336429289,0.120735815439028,
1.70064065179217));
#19023=CARTESIAN_POINT('Ctrl Pts',(0.0976215204798244,0.121102880493464,
1.70068281677014));
#19024=CARTESIAN_POINT('Ctrl Pts',(0.0974207315975459,0.121264462985403,
1.70070139897141));
#19025=CARTESIAN_POINT('Ctrl Pts',(0.096984982316196,0.121613346260353,
1.70074156658287));
#19026=CARTESIAN_POINT('Ctrl Pts',(0.0967498811808077,0.121800465020371,
1.70076313898286));
#19027=CARTESIAN_POINT('Ctrl Pts',(0.0960916814512226,0.122321222926369,
1.70082326192739));
#19028=CARTESIAN_POINT('Ctrl Pts',(0.0956673837028532,0.122653351119015,
1.70086170666449));
#19029=CARTESIAN_POINT('Ctrl Pts',(0.0931962540677215,0.124567056451588,
1.70108386208888));
#19030=CARTESIAN_POINT('Ctrl Pts',(0.0911117975507876,0.126099705730657,
1.70126433803457));
#19031=CARTESIAN_POINT('Ctrl Pts',(0.0769212176750395,0.135997972692268,
1.70245483375188));
#19032=CARTESIAN_POINT('Ctrl Pts',(0.0637179849680319,0.142662012931959,
1.70338761203266));
#19033=CARTESIAN_POINT('Ctrl Pts',(0.0479955919389848,0.147972116324583,
1.70450249562277));
#19034=CARTESIAN_POINT('Ctrl Pts',(0.0462070074747395,0.148540351839447,
1.70462926152316));
#19035=CARTESIAN_POINT('Ctrl Pts',(0.0405270475174182,0.150232368714803,
1.70503233660449));
#19036=CARTESIAN_POINT('Ctrl Pts',(0.0366021100722138,0.15123652616071,
1.70531166074971));
#19037=CARTESIAN_POINT('Ctrl Pts',(0.0317916694146205,0.152269005188088,
1.70565705911394));
#19038=CARTESIAN_POINT('Ctrl Pts',(0.0309390982600143,0.152444522135648,
1.70571838780001));
#19039=CARTESIAN_POINT('Ctrl Pts',(0.0295269941928091,0.152722895196094,
1.70582017265145));
#19040=CARTESIAN_POINT('Ctrl Pts',(0.0289682817630957,0.152829855523179,
1.70586049810404));
#19041=CARTESIAN_POINT('Ctrl Pts',(0.0279563649510032,0.153017829381643,
1.70593363601026));
#19042=CARTESIAN_POINT('Ctrl Pts',(0.0275033614987932,0.153099900548161,
1.70596641448408));
#19043=CARTESIAN_POINT('Ctrl Pts',(0.0265308740041513,0.153271631834918,
1.70603686430812));
#19044=CARTESIAN_POINT('Ctrl Pts',(0.0260112865099643,0.15336066432507,
1.70607455511215));
#19045=CARTESIAN_POINT('Ctrl Pts',(0.0246403235618893,0.153588414389331,
1.70617414285442));
#19046=CARTESIAN_POINT('Ctrl Pts',(0.0237882399181991,0.153722692422995,
1.70623617923938));
#19047=CARTESIAN_POINT('Ctrl Pts',(0.0194753583731613,0.154365633256455,
1.70655093027577));
#19048=CARTESIAN_POINT('Ctrl Pts',(0.0159994862901673,0.15476450204419,
1.70680706561581));
#19049=CARTESIAN_POINT('Ctrl Pts',(-0.00253453420130531,0.156260337500092,
1.70818732570391));
#19050=CARTESIAN_POINT('Ctrl Pts',(-0.017677856791741,0.155277312488693,
1.70937668862919));
#19051=CARTESIAN_POINT('Ctrl Pts',(-0.0339945702669225,0.151798243479703,
1.71065271643613));
#19052=CARTESIAN_POINT('Ctrl Pts',(-0.0355466066846262,0.151442321075664,
1.71077391313104));
#19053=CARTESIAN_POINT('Ctrl Pts',(-0.0400948938486527,0.150325503416693,
1.71112809218911));
#19054=CARTESIAN_POINT('Ctrl Pts',(-0.043074476475213,0.149498998094757,
1.71135884752414));
#19055=CARTESIAN_POINT('Ctrl Pts',(-0.0465443836294818,0.14842410664082,
1.71162458566063));
#19056=CARTESIAN_POINT('Ctrl Pts',(-0.0470602389120831,0.14826135375155,
1.71166401282278));
#19057=CARTESIAN_POINT('Ctrl Pts',(-0.0478929114937225,0.147993860868635,
1.71172751517046));
#19058=CARTESIAN_POINT('Ctrl Pts',(-0.0482102530516723,0.147890788531662,
1.71175168382805));
#19059=CARTESIAN_POINT('Ctrl Pts',(-0.0487727917824953,0.147706073216984,
1.71179446527758));
#19060=CARTESIAN_POINT('Ctrl Pts',(-0.0490181190927283,0.147624839671233,
1.71181310167686));
#19061=CARTESIAN_POINT('Ctrl Pts',(-0.0495432762298786,0.147449494532381,
1.7118529500133));
#19062=CARTESIAN_POINT('Ctrl Pts',(-0.0498230402452061,0.147355197811706,
1.71187415084166));
#19063=CARTESIAN_POINT('Ctrl Pts',(-0.0505802082159241,0.147097585359871,
1.71193146008684));
#19064=CARTESIAN_POINT('Ctrl Pts',(-0.0510570944556044,0.146932740417311,
1.71196747978987));
#19065=CARTESIAN_POINT('Ctrl Pts',(-0.0535251601482233,0.146066138891908,
1.71215354612816));
#19066=CARTESIAN_POINT('Ctrl Pts',(-0.0555028290526461,0.145326174028104,
1.71230146085976));
#19067=CARTESIAN_POINT('Ctrl Pts',(-0.0595584335563164,0.143713850590068,
1.71260355222163));
#19068=CARTESIAN_POINT('Ctrl Pts',(-0.0616334814827387,0.142836237505129,
1.71275743129292));
#19069=CARTESIAN_POINT('Ctrl Pts',(-0.0636886260955797,0.141913922523681,
1.71290984779881));
#19070=CARTESIAN_POINT('Origin',(0.,0.,-0.129405622560373));
#19071=CARTESIAN_POINT('',(-0.0636886042805274,0.141913932313915,1.79664456958818));
#19072=CARTESIAN_POINT('',(-0.0636886300450479,0.141913920751225,1.78267615293977));
#19073=CARTESIAN_POINT('',(-0.0636886258329924,0.141913922641526,-0.129405622560373));
#19074=CARTESIAN_POINT('Ctrl Pts',(-0.0636886042805435,0.141913932313908,
1.79664456958818));
#19075=CARTESIAN_POINT('Ctrl Pts',(-0.0614297561867433,0.142927665638256,
1.79648079782229));
#19076=CARTESIAN_POINT('Ctrl Pts',(-0.059145515988598,0.143888001777509,
1.79631627691133));
#19077=CARTESIAN_POINT('Ctrl Pts',(-0.0527327728000258,0.146405273857401,
1.7958556637672));
#19078=CARTESIAN_POINT('Ctrl Pts',(-0.0485614736293651,0.147841224542857,
1.79555741037763));
#19079=CARTESIAN_POINT('Ctrl Pts',(-0.0417739006076907,0.149859545289724,
1.79506972800745));
#19080=CARTESIAN_POINT('Ctrl Pts',(-0.0391936775312136,0.150554960846653,
1.79488382624486));
#19081=CARTESIAN_POINT('Ctrl Pts',(-0.0358163629284328,0.151372506336316,
1.79463925097973));
#19082=CARTESIAN_POINT('Ctrl Pts',(-0.0350343331617838,0.15155541225724,
1.79458253373647));
#19083=CARTESIAN_POINT('Ctrl Pts',(-0.0337596684824227,0.151843145793434,
1.79448993421611));
#19084=CARTESIAN_POINT('Ctrl Pts',(-0.0332678716153356,0.151951652994638,
1.79445417001827));
#19085=CARTESIAN_POINT('Ctrl Pts',(-0.0323207632470261,0.152155799149134,
1.79438521960791));
#19086=CARTESIAN_POINT('Ctrl Pts',(-0.031865531871939,0.15225178758049,
1.79435204496081));
#19087=CARTESIAN_POINT('Ctrl Pts',(-0.0308218024391521,0.15246697849679,
1.79427590406428));
#19088=CARTESIAN_POINT('Ctrl Pts',(-0.0302330342769231,0.152584817911995,
1.7942328949001));
#19089=CARTESIAN_POINT('Ctrl Pts',(-0.0286662985969709,0.152888969355366,
1.79411828366799));
#19090=CARTESIAN_POINT('Ctrl Pts',(-0.0276872138123964,0.153069303687585,
1.79404649315364));
#19091=CARTESIAN_POINT('Ctrl Pts',(-0.0202760461716728,0.154360911349842,
1.7935017247999));
#19092=CARTESIAN_POINT('Ctrl Pts',(-0.0137824124696716,0.155075567007255,
1.79301630472144));
#19093=CARTESIAN_POINT('Ctrl Pts',(0.00413527026421228,0.155913203716126,
1.79165419749622));
#19094=CARTESIAN_POINT('Ctrl Pts',(0.0155582255594549,0.155189985203871,
1.79075829529241));
#19095=CARTESIAN_POINT('Ctrl Pts',(0.0300745935375249,0.15265119873261,
1.78962949936132));
#19096=CARTESIAN_POINT('Ctrl Pts',(0.0333326124151484,0.151973056529895,
1.78937708450784));
#19097=CARTESIAN_POINT('Ctrl Pts',(0.0377435759024,0.150906233401039,1.78903863983636));
#19098=CARTESIAN_POINT('Ctrl Pts',(0.0389172324148559,0.150607828637981,
1.78894891178945));
#19099=CARTESIAN_POINT('Ctrl Pts',(0.0406607787106198,0.150142784755903,
1.78881621507753));
#19100=CARTESIAN_POINT('Ctrl Pts',(0.0412333609081846,0.149986548454196,
1.78877273446958));
#19101=CARTESIAN_POINT('Ctrl Pts',(0.0422668048210996,0.149698194814547,
1.78869444982059));
#19102=CARTESIAN_POINT('Ctrl Pts',(0.0427279731440021,0.149567217824945,
1.78865958543256));
#19103=CARTESIAN_POINT('Ctrl Pts',(0.0434506720264532,0.149358347791677,
1.78860506662737));
#19104=CARTESIAN_POINT('Ctrl Pts',(0.0437126102944892,0.149281896621743,
1.7885853308385));
#19105=CARTESIAN_POINT('Ctrl Pts',(0.0442216398803071,0.149131872955087,
1.78854702692104));
#19106=CARTESIAN_POINT('Ctrl Pts',(0.0444687467635335,0.149058376242083,
1.78852845518331));
#19107=CARTESIAN_POINT('Ctrl Pts',(0.0450278572064945,0.148890566563971,
1.78848648491731));
#19108=CARTESIAN_POINT('Ctrl Pts',(0.0453397471599194,0.148795887272133,
1.78846310802776));
#19109=CARTESIAN_POINT('Ctrl Pts',(0.0462822324077931,0.148506541947426,
1.78839256738333));
#19110=CARTESIAN_POINT('Ctrl Pts',(0.0469118997549415,0.14830883905122,
1.7883455765265));
#19111=CARTESIAN_POINT('Ctrl Pts',(0.0517460803809523,0.146757135091929,
1.78798572640871));
#19112=CARTESIAN_POINT('Ctrl Pts',(0.0558929478068463,0.145228444324451,
1.78768236493972));
#19113=CARTESIAN_POINT('Ctrl Pts',(0.0736088245304174,0.137826161752135,
1.78638659755108));
#19114=CARTESIAN_POINT('Ctrl Pts',(0.0863661990675227,0.130212281457774,
1.78544670842502));
#19115=CARTESIAN_POINT('Ctrl Pts',(0.100909341190346,0.118442048586702,
1.78417225536528));
#19116=CARTESIAN_POINT('Ctrl Pts',(0.103866059720712,0.115857892080291,
1.78390114102821));
#19117=CARTESIAN_POINT('Ctrl Pts',(0.107385717028277,0.112538630610634,
1.78356122697175));
#19118=CARTESIAN_POINT('Ctrl Pts',(0.108044213586633,0.111906583579372,
1.78349685436312));
#19119=CARTESIAN_POINT('Ctrl Pts',(0.109074706407254,0.110899907956114,
1.7833948560023));
#19120=CARTESIAN_POINT('Ctrl Pts',(0.109450431117544,0.110529110546453,
1.78335739729049));
#19121=CARTESIAN_POINT('Ctrl Pts',(0.110150354307671,0.109831297836998,
1.78328710527739));
#19122=CARTESIAN_POINT('Ctrl Pts',(0.110475003153329,0.109504740575762,
1.78325429240209));
#19123=CARTESIAN_POINT('Ctrl Pts',(0.111197065875754,0.108771954100905,
1.78318083978658));
#19124=CARTESIAN_POINT('Ctrl Pts',(0.111593711400995,0.108364980589715,
1.78314016708753));
#19125=CARTESIAN_POINT('Ctrl Pts',(0.112590742517728,0.107330709302985,
1.7830371009355));
#19126=CARTESIAN_POINT('Ctrl Pts',(0.113188115343678,0.106700548022423,
1.782974578727));
#19127=CARTESIAN_POINT('Ctrl Pts',(0.116518547812333,0.103127874327755,
1.782621595668));
#19128=CARTESIAN_POINT('Ctrl Pts',(0.119141881637525,0.100085648283759,
1.7823265618551));
#19129=CARTESIAN_POINT('Ctrl Pts',(0.122832787030665,0.0954544124569725,
1.78188481960353));
#19130=CARTESIAN_POINT('Ctrl Pts',(0.123993630577599,0.0939415641716582,
1.78174162531866));
#19131=CARTESIAN_POINT('Ctrl Pts',(0.133870792564449,0.0805672292569739,
1.78048542063198));
#19132=CARTESIAN_POINT('Ctrl Pts',(0.140889114517399,0.0675473692591731,
1.77931813274184));
#19133=CARTESIAN_POINT('Ctrl Pts',(0.146868830591789,0.0513037026695924,
1.77801600318244));
#19134=CARTESIAN_POINT('Ctrl Pts',(0.147703536442457,0.0488486517205632,
1.7778233163896));
#19135=CARTESIAN_POINT('Ctrl Pts',(0.148637317158402,0.0458589280376593,
1.77759450845042));
#19136=CARTESIAN_POINT('Ctrl Pts',(0.148795419061345,0.0453433194896637,
1.77755525594162));
#19137=CARTESIAN_POINT('Ctrl Pts',(0.149037477146129,0.0445390086004645,
1.77749435911389));
#19138=CARTESIAN_POINT('Ctrl Pts',(0.149123281222634,0.0442508743729996,
1.77747261016086));
#19139=CARTESIAN_POINT('Ctrl Pts',(0.149281114213581,0.043715190782248,
1.77743230153753));
#19140=CARTESIAN_POINT('Ctrl Pts',(0.149353362345588,0.0434677135802262,
1.7774137296516));
#19141=CARTESIAN_POINT('Ctrl Pts',(0.149515568406769,0.0429069173957601,
1.77737175704667));
#19142=CARTESIAN_POINT('Ctrl Pts',(0.149605156767253,0.0425934951645332,
1.77734837797657));
#19143=CARTESIAN_POINT('Ctrl Pts',(0.149873182732766,0.041644535510489,
1.77727782424821));
#19144=CARTESIAN_POINT('Ctrl Pts',(0.1500485638648,0.0410081304618911,1.77723082258238));
#19145=CARTESIAN_POINT('Ctrl Pts',(0.151367495790153,0.0361003572884876,
1.77687063369835));
#19146=CARTESIAN_POINT('Ctrl Pts',(0.152332630229546,0.031782597305135,
1.77656696448232));
#19147=CARTESIAN_POINT('Ctrl Pts',(0.155720548205868,0.0128708290260328,
1.77527039341198));
#19148=CARTESIAN_POINT('Ctrl Pts',(0.156239098195963,-0.001984978289228,
1.77433000466234));
#19149=CARTESIAN_POINT('Ctrl Pts',(0.154231853951435,-0.0205830012752516,
1.77305566313613));
#19150=CARTESIAN_POINT('Ctrl Pts',(0.153665108098895,-0.0244572036581431,
1.77278531792012));
#19151=CARTESIAN_POINT('Ctrl Pts',(0.152786964628181,-0.0292023553823572,
1.77244625671808));
#19152=CARTESIAN_POINT('Ctrl Pts',(0.152613139939519,-0.0300975675878516,
1.7723819407683));
#19153=CARTESIAN_POINT('Ctrl Pts',(0.152326318839247,-0.0315083094250501,
1.77228001194332));
#19154=CARTESIAN_POINT('Ctrl Pts',(0.152218551002129,-0.0320248917604507,
1.77224256572046));
#19155=CARTESIAN_POINT('Ctrl Pts',(0.152011822993217,-0.0329912143564052,
1.77217228489697));
#19156=CARTESIAN_POINT('Ctrl Pts',(0.151913489960272,-0.0334410842250751,
1.77213947066084));
#19157=CARTESIAN_POINT('Ctrl Pts',(0.151689291382762,-0.0344453859752673,
1.77206599911256));
#19158=CARTESIAN_POINT('Ctrl Pts',(0.151562381368257,-0.034999575330341,
1.77202530876318));
#19159=CARTESIAN_POINT('Ctrl Pts',(0.15123379420906,-0.0363991389352862,
1.77192216807315));
#19160=CARTESIAN_POINT('Ctrl Pts',(0.151028067204055,-0.0372435321326472,
1.77185958865131));
#19161=CARTESIAN_POINT('Ctrl Pts',(0.149829145972329,-0.0419910763485591,
1.77150570836117));
#19162=CARTESIAN_POINT('Ctrl Pts',(0.148691818572973,-0.0458558722880187,
1.77120980727176));
#19163=CARTESIAN_POINT('Ctrl Pts',(0.146800331638623,-0.0514690357844124,
1.77076793398806));
#19164=CARTESIAN_POINT('Ctrl Pts',(0.146161945132119,-0.0532548992426505,
1.77062551044896));
#19165=CARTESIAN_POINT('Ctrl Pts',(0.140281243814903,-0.068802994596929,
1.76936952347799));
#19166=CARTESIAN_POINT('Ctrl Pts',(0.133142695530272,-0.0817656667338998,
1.76820162548707));
#19167=CARTESIAN_POINT('Ctrl Pts',(0.122735797628334,-0.0955949843381436,
1.76689974540649));
#19168=CARTESIAN_POINT('Ctrl Pts',(0.121131040660769,-0.0976204392709824,
1.76670773615539));
#19169=CARTESIAN_POINT('Ctrl Pts',(0.119131466240921,-0.10001893068078,
1.76647962418861));
#19170=CARTESIAN_POINT('Ctrl Pts',(0.118784332818932,-0.100430946640481,
1.76644041187204));
#19171=CARTESIAN_POINT('Ctrl Pts',(0.118240238495962,-0.101069969871784,
1.76637956371951));
#19172=CARTESIAN_POINT('Ctrl Pts',(0.118044753159109,-0.101298218470267,
1.76635782351474));
#19173=CARTESIAN_POINT('Ctrl Pts',(0.117680327458635,-0.101721234270261,
1.76631752281045));
#19174=CARTESIAN_POINT('Ctrl Pts',(0.117511566036504,-0.101916146030575,
1.76629895013822));
#19175=CARTESIAN_POINT('Ctrl Pts',(0.117128227505168,-0.102356666532666,
1.76625696519708));
#19176=CARTESIAN_POINT('Ctrl Pts',(0.116913362512068,-0.102602020124317,
1.76623357463067));
#19177=CARTESIAN_POINT('Ctrl Pts',(0.116260740110817,-0.103342535376414,
1.76616295189995));
#19178=CARTESIAN_POINT('Ctrl Pts',(0.115820589321804,-0.103835593319316,
1.76611589322625));
#19179=CARTESIAN_POINT('Ctrl Pts',(0.112395106378392,-0.107623944885169,
1.76575390418718));
#19180=CARTESIAN_POINT('Ctrl Pts',(0.109272509583499,-0.110793056565655,
1.76544859960747));
#19181=CARTESIAN_POINT('Ctrl Pts',(0.0951632378153099,-0.123934686704193,
1.76414767363625));
#19182=CARTESIAN_POINT('Ctrl Pts',(0.0829181456910517,-0.132440467940152,
1.76320455285298));
#19183=CARTESIAN_POINT('Ctrl Pts',(0.0662080847190203,-0.140808864601828,
1.76193077465562));
#19184=CARTESIAN_POINT('Ctrl Pts',(0.0627004738156415,-0.14240538316404,
1.7616645856437));
#19185=CARTESIAN_POINT('Ctrl Pts',(0.058298099649379,-0.144214970203719,
1.76133013486416));
#19186=CARTESIAN_POINT('Ctrl Pts',(0.0574557570431828,-0.144552627004233,
1.76126612837196));
#19187=CARTESIAN_POINT('Ctrl Pts',(0.0561199150854454,-0.145074584526248,
1.76116457936147));
#19188=CARTESIAN_POINT('Ctrl Pts',(0.0556283413968665,-0.145263786146715,
1.76112720138286));
#19189=CARTESIAN_POINT('Ctrl Pts',(0.0547051359064052,-0.145613745056728,
1.76105698143769));
#19190=CARTESIAN_POINT('Ctrl Pts',(0.0542737314389346,-0.145775089474504,
1.76102415949882));
#19191=CARTESIAN_POINT('Ctrl Pts',(0.0533069661870855,-0.146131771433182,
1.76095058321685));
#19192=CARTESIAN_POINT('Ctrl Pts',(0.052771238087427,-0.146326086809594,
1.76090979540374));
#19193=CARTESIAN_POINT('Ctrl Pts',(0.0514117408556365,-0.146810756752664,
1.76080624289936));
#19194=CARTESIAN_POINT('Ctrl Pts',(0.0505865810045376,-0.147097121523561,
1.76074334732105));
#19195=CARTESIAN_POINT('Ctrl Pts',(0.0458839497237457,-0.148684881624701,
1.76038461023037));
#19196=CARTESIAN_POINT('Ctrl Pts',(0.041959105488379,-0.14983977620702,
1.76008401985359));
#19197=CARTESIAN_POINT('Ctrl Pts',(0.0257902264300201,-0.153912437759099,
1.75883952410253));
#19198=CARTESIAN_POINT('Ctrl Pts',(0.0132601626775284,-0.155493560898368,
1.75785586721246));
#19199=CARTESIAN_POINT('Ctrl Pts',(-0.00371418171453799,-0.155567708351024,
1.75654666089774));
#19200=CARTESIAN_POINT('Ctrl Pts',(-0.00810704462424373,-0.155400737191817,
1.75621055179108));
#19201=CARTESIAN_POINT('Ctrl Pts',(-0.0146755064276768,-0.154871725841464,
1.75571692940235));
#19202=CARTESIAN_POINT('Ctrl Pts',(-0.01685992661398,-0.154649171268608,
1.75555427434402));
#19203=CARTESIAN_POINT('Ctrl Pts',(-0.0195477958919771,-0.154317688341038,
1.75535656312287));
#19204=CARTESIAN_POINT('Ctrl Pts',(-0.0200562385351817,-0.154252431342088,
1.75531927150631));
#19205=CARTESIAN_POINT('Ctrl Pts',(-0.0208565449046498,-0.154145690585219,
1.75526075277204));
#19206=CARTESIAN_POINT('Ctrl Pts',(-0.0211486228915669,-0.154105889391339,
1.75523943363137));
#19207=CARTESIAN_POINT('Ctrl Pts',(-0.0216967268285729,-0.154029612159401,
1.7551994998784));
#19208=CARTESIAN_POINT('Ctrl Pts',(-0.0219527718555892,-0.153993328382706,
1.75518087518737));
#19209=CARTESIAN_POINT('Ctrl Pts',(-0.0225399509756017,-0.153908625812204,
1.75513823183764));
#19210=CARTESIAN_POINT('Ctrl Pts',(-0.0228710198485558,-0.153859776894972,
1.75511423768703));
#19211=CARTESIAN_POINT('Ctrl Pts',(-0.0238981897699672,-0.153704830212752,
1.755039939928));
#19212=CARTESIAN_POINT('Ctrl Pts',(-0.024593743258209,-0.153595072016359,
1.75498983738828));
#19213=CARTESIAN_POINT('Ctrl Pts',(-0.03261523520254,-0.152273394418483,
1.75441418523699));
#19214=CARTESIAN_POINT('Ctrl Pts',(-0.0398473069998486,-0.1505429092258,
1.75391579057767));
#19215=CARTESIAN_POINT('Ctrl Pts',(-0.0486997482833774,-0.147741620341379,
1.75330080075456));
#19216=CARTESIAN_POINT('Ctrl Pts',(-0.0504602974047382,-0.147149619128453,
1.75317825574012));
#19217=CARTESIAN_POINT('Ctrl Pts',(-0.0610314623959728,-0.143382929269549,
1.75243886850096));
#19218=CARTESIAN_POINT('Ctrl Pts',(-0.0695505348139731,-0.139449670314694,
1.75182651991915));
#19219=CARTESIAN_POINT('Ctrl Pts',(-0.0814260692977656,-0.13260637965032,
1.75089594662155));
#19220=CARTESIAN_POINT('Ctrl Pts',(-0.0850955006778522,-0.130282026716384,
1.75059677779658));
#19221=CARTESIAN_POINT('Ctrl Pts',(-0.0894355041149582,-0.12727127664727,
1.75022581498615));
#19222=CARTESIAN_POINT('Ctrl Pts',(-0.0902034640843575,-0.126728143099933,
1.75015949745554));
#19223=CARTESIAN_POINT('Ctrl Pts',(-0.091399601169933,-0.125865803774084,
1.75005511316914));
#19224=CARTESIAN_POINT('Ctrl Pts',(-0.0918311503139302,-0.125551294190099,
1.75001722701113));
#19225=CARTESIAN_POINT('Ctrl Pts',(-0.0925941831546651,-0.124989163282781,
1.74994983269994));
#19226=CARTESIAN_POINT('Ctrl Pts',(-0.0929263162411565,-0.124742428371377,
1.74992035914783));
#19227=CARTESIAN_POINT('Ctrl Pts',(-0.093690262986942,-0.124170163700927,
1.74985224417579));
#19228=CARTESIAN_POINT('Ctrl Pts',(-0.0941213691942,-0.123843703027014,
1.74981356661273));
#19229=CARTESIAN_POINT('Ctrl Pts',(-0.0953015517344583,-0.122940273070961,
1.74970701764101));
#19230=CARTESIAN_POINT('Ctrl Pts',(-0.0960470724287772,-0.122358719796578,
1.74963896622906));
#19231=CARTESIAN_POINT('Ctrl Pts',(-0.0998545441082448,-0.119332413049575,
1.74928750901641));
#19232=CARTESIAN_POINT('Ctrl Pts',(-0.102828366574918,-0.116779607382737,
1.74899980343514));
#19233=CARTESIAN_POINT('Ctrl Pts',(-0.107166286715345,-0.112761566433556,
1.74855910185614));
#19234=CARTESIAN_POINT('Ctrl Pts',(-0.108603860203675,-0.111377667502997,
1.74840932632836));
#19235=CARTESIAN_POINT('Ctrl Pts',(-0.120380034043979,-0.0995963734766138,
1.74715092626957));
#19236=CARTESIAN_POINT('Ctrl Pts',(-0.129225898037721,-0.0878144591943174,
1.74598848002336));
#19237=CARTESIAN_POINT('Ctrl Pts',(-0.137575586934046,-0.0726351137692201,
1.74468428046566));
#19238=CARTESIAN_POINT('Ctrl Pts',(-0.138799677234858,-0.0702677293479703,
1.74448613123363));
#19239=CARTESIAN_POINT('Ctrl Pts',(-0.140199622447735,-0.0673807382183866,
1.74425172095393));
#19240=CARTESIAN_POINT('Ctrl Pts',(-0.140434252619785,-0.0668903485727644,
1.74421215051362));
#19241=CARTESIAN_POINT('Ctrl Pts',(-0.140795044273981,-0.0661260081715274,
1.74415086876003));
#19242=CARTESIAN_POINT('Ctrl Pts',(-0.140922984900632,-0.0658529101842299,
1.74412905070382));
#19243=CARTESIAN_POINT('Ctrl Pts',(-0.141158785723988,-0.0653457430306535,
1.7440886791461));
#19244=CARTESIAN_POINT('Ctrl Pts',(-0.141266857434217,-0.0651117801313446,
1.74407011309058));
#19245=CARTESIAN_POINT('Ctrl Pts',(-0.141509780469074,-0.0645824276924301,
1.74402823619718));
#19246=CARTESIAN_POINT('Ctrl Pts',(-0.141644288367612,-0.0642868844563697,
1.74400494659083));
#19247=CARTESIAN_POINT('Ctrl Pts',(-0.14203826023097,-0.0634140029055581,
1.74393642199687));
#19248=CARTESIAN_POINT('Ctrl Pts',(-0.142295131171779,-0.0628354900950748,
1.7438913420529));
#19249=CARTESIAN_POINT('Ctrl Pts',(-0.144115399130699,-0.0586675566993679,
1.74356885058617));
#19250=CARTESIAN_POINT('Ctrl Pts',(-0.145546485575233,-0.0550214285575594,
1.7432988846673));
#19251=CARTESIAN_POINT('Ctrl Pts',(-0.147503303763815,-0.0494230355989775,
1.74289682713822));
#19252=CARTESIAN_POINT('Ctrl Pts',(-0.148131046112163,-0.0475084708582904,
1.7427614784464));
#19253=CARTESIAN_POINT('Ctrl Pts',(-0.152286772020839,-0.0339495446450549,
1.741814519695));
#19254=CARTESIAN_POINT('Ctrl Pts',(-0.154474985958918,-0.0219390321530172,
1.74103177607834));
#19255=CARTESIAN_POINT('Ctrl Pts',(-0.15544609479793,-0.00654950058985834,
1.7399894607761));
#19256=CARTESIAN_POINT('Ctrl Pts',(-0.155549053882137,-0.00329755167798682,
1.73976727166252));
#19257=CARTESIAN_POINT('Ctrl Pts',(-0.155550109736665,0.000357396774194728,
1.73951423103283));
#19258=CARTESIAN_POINT('Ctrl Pts',(-0.155548665002922,0.000759725169547559,
1.73948633212019));
#19259=CARTESIAN_POINT('Ctrl Pts',(-0.155532254608223,0.00295634915230469,
1.73933375698741));
#19260=CARTESIAN_POINT('Ctrl Pts',(-0.155487803810492,0.00475022358437416,
1.7392082315102));
#19261=CARTESIAN_POINT('Ctrl Pts',(-0.155382355293907,0.00725493685538521,
1.73903149831066));
#19262=CARTESIAN_POINT('Ctrl Pts',(-0.15534748395943,0.00796678369735155,
1.73898110474304));
#19263=CARTESIAN_POINT('Ctrl Pts',(-0.155283416033973,0.00911334238682362,
1.73889965944689));
#19264=CARTESIAN_POINT('Ctrl Pts',(-0.155257282486212,0.00954822143587498,
1.73886870368154));
#19265=CARTESIAN_POINT('Ctrl Pts',(-0.155199240457862,0.0104507399107341,
1.73880432378887));
#19266=CARTESIAN_POINT('Ctrl Pts',(-0.15516704451143,0.0109183557425694,
1.73877089098723));
#19267=CARTESIAN_POINT('Ctrl Pts',(-0.155086412699842,0.0120169713761962,
1.73869216148284));
#19268=CARTESIAN_POINT('Ctrl Pts',(-0.155036238829405,0.0126478311529641,
1.73864681084841));
#19269=CARTESIAN_POINT('Ctrl Pts',(-0.154859438128438,0.0147114118553243,
1.73849799092978));
#19270=CARTESIAN_POINT('Ctrl Pts',(-0.154716792603448,0.016142646757619,
1.73839402280467));
#19271=CARTESIAN_POINT('Ctrl Pts',(-0.15387559904101,0.0235415007387464,
1.73785249273175));
#19272=CARTESIAN_POINT('Ctrl Pts',(-0.152851654066885,0.029466194238073,
1.73740485654255));
#19273=CARTESIAN_POINT('Ctrl Pts',(-0.14866079573209,0.0474427755649512,
1.73600321158561));
#19274=CARTESIAN_POINT('Ctrl Pts',(-0.144388304701991,0.0591846610049198,
1.73502235396061));
#19275=CARTESIAN_POINT('Ctrl Pts',(-0.137023622434677,0.0737233545624012,
1.73378210400021));
#19276=CARTESIAN_POINT('Ctrl Pts',(-0.135158024795964,0.0770903411674165,
1.73349332339123));
#19277=CARTESIAN_POINT('Ctrl Pts',(-0.13284354065872,0.080924616152256,
1.73316542085292));
#19278=CARTESIAN_POINT('Ctrl Pts',(-0.132514523738763,0.0814622662888544,
1.73311946488892));
#19279=CARTESIAN_POINT('Ctrl Pts',(-0.132011371080237,0.0822733582114227,
1.73305018874747));
#19280=CARTESIAN_POINT('Ctrl Pts',(-0.131839639273269,0.0825482712561308,
1.73302671735105));
#19281=CARTESIAN_POINT('Ctrl Pts',(-0.131529845980388,0.0830407641754954,
1.73298468884172));
#19282=CARTESIAN_POINT('Ctrl Pts',(-0.131392102794995,0.0832585384511001,
1.73296611135214));
#19283=CARTESIAN_POINT('Ctrl Pts',(-0.131091741687671,0.0837308125575096,
1.73292583892584));
#19284=CARTESIAN_POINT('Ctrl Pts',(-0.130928923996588,0.0839851806902346,
1.73290415751868));
#19285=CARTESIAN_POINT('Ctrl Pts',(-0.130469887999167,0.0846977479744231,
1.73284344255255));
#19286=CARTESIAN_POINT('Ctrl Pts',(-0.130171994269653,0.0851548713704573,
1.73280451815436));
#19287=CARTESIAN_POINT('Ctrl Pts',(-0.12838655454332,0.0878633975707241,
1.7325739748399));
#19288=CARTESIAN_POINT('Ctrl Pts',(-0.126842916780531,0.0900775269508181,
1.732385882531));
#19289=CARTESIAN_POINT('Ctrl Pts',(-0.116564191198058,0.10403225749559,
1.73119491717937));
#19290=CARTESIAN_POINT('Ctrl Pts',(-0.106266314764755,0.114531636572013,
1.73026691320409));
#19291=CARTESIAN_POINT('Ctrl Pts',(-0.0930327779010258,0.124679051186721,
1.72914628381507));
#19292=CARTESIAN_POINT('Ctrl Pts',(-0.0913898172430544,0.125888301145483,
1.72900838379073));
#19293=CARTESIAN_POINT('Ctrl Pts',(-0.0865626836008204,0.129296858176909,
1.72860590125256));
#19294=CARTESIAN_POINT('Ctrl Pts',(-0.0833198339825612,0.13140995661346,
1.72833875754766));
#19295=CARTESIAN_POINT('Ctrl Pts',(-0.0791943083075496,0.133884093862236,
1.7280009725506));
#19296=CARTESIAN_POINT('Ctrl Pts',(-0.0783824512172755,0.134361007473451,
1.7279345995908));
#19297=CARTESIAN_POINT('Ctrl Pts',(-0.0770983746296638,0.135099720892583,
1.72782975079831));
#19298=CARTESIAN_POINT('Ctrl Pts',(-0.0766290262744205,0.135366488743217,
1.72779145417624));
#19299=CARTESIAN_POINT('Ctrl Pts',(-0.0757975150310976,0.135833392159041,
1.72772364974976));
#19300=CARTESIAN_POINT('Ctrl Pts',(-0.0754359223462922,0.13603453724704,
1.72769417843668));
#19301=CARTESIAN_POINT('Ctrl Pts',(-0.0746050829093937,0.136492381437273,
1.72762649160836));
#19302=CARTESIAN_POINT('Ctrl Pts',(-0.0741353083437456,0.136748106494806,
1.72758824186227));
#19303=CARTESIAN_POINT('Ctrl Pts',(-0.0728322608673699,0.137448741583128,
1.72748219994082));
#19304=CARTESIAN_POINT('Ctrl Pts',(-0.071996252046468,0.137888485392943,
1.72741422635685));
#19305=CARTESIAN_POINT('Ctrl Pts',(-0.0686990227952293,0.139584680263499,
1.72714633417309));
#19306=CARTESIAN_POINT('Ctrl Pts',(-0.0662089069558742,0.140782862098249,
1.72694443215555));
#19307=CARTESIAN_POINT('Ctrl Pts',(-0.0636886248462869,0.141913923084343,
1.72674034350975));
#19308=CARTESIAN_POINT('',(-0.155549931058622,0.000140704823091921,1.72557622542367));
#19309=CARTESIAN_POINT('Ctrl Pts',(-0.0636886260955797,0.141913922523681,
1.71290984779881));
#19310=CARTESIAN_POINT('Ctrl Pts',(-0.0654236273732955,0.141135282586974,
1.71303852138742));
#19311=CARTESIAN_POINT('Ctrl Pts',(-0.0671444433123963,0.140324783043432,
1.71316615252523));
#19312=CARTESIAN_POINT('Ctrl Pts',(-0.0772688368385502,0.135327275048561,
1.71391956536969));
#19313=CARTESIAN_POINT('Ctrl Pts',(-0.0852940727414064,0.130418076052826,
1.71452828255038));
#19314=CARTESIAN_POINT('Ctrl Pts',(-0.0987184873531856,0.120434032958858,
1.71564217942489));
#19315=CARTESIAN_POINT('Ctrl Pts',(-0.104290828069218,0.115642100442611,
1.71613933078241));
#19316=CARTESIAN_POINT('Ctrl Pts',(-0.110224802971553,0.109760313978326,
1.71672455251474));
#19317=CARTESIAN_POINT('Ctrl Pts',(-0.110938992223859,0.109038404393045,
1.71679597868351));
#19318=CARTESIAN_POINT('Ctrl Pts',(-0.112068134301731,0.107874479070005,
1.71691053600853));
#19319=CARTESIAN_POINT('Ctrl Pts',(-0.112487669015793,0.107436931550854,
1.71695346771157));
#19320=CARTESIAN_POINT('Ctrl Pts',(-0.113225180465223,0.106658699474202,
1.71702959980754));
#19321=CARTESIAN_POINT('Ctrl Pts',(-0.113544205895162,0.106319015062676,
1.71706275459873));
#19322=CARTESIAN_POINT('Ctrl Pts',(-0.114202917058564,0.105611301785401,
1.71713167813114));
#19323=CARTESIAN_POINT('Ctrl Pts',(-0.114542360901767,0.10524305619718,
1.7171674566231));
#19324=CARTESIAN_POINT('Ctrl Pts',(-0.115225048223495,0.104495227917897,
1.7172399485924));
#19325=CARTESIAN_POINT('Ctrl Pts',(-0.115568208460668,0.104115577976137,
1.7172766649682));
#19326=CARTESIAN_POINT('Ctrl Pts',(-0.116953931359989,0.10256721343367,
1.71742607025569));
#19327=CARTESIAN_POINT('Ctrl Pts',(-0.117980655635431,0.101384515062276,
1.71753941478281));
#19328=CARTESIAN_POINT('Ctrl Pts',(-0.123146891222748,0.0952486934955429,
1.71812372408852));
#19329=CARTESIAN_POINT('Ctrl Pts',(-0.126992474937705,0.0900575395294839,
1.71860627911308));
#19330=CARTESIAN_POINT('Ctrl Pts',(-0.133269256976991,0.0803799065816245,
1.71948534075563));
#19331=CARTESIAN_POINT('Ctrl Pts',(-0.135823658657544,0.0759838961843065,
1.71987771314208));
#19332=CARTESIAN_POINT('Ctrl Pts',(-0.142660297122646,0.0627682207319928,
1.72103098931182));
#19333=CARTESIAN_POINT('Ctrl Pts',(-0.146330456601708,0.0536586167239064,
1.72179451302398));
#19334=CARTESIAN_POINT('Ctrl Pts',(-0.1494467083144,0.0431602601280605,
1.72260396684577));
#19335=CARTESIAN_POINT('Ctrl Pts',(-0.149761922609095,0.0420534591620181,
1.72268844091508));
#19336=CARTESIAN_POINT('Ctrl Pts',(-0.150175685682622,0.0405369372520968,
1.72280291723953));
#19337=CARTESIAN_POINT('Ctrl Pts',(-0.150284885609153,0.0401302008553649,
1.72283349616439));
#19338=CARTESIAN_POINT('Ctrl Pts',(-0.15045553121994,0.0394841319253197,
1.72288186642966));
#19339=CARTESIAN_POINT('Ctrl Pts',(-0.150518059737978,0.0392450919686247,
1.72289971924773));
#19340=CARTESIAN_POINT('Ctrl Pts',(-0.150645789894482,0.0387519971155168,
1.72293645469024));
#19341=CARTESIAN_POINT('Ctrl Pts',(-0.150710918551079,0.0384979262306401,
1.72295533263976));
#19342=CARTESIAN_POINT('Ctrl Pts',(-0.150864150120947,0.0378938121398273,
1.72300010240695));
#19343=CARTESIAN_POINT('Ctrl Pts',(-0.150951678573044,0.0375436217391715,
1.72302596122048));
#19344=CARTESIAN_POINT('Ctrl Pts',(-0.151134419985444,0.03680152504019,
1.72308056845939));
#19345=CARTESIAN_POINT('Ctrl Pts',(-0.151229329620691,0.0364095457484073,
1.72310929990258));
#19346=CARTESIAN_POINT('Ctrl Pts',(-0.151485282034299,0.0353341867975488,
1.7231878255408));
#19347=CARTESIAN_POINT('Ctrl Pts',(-0.151643226805986,0.0346500684072558,
1.72323745429586));
#19348=CARTESIAN_POINT('Ctrl Pts',(-0.154280640908645,0.0228628859446989,
1.72408729525527));
#19349=CARTESIAN_POINT('Ctrl Pts',(-0.155539639183238,0.0115203149781142,
1.7248266954542));
#19350=CARTESIAN_POINT('Ctrl Pts',(-0.1555499363173,0.000140753984132637,
1.72557621298977));
#19351=CARTESIAN_POINT('Ctrl Pts',(-0.155549936362318,0.000140704224764531,
1.72557621626718));
#19352=CARTESIAN_POINT('Ctrl Pts',(-0.155557231474537,-0.00792411574282843,
1.72610740759547));
#19353=CARTESIAN_POINT('Ctrl Pts',(-0.154937332086665,-0.0159767149073688,
1.72664147358767));
#19354=CARTESIAN_POINT('Ctrl Pts',(-0.153271235507139,-0.0266710360606433,
1.72738304732705));
#19355=CARTESIAN_POINT('Ctrl Pts',(-0.152774050896218,-0.0293854314049922,
1.72757403013639));
#19356=CARTESIAN_POINT('Ctrl Pts',(-0.152040759071231,-0.0328640208606756,
1.72782302989824));
#19357=CARTESIAN_POINT('Ctrl Pts',(-0.151870572343261,-0.0336417226174832,
1.72787897336641));
#19358=CARTESIAN_POINT('Ctrl Pts',(-0.151576166862013,-0.0349392872115377,
1.72797279031911));
#19359=CARTESIAN_POINT('Ctrl Pts',(-0.151455223537571,-0.0354598844018647,
1.72801055968426));
#19360=CARTESIAN_POINT('Ctrl Pts',(-0.15121211856038,-0.0364823865362186,
1.72808500171594));
#19361=CARTESIAN_POINT('Ctrl Pts',(-0.151090134917705,-0.0369843270281836,
1.72812166827056));
#19362=CARTESIAN_POINT('Ctrl Pts',(-0.150854357508204,-0.0379338716032327,
1.72819127050672));
#19363=CARTESIAN_POINT('Ctrl Pts',(-0.150741065737695,-0.0383815956655832,
1.72822418970341));
#19364=CARTESIAN_POINT('Ctrl Pts',(-0.150479751482428,-0.039395293231898,
1.72829895450225));
#19365=CARTESIAN_POINT('Ctrl Pts',(-0.150330527356654,-0.0399609467156958,
1.72834083847357));
#19366=CARTESIAN_POINT('Ctrl Pts',(-0.149879573722586,-0.0416320666385901,
1.72846507262903));
#19367=CARTESIAN_POINT('Ctrl Pts',(-0.149568821301318,-0.0427350342895152,
1.72854771328153));
#19368=CARTESIAN_POINT('Ctrl Pts',(-0.146529633706473,-0.0530827502500465,
1.72932926656177));
#19369=CARTESIAN_POINT('Ctrl Pts',(-0.142960188045411,-0.0620566522011234,
1.73005616359697));
#19370=CARTESIAN_POINT('Ctrl Pts',(-0.136058948306859,-0.0755955641029131,
1.73122726110572));
#19371=CARTESIAN_POINT('Ctrl Pts',(-0.133269673865166,-0.0804109353330466,
1.73165974624265));
#19372=CARTESIAN_POINT('Ctrl Pts',(-0.12649044660889,-0.0907892833558381,
1.7326190552481));
#19373=CARTESIAN_POINT('Ctrl Pts',(-0.122378613694646,-0.0962601935947096,
1.73314386905609));
#19374=CARTESIAN_POINT('Ctrl Pts',(-0.117198038191796,-0.102282191626779,
1.73373054988717));
#19375=CARTESIAN_POINT('Ctrl Pts',(-0.116467454786522,-0.103113331067661,
1.7338117278688));
#19376=CARTESIAN_POINT('Ctrl Pts',(-0.115521071871376,-0.104167079217518,
1.73391483679874));
#19377=CARTESIAN_POINT('Ctrl Pts',(-0.115313416915625,-0.104396907630037,
1.73393733708179));
#19378=CARTESIAN_POINT('Ctrl Pts',(-0.114906883315595,-0.104844158103298,
1.73398114321194));
#19379=CARTESIAN_POINT('Ctrl Pts',(-0.114708070779714,-0.10506163821127,
1.73400245375995));
#19380=CARTESIAN_POINT('Ctrl Pts',(-0.114333665793,-0.105468868399165,1.73404237307569));
#19381=CARTESIAN_POINT('Ctrl Pts',(-0.114158220408911,-0.105658743365668,
1.73406099190778));
#19382=CARTESIAN_POINT('Ctrl Pts',(-0.113754632556436,-0.106093345727504,
1.73410362365506));
#19383=CARTESIAN_POINT('Ctrl Pts',(-0.113526173529466,-0.106337774874026,
1.73412761206854));
#19384=CARTESIAN_POINT('Ctrl Pts',(-0.112814515616789,-0.107094272738072,
1.73420189818956));
#19385=CARTESIAN_POINT('Ctrl Pts',(-0.112328618271171,-0.107603809201015,
1.73425199486069));
#19386=CARTESIAN_POINT('Ctrl Pts',(-0.106707450824626,-0.113418877160757,
1.73482468526606));
#19387=CARTESIAN_POINT('Ctrl Pts',(-0.101203284594116,-0.118356460023565,
1.73532043183209));
#19388=CARTESIAN_POINT('Ctrl Pts',(-0.0897364859266798,-0.127255592215326,
1.73628197636209));
#19389=CARTESIAN_POINT('Ctrl Pts',(-0.0838109111111542,-0.131233970511423,
1.73674719417848));
#19390=CARTESIAN_POINT('Ctrl Pts',(-0.0728495457315214,-0.137547163850056,
1.73758641401376));
#19391=CARTESIAN_POINT('Ctrl Pts',(-0.0679228654962218,-0.140045543363424,
1.73795661394668));
#19392=CARTESIAN_POINT('Ctrl Pts',(-0.0600219163241034,-0.143537089284572,
1.73854903602219));
#19393=CARTESIAN_POINT('Ctrl Pts',(-0.0571326140867982,-0.144711397329763,
1.73876538497644));
#19394=CARTESIAN_POINT('Ctrl Pts',(-0.0534350880930995,-0.146086199251163,
1.73904281585321));
#19395=CARTESIAN_POINT('Ctrl Pts',(-0.0526577645394653,-0.146368186562579,
1.73910116911291));
#19396=CARTESIAN_POINT('Ctrl Pts',(-0.0513875174733978,-0.146817561952489,
1.73919659117301));
#19397=CARTESIAN_POINT('Ctrl Pts',(-0.0508959292532899,-0.146988699644592,
1.73923353551572));
#19398=CARTESIAN_POINT('Ctrl Pts',(-0.0499671905651373,-0.147306805894034,
1.73930336730971));
#19399=CARTESIAN_POINT('Ctrl Pts',(-0.049530226343338,-0.147454304330661,
1.73933623685491));
#19400=CARTESIAN_POINT('Ctrl Pts',(-0.0485436195289985,-0.147782455805455,
1.73941048738589));
#19401=CARTESIAN_POINT('Ctrl Pts',(-0.047993614597459,-0.147961988976933,
1.73945190467083));
#19402=CARTESIAN_POINT('Ctrl Pts',(-0.046583665922037,-0.148413537317381,
1.73955814890924));
#19403=CARTESIAN_POINT('Ctrl Pts',(-0.0457223450234555,-0.148681145716725,
1.73962311889532));
#19404=CARTESIAN_POINT('Ctrl Pts',(-0.0405150468451091,-0.150249502106093,
1.74001636252311));
#19405=CARTESIAN_POINT('Ctrl Pts',(-0.0361166406666132,-0.151366978928621,
1.74035051644414));
#19406=CARTESIAN_POINT('Ctrl Pts',(-0.0193356853182221,-0.154857378831999,
1.74163433119736));
#19407=CARTESIAN_POINT('Ctrl Pts',(-0.00673007942645939,-0.155914386861695,
1.74262168519795));
#19408=CARTESIAN_POINT('Ctrl Pts',(0.00987534283940077,-0.155288149733739,
1.74390068800435));
#19409=CARTESIAN_POINT('Ctrl Pts',(0.0138815922782705,-0.154981413030162,
1.74420708414451));
#19410=CARTESIAN_POINT('Ctrl Pts',(0.0198985994718691,-0.154285486156554,
1.74466015548634));
#19411=CARTESIAN_POINT('Ctrl Pts',(0.0219207576787233,-0.15401119106018,
1.74481119196353));
#19412=CARTESIAN_POINT('Ctrl Pts',(0.0244339350925388,-0.153619784494405,
1.74499690292667));
#19413=CARTESIAN_POINT('Ctrl Pts',(0.024930440361999,-0.153539990016912,
1.7450334942952));
#19414=CARTESIAN_POINT('Ctrl Pts',(0.025722947577856,-0.153408678782246,
1.74509173475559));
#19415=CARTESIAN_POINT('Ctrl Pts',(0.0260191965912659,-0.153358710775517,
1.74511346872854));
#19416=CARTESIAN_POINT('Ctrl Pts',(0.0265693236146171,-0.153264281457372,
1.74515375703412));
#19417=CARTESIAN_POINT('Ctrl Pts',(0.0268232333488723,-0.153220047913235,
1.74517232353617));
#19418=CARTESIAN_POINT('Ctrl Pts',(0.0273980642454144,-0.153118434075364,
1.74521429309068));
#19419=CARTESIAN_POINT('Ctrl Pts',(0.0277189150736658,-0.153060675976906,
1.74523767446213));
#19420=CARTESIAN_POINT('Ctrl Pts',(0.0286893488580272,-0.15288283138867,
1.74530826448711));
#19421=CARTESIAN_POINT('Ctrl Pts',(0.0293383621485162,-0.15275961318156,
1.74535529983243));
#19422=CARTESIAN_POINT('Ctrl Pts',(0.0343440365276796,-0.151776183564272,
1.7457168637528));
#19423=CARTESIAN_POINT('Ctrl Pts',(0.0386633523977352,-0.15073379573123,
1.74602179117571));
#19424=CARTESIAN_POINT('Ctrl Pts',(0.0571643788942634,-0.14542104904157,
1.74732057551452));
#19425=CARTESIAN_POINT('Ctrl Pts',(0.0707397721978309,-0.139323294616565,
1.74826204308894));
#19426=CARTESIAN_POINT('Ctrl Pts',(0.0865285793673756,-0.129320069239485,
1.74953569024452));
#19427=CARTESIAN_POINT('Ctrl Pts',(0.0897289405352208,-0.127120369063847,
1.74980387603136));
#19428=CARTESIAN_POINT('Ctrl Pts',(0.093573142699395,-0.12426059935753,
1.75014052866187));
#19429=CARTESIAN_POINT('Ctrl Pts',(0.0942980334991059,-0.123711399647648,
1.75020467089541));
#19430=CARTESIAN_POINT('Ctrl Pts',(0.0954353443859444,-0.122833933937407,
1.75030637902431));
#19431=CARTESIAN_POINT('Ctrl Pts',(0.0958509918576321,-0.122509867488594,
1.75034377942158));
#19432=CARTESIAN_POINT('Ctrl Pts',(0.0966266145223844,-0.121898776966581,
1.75041400731021));
#19433=CARTESIAN_POINT('Ctrl Pts',(0.0969869789748826,-0.121612254156248,
1.75044681461652));
#19434=CARTESIAN_POINT('Ctrl Pts',(0.0977898748815137,-0.120968039772314,
1.75052031358092));
#19435=CARTESIAN_POINT('Ctrl Pts',(0.0982317243458602,-0.120609512857936,
1.75056103846722));
#19436=CARTESIAN_POINT('Ctrl Pts',(0.0993448760503353,-0.119696101194275,
1.75066434725146));
#19437=CARTESIAN_POINT('Ctrl Pts',(0.100013495837147,-0.119137994072607,
1.75072706103009));
#19438=CARTESIAN_POINT('Ctrl Pts',(0.103770331522889,-0.115948193752939,
1.75108324752233));
#19439=CARTESIAN_POINT('Ctrl Pts',(0.106759054856323,-0.113202313939023,
1.75138139144821));
#19440=CARTESIAN_POINT('Ctrl Pts',(0.11096342196824,-0.109024854418954,
1.75182363894561));
#19441=CARTESIAN_POINT('Ctrl Pts',(0.112266115707445,-0.107682954389712,
1.75196410517105));
#19442=CARTESIAN_POINT('Ctrl Pts',(0.123607070491539,-0.0955711673085891,
1.75321784346555));
#19443=CARTESIAN_POINT('Ctrl Pts',(0.132091779129171,-0.0834520237155355,
1.75438540631624));
#19444=CARTESIAN_POINT('Ctrl Pts',(0.139913288702606,-0.0680201106625926,
1.75568674219346));
#19445=CARTESIAN_POINT('Ctrl Pts',(0.141022722549392,-0.0656890984411436,
1.75587855666601));
#19446=CARTESIAN_POINT('Ctrl Pts',(0.142292944183374,-0.0628395614316616,
1.75610645962497));
#19447=CARTESIAN_POINT('Ctrl Pts',(0.142509626835847,-0.0623466015711575,
1.7561456516211));
#19448=CARTESIAN_POINT('Ctrl Pts',(0.142843198153651,-0.0615768907859745,
1.75620647087489));
#19449=CARTESIAN_POINT('Ctrl Pts',(0.142961849499286,-0.0613009162211243,
1.75622820238575));
#19450=CARTESIAN_POINT('Ctrl Pts',(0.143180817146159,-0.0607875195341439,
1.75626848846425));
#19451=CARTESIAN_POINT('Ctrl Pts',(0.143281341825506,-0.0605501941885859,
1.75628705518921));
#19452=CARTESIAN_POINT('Ctrl Pts',(0.143507700127799,-0.0600120722183201,
1.75632902822296));
#19453=CARTESIAN_POINT('Ctrl Pts',(0.143633177929451,-0.0597111297085974,
1.75635241283563));
#19454=CARTESIAN_POINT('Ctrl Pts',(0.144010096591986,-0.0587990752681772,
1.7564230223198));
#19455=CARTESIAN_POINT('Ctrl Pts',(0.144258594841011,-0.0581867427253662,
1.75647007374252));
#19456=CARTESIAN_POINT('Ctrl Pts',(0.146149408554309,-0.0534409518917513,
1.75683214812904));
#19457=CARTESIAN_POINT('Ctrl Pts',(0.147617849606137,-0.0492398692978504,
1.75713753929933));
#19458=CARTESIAN_POINT('Ctrl Pts',(0.153189754390315,-0.0307947914952604,
1.75843756626187));
#19459=CARTESIAN_POINT('Ctrl Pts',(0.155426056734633,-0.016068878104595,
1.75937981562853));
#19460=CARTESIAN_POINT('Ctrl Pts',(0.155576005672513,0.00261647402569874,
1.76065330553863));
#19461=CARTESIAN_POINT('Ctrl Pts',(0.155462972470131,0.00648069197999925,
1.76092030639963));
#19462=CARTESIAN_POINT('Ctrl Pts',(0.155145838445867,0.0112426018721626,
1.76125564449856));
#19463=CARTESIAN_POINT('Ctrl Pts',(0.155077555704418,0.0121482071999812,
1.7613196982774));
#19464=CARTESIAN_POINT('Ctrl Pts',(0.154957143229427,0.0135780614487544,
1.76142129783928));
#19465=CARTESIAN_POINT('Ctrl Pts',(0.154910272775595,0.0141027432332509,
1.76145867872746));
#19466=CARTESIAN_POINT('Ctrl Pts',(0.154817443031725,0.0150855500045843,
1.7615288892302));
#19467=CARTESIAN_POINT('Ctrl Pts',(0.154772112917346,0.0155437299433997,
1.76156169875603));
#19468=CARTESIAN_POINT('Ctrl Pts',(0.154666174746554,0.0165680748340622,
1.7616352277448));
#19469=CARTESIAN_POINT('Ctrl Pts',(0.154604491052928,0.0171341193168057,
1.76167598055993));
#19470=CARTESIAN_POINT('Ctrl Pts',(0.15444045686002,0.0185663268778815,
1.76177940736583));
#19471=CARTESIAN_POINT('Ctrl Pts',(0.154333927727908,0.0194319814569409,
1.76184221175509));
#19472=CARTESIAN_POINT('Ctrl Pts',(0.153688554556271,0.0243357164885009,
1.76219968263018));
#19473=CARTESIAN_POINT('Ctrl Pts',(0.152998566227657,0.0283519293732846,
1.76249905939415));
#19474=CARTESIAN_POINT('Ctrl Pts',(0.151766141399666,0.0341508855888993,
1.76294148558436));
#19475=CARTESIAN_POINT('Ctrl Pts',(0.151348032537155,0.035958548735151,
1.76308084876283));
#19476=CARTESIAN_POINT('Ctrl Pts',(0.147321336088201,0.052050910791138,
1.76433431280582));
#19477=CARTESIAN_POINT('Ctrl Pts',(0.141733246908828,0.0657607987281602,
1.76550278924448));
#19478=CARTESIAN_POINT('Ctrl Pts',(0.133005762830483,0.0806961110609668,
1.76680375777164));
#19479=CARTESIAN_POINT('Ctrl Pts',(0.13165551943514,0.0828807672353076,
1.76699456339878));
#19480=CARTESIAN_POINT('Ctrl Pts',(0.129957796177516,0.0854813592326551,
1.76722142954024));
#19481=CARTESIAN_POINT('Ctrl Pts',(0.129661554647012,0.0859300461600298,
1.76726056132213));
#19482=CARTESIAN_POINT('Ctrl Pts',(0.129196275788744,0.0866268720001769,
1.76732130764618));
#19483=CARTESIAN_POINT('Ctrl Pts',(0.129028840368,0.0868760668289772,1.76734302604481));
#19484=CARTESIAN_POINT('Ctrl Pts',(0.128716310194509,0.0873383102035789,
1.76738330027735));
#19485=CARTESIAN_POINT('Ctrl Pts',(0.128571408823881,0.0875514807080559,
1.76740186820422));
#19486=CARTESIAN_POINT('Ctrl Pts',(0.128241873787442,0.0880336911344328,
1.76744385983441));
#19487=CARTESIAN_POINT('Ctrl Pts',(0.128056923399997,0.0883025103940371,
1.76746726176095));
#19488=CARTESIAN_POINT('Ctrl Pts',(0.12749416283232,0.0891149775839778,
1.76753797524011));
#19489=CARTESIAN_POINT('Ctrl Pts',(0.127113719881456,0.0896568070248737,
1.76758511259187));
#19490=CARTESIAN_POINT('Ctrl Pts',(0.124128822420835,0.0938507254158757,
1.76794994727309));
#19491=CARTESIAN_POINT('Ctrl Pts',(0.121370647486039,0.0973914711342306,
1.76825784620435));
#19492=CARTESIAN_POINT('Ctrl Pts',(0.108812642963751,0.112148753435143,
1.76956480867118));
#19493=CARTESIAN_POINT('Ctrl Pts',(0.0975841401833062,0.122044732983213,
1.77051148329402));
#19494=CARTESIAN_POINT('Ctrl Pts',(0.0819661568475446,0.132255605476125,
1.77178419864028));
#19495=CARTESIAN_POINT('Ctrl Pts',(0.0787392383769247,0.134201804712946,
1.77204461483336));
#19496=CARTESIAN_POINT('Ctrl Pts',(0.0746571354149566,0.136465843557174,
1.77237264348729));
#19497=CARTESIAN_POINT('Ctrl Pts',(0.0738654296511796,0.136895991787701,
1.77243619732048));
#19498=CARTESIAN_POINT('Ctrl Pts',(0.0726064048948479,0.137565941636466,
1.77253718319987));
#19499=CARTESIAN_POINT('Ctrl Pts',(0.0721415222795669,0.13781030106984,
1.77257445374281));
#19500=CARTESIAN_POINT('Ctrl Pts',(0.0712666397819486,0.138264531587501,
1.77264456661951));
#19501=CARTESIAN_POINT('Ctrl Pts',(0.0708569268086231,0.138474945588649,
1.77267738941107));
#19502=CARTESIAN_POINT('Ctrl Pts',(0.0699366546778662,0.138942411008693,
1.77275109163477));
#19503=CARTESIAN_POINT('Ctrl Pts',(0.0694256032566575,0.139198472839179,
1.77279200513208));
#19504=CARTESIAN_POINT('Ctrl Pts',(0.0681248077724416,0.139841289810439,
1.77289611155742));
#19505=CARTESIAN_POINT('Ctrl Pts',(0.0673331832232085,0.140224171054325,
1.77295943788348));
#19506=CARTESIAN_POINT('Ctrl Pts',(0.0627576298089193,0.14238952801178,
1.77332533835482));
#19507=CARTESIAN_POINT('Ctrl Pts',(0.0589066301748565,0.144025346776159,
1.77363288645451));
#19508=CARTESIAN_POINT('Ctrl Pts',(0.0533485686906487,0.14612607454763,
1.77407669683773));
#19509=CARTESIAN_POINT('Ctrl Pts',(0.0516920282657672,0.14672025507256,
1.77420895249216));
#19510=CARTESIAN_POINT('Ctrl Pts',(0.036000900263383,0.152049753605084,
1.77546134552491));
#19511=CARTESIAN_POINT('Ctrl Pts',(0.0213697357688163,0.154785173011199,
1.77663647192841));
#19512=CARTESIAN_POINT('Ctrl Pts',(0.00410313479575672,0.155515535062561,
1.77793493690867));
#19513=CARTESIAN_POINT('Ctrl Pts',(0.00163018392792171,0.155561118990352,
1.77811856032015));
#19514=CARTESIAN_POINT('Ctrl Pts',(-0.00137463617365801,0.155544834492541,
1.77833802929362));
#19515=CARTESIAN_POINT('Ctrl Pts',(-0.00190628019363298,0.155539227463588,
1.7783767211403));
#19516=CARTESIAN_POINT('Ctrl Pts',(-0.00273676651825873,0.155526209864854,
1.77843693442425));
#19517=CARTESIAN_POINT('Ctrl Pts',(-0.00303562697926189,0.155520663639465,
1.77845855683875));
#19518=CARTESIAN_POINT('Ctrl Pts',(-0.00359231848293808,0.155508727288098,
1.77849874513097));
#19519=CARTESIAN_POINT('Ctrl Pts',(-0.00385014687188625,0.155502557489095,
1.77851732262894));
#19520=CARTESIAN_POINT('Ctrl Pts',(-0.00443597061740971,0.155487080902078,
1.77855945390996));
#19521=CARTESIAN_POINT('Ctrl Pts',(-0.00476395208235854,0.155477377546403,
1.7785829853135));
#19522=CARTESIAN_POINT('Ctrl Pts',(-0.00561421528973363,0.155449529391081,
1.77864384800574));
#19523=CARTESIAN_POINT('Ctrl Pts',(-0.00613644649395696,0.155429790086746,
1.77868109245691));
#19524=CARTESIAN_POINT('Ctrl Pts',(-0.00941449492455507,0.155289338994041,
1.77891406980479));
#19525=CARTESIAN_POINT('Ctrl Pts',(-0.0121670130950097,0.155097962027391,
1.77910611946731));
#19526=CARTESIAN_POINT('Ctrl Pts',(-0.0163642092862801,0.15469369767609,
1.77939550118484));
#19527=CARTESIAN_POINT('Ctrl Pts',(-0.0178132250117427,0.154533545665462,
1.77949477075443));
#19528=CARTESIAN_POINT('Ctrl Pts',(-0.0210375272090124,0.154131224583442,
1.77971466890965));
#19529=CARTESIAN_POINT('Ctrl Pts',(-0.0228113228616239,0.153878705077222,
1.77983496857021));
#19530=CARTESIAN_POINT('Ctrl Pts',(-0.0342514347887873,0.15204790607571,
1.78060870008363));
#19531=CARTESIAN_POINT('Ctrl Pts',(-0.0437547698812458,0.149590296956172,
1.7812429162474));
#19532=CARTESIAN_POINT('Ctrl Pts',(-0.0565926488913294,0.144941255437753,
1.78215317429878));
#19533=CARTESIAN_POINT('Ctrl Pts',(-0.0601699153776717,0.143493061934122,
1.78241277129182));
#19534=CARTESIAN_POINT('Ctrl Pts',(-0.0636886300450479,0.141913920751225,
1.78267615293977));
#19535=CARTESIAN_POINT('Origin',(0.,0.,-0.129405622560373));
#19536=CARTESIAN_POINT('',(-0.0636886258329835,0.14191392264153,1.86645936880636));
#19537=CARTESIAN_POINT('',(-0.0636886270478348,0.141913922096325,1.85272361624831));
#19538=CARTESIAN_POINT('',(-0.0636886258329924,0.141913922641526,-0.129405622560373));
#19539=CARTESIAN_POINT('',(-0.155549955676549,-0.000117426673429394,1.80932156858097));
#19540=CARTESIAN_POINT('Ctrl Pts',(-0.0636886258329876,0.141913922641528,
1.86645936880636));
#19541=CARTESIAN_POINT('Ctrl Pts',(-0.0636564620419431,0.141928357220004,
1.86645680851686));
#19542=CARTESIAN_POINT('Ctrl Pts',(-0.0636242932870201,0.141942780889352,
1.86645424886815));
#19543=CARTESIAN_POINT('Ctrl Pts',(-0.0632942811561062,0.142090615390378,
1.86642800064363));
#19544=CARTESIAN_POINT('Ctrl Pts',(-0.0629960198527353,0.142223101137319,
1.86640436670713));
#19545=CARTESIAN_POINT('Ctrl Pts',(-0.0624613755478455,0.142458574836849,
1.8663621637997));
#19546=CARTESIAN_POINT('Ctrl Pts',(-0.0622251524764948,0.142561914208194,
1.86634357370127));
#19547=CARTESIAN_POINT('Ctrl Pts',(-0.0617131975510311,0.142784361743086,
1.86630340681509));
#19548=CARTESIAN_POINT('Ctrl Pts',(-0.0614373780922462,0.142903258492115,
1.86628184296741));
#19549=CARTESIAN_POINT('Ctrl Pts',(-0.0606665579334369,0.143232889651892,
1.86622178756415));
#19550=CARTESIAN_POINT('Ctrl Pts',(-0.0601707992166112,0.143441858862749,
1.86618340138882));
#19551=CARTESIAN_POINT('Ctrl Pts',(-0.0572994636863012,0.144634661035102,
1.86596239739613));
#19552=CARTESIAN_POINT('Ctrl Pts',(-0.0549006897583775,0.14556211750769,
1.86578297484937));
#19553=CARTESIAN_POINT('Ctrl Pts',(-0.0386103521660974,0.151400509948218,
1.86459203355857));
#19554=CARTESIAN_POINT('Ctrl Pts',(-0.0241036913399888,0.154376150486204,
1.86365816026321));
#19555=CARTESIAN_POINT('Ctrl Pts',(-0.00751453163996468,0.155379785751169,
1.86254161332361));
#19556=CARTESIAN_POINT('Ctrl Pts',(-0.00563369337086947,0.155459342306031,
1.8624144493627));
#19557=CARTESIAN_POINT('Ctrl Pts',(0.000290051260673029,0.15560226687935,
1.86201143129366));
#19558=CARTESIAN_POINT('Ctrl Pts',(0.00433395751572635,0.155542153580607,
1.86173257915957));
#19559=CARTESIAN_POINT('Ctrl Pts',(0.00923954774031282,0.155277784727314,
1.86138769066159));
#19560=CARTESIAN_POINT('Ctrl Pts',(0.0101080190607186,0.155223669484268,
1.86132638251121));
#19561=CARTESIAN_POINT('Ctrl Pts',(0.0115434237840658,0.155122130840707,
1.861224617874));
#19562=CARTESIAN_POINT('Ctrl Pts',(0.0121106410099563,0.155078878213475,
1.86118429194483));
#19563=CARTESIAN_POINT('Ctrl Pts',(0.0131365864351479,0.154994982734194,
1.86111114375714));
#19564=CARTESIAN_POINT('Ctrl Pts',(0.0135953979016833,0.154955412049647,
1.8610783554427));
#19565=CARTESIAN_POINT('Ctrl Pts',(0.0145793310951522,0.154866148093182,
1.86100787398236));
#19566=CARTESIAN_POINT('Ctrl Pts',(0.0151043879339209,0.154815820163473,
1.8609701613248));
#19567=CARTESIAN_POINT('Ctrl Pts',(0.0165354040004468,0.154671304854158,
1.86086709441261));
#19568=CARTESIAN_POINT('Ctrl Pts',(0.0174407956175257,0.154571830271281,
1.86080157515396));
#19569=CARTESIAN_POINT('Ctrl Pts',(0.022217170088745,0.154004555563906,
1.86045424302941));
#19570=CARTESIAN_POINT('Ctrl Pts',(0.0260700845105509,0.153399320174467,
1.86016815238346));
#19571=CARTESIAN_POINT('Ctrl Pts',(0.0444232491006836,0.149804927033222,
1.85877529464241));
#19572=CARTESIAN_POINT('Ctrl Pts',(0.0584690221189989,0.144900545957311,
1.85760838445969));
#19573=CARTESIAN_POINT('Ctrl Pts',(0.0755370563172391,0.13604985293001,
1.85613928008289));
#19574=CARTESIAN_POINT('Ctrl Pts',(0.0793795865855532,0.133844311176416,
1.85580562828475));
#19575=CARTESIAN_POINT('Ctrl Pts',(0.0836812765253949,0.131124682910041,
1.85543284471027));
#19576=CARTESIAN_POINT('Ctrl Pts',(0.0842371598384742,0.130768266232467,
1.85538468766181));
#19577=CARTESIAN_POINT('Ctrl Pts',(0.0850640872380474,0.130230602568646,
1.85531309257506));
#19578=CARTESIAN_POINT('Ctrl Pts',(0.085336848668374,0.130052032078268,
1.85528948402377));
#19579=CARTESIAN_POINT('Ctrl Pts',(0.0858243027934332,0.129730713466181,
1.85524730845479));
#19580=CARTESIAN_POINT('Ctrl Pts',(0.0860392028736441,0.129588288586679,
1.85522872042675));
#19581=CARTESIAN_POINT('Ctrl Pts',(0.0865039097251108,0.12927863885955,
1.85518853751938));
#19582=CARTESIAN_POINT('Ctrl Pts',(0.0867535854775034,0.129111224431017,
1.85516695567075));
#19583=CARTESIAN_POINT('Ctrl Pts',(0.0874497063912889,0.128641525318255,
1.85510679941594));
#19584=CARTESIAN_POINT('Ctrl Pts',(0.0878950735235377,0.128337637727252,
1.85506833096416));
#19585=CARTESIAN_POINT('Ctrl Pts',(0.0904708221408475,0.126560428105555,
1.85484590231258));
#19586=CARTESIAN_POINT('Ctrl Pts',(0.092565878869125,0.125036281979947,
1.85466518576827));
#19587=CARTESIAN_POINT('Ctrl Pts',(0.106303783438006,0.114507329475116,
1.8534742650543));
#19588=CARTESIAN_POINT('Ctrl Pts',(0.116656893927821,0.103940854068111,
1.85254128531495));
#19589=CARTESIAN_POINT('Ctrl Pts',(0.126498330036356,0.090540603257222,
1.85142426928196));
#19590=CARTESIAN_POINT('Ctrl Pts',(0.127597159841334,0.088985351218547,
1.85129562347155));
#19591=CARTESIAN_POINT('Ctrl Pts',(0.130925501772152,0.0840860669673104,
1.85089270111927));
#19592=CARTESIAN_POINT('Ctrl Pts',(0.133054005605272,0.0806757738536333,
1.85061548661836));
#19593=CARTESIAN_POINT('Ctrl Pts',(0.135478920018413,0.0764331017066894,
1.85027241012731));
#19594=CARTESIAN_POINT('Ctrl Pts',(0.135903560914175,0.0756754840238233,
1.85021121687891));
#19595=CARTESIAN_POINT('Ctrl Pts',(0.136595553117784,0.0744162643307243,
1.85010960357116));
#19596=CARTESIAN_POINT('Ctrl Pts',(0.136866543398813,0.0739166747831478,
1.85006931338459));
#19597=CARTESIAN_POINT('Ctrl Pts',(0.137352121588842,0.0730096516749289,
1.84999620338284));
#19598=CARTESIAN_POINT('Ctrl Pts',(0.137567650845395,0.0726027270505144,
1.84996341734699));
#19599=CARTESIAN_POINT('Ctrl Pts',(0.138026352217636,0.0717273114519083,
1.84989291119219));
#19600=CARTESIAN_POINT('Ctrl Pts',(0.138268952240869,0.0712585289502712,
1.84985517143316));
#19601=CARTESIAN_POINT('Ctrl Pts',(0.138924441542764,0.0699759584983784,
1.84975195488272));
#19602=CARTESIAN_POINT('Ctrl Pts',(0.139332557373286,0.0691597687649968,
1.84968631227857));
#19603=CARTESIAN_POINT('Ctrl Pts',(0.141456960674764,0.0648160461813629,
1.84933713336321));
#19604=CARTESIAN_POINT('Ctrl Pts',(0.143046377612563,0.0612284270731534,
1.8490492649099));
#19605=CARTESIAN_POINT('Ctrl Pts',(0.149972392480942,0.0438488933048152,
1.84765561813267));
#19606=CARTESIAN_POINT('Ctrl Pts',(0.153459237289211,0.0294034203451148,
1.84648999322492));
#19607=CARTESIAN_POINT('Ctrl Pts',(0.155272196199702,0.010289272616759,
1.84502299951898));
#19608=CARTESIAN_POINT('Ctrl Pts',(0.15550184761795,0.00587438691557986,
1.84469009565279));
#19609=CARTESIAN_POINT('Ctrl Pts',(0.155549367139988,0.000795280883174198,
1.84431804453059));
#19610=CARTESIAN_POINT('Ctrl Pts',(0.155551341470964,0.000135269279772496,
1.84426991090671));
#19611=CARTESIAN_POINT('Ctrl Pts',(0.155548015282042,-0.000850695760490853,
1.8441983437245));
#19612=CARTESIAN_POINT('Ctrl Pts',(0.155545891181125,-0.00117664073826175,
1.84417473984506));
#19613=CARTESIAN_POINT('Ctrl Pts',(0.155540252168953,-0.00176037473149842,
1.84413256930341));
#19614=CARTESIAN_POINT('Ctrl Pts',(0.155537120928838,-0.00201816269779856,
1.84411398165239));
#19615=CARTESIAN_POINT('Ctrl Pts',(0.155528949690423,-0.0025765673966196,
1.84407379577822));
#19616=CARTESIAN_POINT('Ctrl Pts',(0.155523679061816,-0.00287717684641305,
1.8440522106025));
#19617=CARTESIAN_POINT('Ctrl Pts',(0.155506517963022,-0.0037170266902462,
1.84399203570189));
#19618=CARTESIAN_POINT('Ctrl Pts',(0.155492694173688,-0.00425623049467691,
1.8439535520377));
#19619=CARTESIAN_POINT('Ctrl Pts',(0.155396105290372,-0.00738785208885911,
1.84373085868057));
#19620=CARTESIAN_POINT('Ctrl Pts',(0.155251308132826,-0.009978143621746,
1.84354990167561));
#19621=CARTESIAN_POINT('Ctrl Pts',(0.153853230496537,-0.0272309194385228,
1.84235898381934));
#19622=CARTESIAN_POINT('Ctrl Pts',(0.150589433582856,-0.0416565841488789,
1.84142616942558));
#19623=CARTESIAN_POINT('Ctrl Pts',(0.144666507281365,-0.0571930563456218,
1.84030906042476));
#19624=CARTESIAN_POINT('Ctrl Pts',(0.143954006901864,-0.0589634421328646,
1.84018013424006));
#19625=CARTESIAN_POINT('Ctrl Pts',(0.141642135899606,-0.0644160085607246,
1.83977722932767));
#19626=CARTESIAN_POINT('Ctrl Pts',(0.139932787840494,-0.0680494448601561,
1.83950032401785));
#19627=CARTESIAN_POINT('Ctrl Pts',(0.137685262712994,-0.0723831796436164,
1.83915758965993));
#19628=CARTESIAN_POINT('Ctrl Pts',(0.137279122640218,-0.0731505208210331,
1.83909641817064));
#19629=CARTESIAN_POINT('Ctrl Pts',(0.136596561435496,-0.0744144127340373,
1.83899483352174));
#19630=CARTESIAN_POINT('Ctrl Pts',(0.136323800816748,-0.0749129276819405,
1.83895455010541));
#19631=CARTESIAN_POINT('Ctrl Pts',(0.135825082211533,-0.0758126742612604,
1.8388814473313));
#19632=CARTESIAN_POINT('Ctrl Pts',(0.135600061426161,-0.0762144203499371,
1.83884866172163));
#19633=CARTESIAN_POINT('Ctrl Pts',(0.135113243312695,-0.0770745916055004,
1.83877815086338));
#19634=CARTESIAN_POINT('Ctrl Pts',(0.13485089013256,-0.077532693796875,
1.83874040595029));
#19635=CARTESIAN_POINT('Ctrl Pts',(0.134128524073201,-0.0787792792874892,
1.83863716093697));
#19636=CARTESIAN_POINT('Ctrl Pts',(0.133663900431018,-0.079565051817242,
1.83857149486996));
#19637=CARTESIAN_POINT('Ctrl Pts',(0.131163751583623,-0.0837096019302213,
1.8382219632588));
#19638=CARTESIAN_POINT('Ctrl Pts',(0.129008657715937,-0.0869941852401678,
1.83793375514853));
#19639=CARTESIAN_POINT('Ctrl Pts',(0.118159868929774,-0.102237932551405,
1.83653995653891));
#19640=CARTESIAN_POINT('Ctrl Pts',(0.107915092313449,-0.112997952342107,
1.83537457593628));
#19641=CARTESIAN_POINT('Ctrl Pts',(0.0928419949743466,-0.124882631437129,
1.83390798523657));
#19642=CARTESIAN_POINT('Ctrl Pts',(0.0892585910117333,-0.127468508177072,
1.83357522512988));
#19643=CARTESIAN_POINT('Ctrl Pts',(0.0850184828871368,-0.130261642765548,
1.83320331481461));
#19644=CARTESIAN_POINT('Ctrl Pts',(0.0844650618765273,-0.130621175053868,
1.83315518570705));
#19645=CARTESIAN_POINT('Ctrl Pts',(0.0836349106926757,-0.131153003956719,
1.83308362390508));
#19646=CARTESIAN_POINT('Ctrl Pts',(0.083359909733341,-0.13132796422693,
1.83306002092652));
#19647=CARTESIAN_POINT('Ctrl Pts',(0.0828664088163777,-0.131639763192521,
1.83301785135415));
#19648=CARTESIAN_POINT('Ctrl Pts',(0.082648117757366,-0.131776923617908,
1.8329992637757));
#19649=CARTESIAN_POINT('Ctrl Pts',(0.0821796301652738,-0.132069669821476,
1.83295951200915));
#19650=CARTESIAN_POINT('Ctrl Pts',(0.0819293331163704,-0.132225087180495,
1.83293835891954));
#19651=CARTESIAN_POINT('Ctrl Pts',(0.0812366087046629,-0.132652499503837,
1.83288004523023));
#19652=CARTESIAN_POINT('Ctrl Pts',(0.0807932528251867,-0.132922994763733,
1.83284298142844));
#19653=CARTESIAN_POINT('Ctrl Pts',(0.0797964936795299,-0.133524296518719,
1.83276021080323));
#19654=CARTESIAN_POINT('Ctrl Pts',(0.0792423678983951,-0.133853895464776,
1.83271457795244));
#19655=CARTESIAN_POINT('Ctrl Pts',(0.0775137429805142,-0.13486759998589,
1.83257335318037));
#19656=CARTESIAN_POINT('Ctrl Pts',(0.0763322792542339,-0.135539785033318,
1.83247843898825));
#19657=CARTESIAN_POINT('Ctrl Pts',(0.0716828811839098,-0.138104944678126,
1.83211054704997));
#19658=CARTESIAN_POINT('Ctrl Pts',(0.068151902602447,-0.139881144391765,
1.8318432060018));
#19659=CARTESIAN_POINT('Ctrl Pts',(0.0517969745066226,-0.147341675565304,
1.83064156364857));
#19660=CARTESIAN_POINT('Ctrl Pts',(0.0383091525225917,-0.151409762360861,
1.82974390620955));
#19661=CARTESIAN_POINT('Ctrl Pts',(0.0234906498389948,-0.15376915258353,
1.8287176225249));
#19662=CARTESIAN_POINT('Ctrl Pts',(0.0225214150315662,-0.153914095240971,
1.82865035313605));
#19663=CARTESIAN_POINT('Ctrl Pts',(0.0192895791703714,-0.154366214720551,
1.82842548450659));
#19664=CARTESIAN_POINT('Ctrl Pts',(0.0170216819466096,-0.154632718166361,
1.82826676225427));
#19665=CARTESIAN_POINT('Ctrl Pts',(0.0138781364727169,-0.15493212974269,
1.82804509243061));
#19666=CARTESIAN_POINT('Ctrl Pts',(0.0130067672610395,-0.15500771415759,
1.82798347167475));
#19667=CARTESIAN_POINT('Ctrl Pts',(0.0115663056362418,-0.155120431486351,
1.82788129539222));
#19668=CARTESIAN_POINT('Ctrl Pts',(0.010997555341956,-0.155161791209602,
1.8278408722943));
#19669=CARTESIAN_POINT('Ctrl Pts',(0.00996901504006827,-0.155230903523213,
1.82776762005582));
#19670=CARTESIAN_POINT('Ctrl Pts',(0.00950930247782793,-0.155259743100141,
1.82773482530713));
#19671=CARTESIAN_POINT('Ctrl Pts',(0.00852390171567526,-0.15531716828125,
1.82766440983169));
#19672=CARTESIAN_POINT('Ctrl Pts',(0.00799818427422717,-0.155345127696682,
1.82762676993899));
#19673=CARTESIAN_POINT('Ctrl Pts',(0.00656710084386395,-0.155413953818681,
1.82752410456597));
#19674=CARTESIAN_POINT('Ctrl Pts',(0.00566151576986955,-0.155449577129231,
1.82745891624326));
#19675=CARTESIAN_POINT('Ctrl Pts',(0.00112065133212638,-0.155588471614936,
1.827130884288));
#19676=CARTESIAN_POINT('Ctrl Pts',(-0.00251685938817576,-0.155572136556827,
1.82686434952662));
#19677=CARTESIAN_POINT('Ctrl Pts',(-0.0211178836382268,-0.15483610736433,
1.82548066633444));
#19678=CARTESIAN_POINT('Ctrl Pts',(-0.0359203693870522,-0.152084692956403,
1.82430027079617));
#19679=CARTESIAN_POINT('Ctrl Pts',(-0.0543748581382912,-0.145806716336831,
1.8228099120028));
#19680=CARTESIAN_POINT('Ctrl Pts',(-0.0585881334893525,-0.144165404552133,
1.82246919741571));
#19681=CARTESIAN_POINT('Ctrl Pts',(-0.0633313089393348,-0.142075288787899,
1.82208950700556));
#19682=CARTESIAN_POINT('Ctrl Pts',(-0.0639365256379832,-0.141803960127855,
1.82204113472764));
#19683=CARTESIAN_POINT('Ctrl Pts',(-0.0648371595087773,-0.141393252709448,
1.82196928330904));
#19684=CARTESIAN_POINT('Ctrl Pts',(-0.0651338924031497,-0.141256805962291,
1.82194563188759));
#19685=CARTESIAN_POINT('Ctrl Pts',(-0.0656641306598325,-0.141010960332821,
1.82190341012858));
#19686=CARTESIAN_POINT('Ctrl Pts',(-0.065897794752191,-0.140901914960937,
1.82188481858288));
#19687=CARTESIAN_POINT('Ctrl Pts',(-0.0663974298853807,-0.140667232593432,
1.82184509669582));
#19688=CARTESIAN_POINT('Ctrl Pts',(-0.0666633151911642,-0.140541422479324,
1.821823977286));
#19689=CARTESIAN_POINT('Ctrl Pts',(-0.0673932488709636,-0.140193499054368,
1.82176604602531));
#19690=CARTESIAN_POINT('Ctrl Pts',(-0.0678565604684636,-0.139969833863938,
1.82172932846458));
#19691=CARTESIAN_POINT('Ctrl Pts',(-0.0688929303610933,-0.139463167570136,
1.82164729626669));
#19692=CARTESIAN_POINT('Ctrl Pts',(-0.0694653753341122,-0.139178923074163,
1.82160205454881));
#19693=CARTESIAN_POINT('Ctrl Pts',(-0.0712349755614895,-0.138286599596392,
1.82146236315737));
#19694=CARTESIAN_POINT('Ctrl Pts',(-0.0724260578789047,-0.137666523916598,
1.82136857435658));
#19695=CARTESIAN_POINT('Ctrl Pts',(-0.0770261396153564,-0.135195497144179,
1.82100668035147));
#19696=CARTESIAN_POINT('Ctrl Pts',(-0.0803737028351996,-0.133232584158757,
1.82074401750884));
#19697=CARTESIAN_POINT('Ctrl Pts',(-0.0889778440617732,-0.12774489896864,
1.82006139434388));
#19698=CARTESIAN_POINT('Ctrl Pts',(-0.0940988123137882,-0.124021110263872,
1.81964717418066));
#19699=CARTESIAN_POINT('Ctrl Pts',(-0.107274675415437,-0.11315294392232,
1.81852213990994));
#19700=CARTESIAN_POINT('Ctrl Pts',(-0.11483708847046,-0.105469592136939,
1.81780778981687));
#19701=CARTESIAN_POINT('Ctrl Pts',(-0.12225534010549,-0.0961806920995499,
1.81697539317036));
#19702=CARTESIAN_POINT('Ctrl Pts',(-0.122954673636267,-0.0952850556319218,
1.81689545334115));
#19703=CARTESIAN_POINT('Ctrl Pts',(-0.123997902005043,-0.0939183835674643,
1.81677390713177));
#19704=CARTESIAN_POINT('Ctrl Pts',(-0.124349075167464,-0.0934529291236586,
1.81673258680023));
#19705=CARTESIAN_POINT('Ctrl Pts',(-0.124973655052058,-0.0926153403581597,
1.81665835866833));
#19706=CARTESIAN_POINT('Ctrl Pts',(-0.125248038816172,-0.0922439401316245,
1.8166254893906));
#19707=CARTESIAN_POINT('Ctrl Pts',(-0.125826704208121,-0.0914533287066598,
1.81655561062264));
#19708=CARTESIAN_POINT('Ctrl Pts',(-0.126130552970582,-0.0910338092071362,
1.81651858494027));
#19709=CARTESIAN_POINT('Ctrl Pts',(-0.126937929762812,-0.0899072738824901,
1.81641929804675));
#19710=CARTESIAN_POINT('Ctrl Pts',(-0.127437638408971,-0.0891975569703274,
1.81635689169476));
#19711=CARTESIAN_POINT('Ctrl Pts',(-0.129837449838406,-0.0857278654928895,
1.81605245436584));
#19712=CARTESIAN_POINT('Ctrl Pts',(-0.131653834759047,-0.0829113675733186,
1.81580730510471));
#19713=CARTESIAN_POINT('Ctrl Pts',(-0.139956286019524,-0.0690760177112689,
1.81461117564694));
#19714=CARTESIAN_POINT('Ctrl Pts',(-0.145157214274883,-0.0573456832257681,
1.81361539428185));
#19715=CARTESIAN_POINT('Ctrl Pts',(-0.149542666292154,-0.0428750426454134,
1.81244648344936));
#19716=CARTESIAN_POINT('Ctrl Pts',(-0.150170754217539,-0.0406204816221885,
1.81226617356169));
#19717=CARTESIAN_POINT('Ctrl Pts',(-0.151009461864669,-0.0373238742499031,
1.81200578953618));
#19718=CARTESIAN_POINT('Ctrl Pts',(-0.1512606415017,-0.0362925279388187,
1.81192478832263));
#19719=CARTESIAN_POINT('Ctrl Pts',(-0.152341911866877,-0.0316464705246524,
1.81156215943024));
#19720=CARTESIAN_POINT('Ctrl Pts',(-0.153053207698486,-0.0280049726370916,
1.81128406451051));
#19721=CARTESIAN_POINT('Ctrl Pts',(-0.153722844379017,-0.0237784405222317,
1.81097080115317));
#19722=CARTESIAN_POINT('Ctrl Pts',(-0.15380891120363,-0.0232152100761871,
1.81092924927667));
#19723=CARTESIAN_POINT('Ctrl Pts',(-0.15394119655569,-0.0223164777682235,
1.81086326808289));
#19724=CARTESIAN_POINT('Ctrl Pts',(-0.153989416428217,-0.0219812831971472,
1.81083873078794));
#19725=CARTESIAN_POINT('Ctrl Pts',(-0.154072695950437,-0.0213886503143945,
1.8107954772736));
#19726=CARTESIAN_POINT('Ctrl Pts',(-0.154108205726354,-0.0211312785174762,
1.81077673597431));
#19727=CARTESIAN_POINT('Ctrl Pts',(-0.154175500040681,-0.0206343423719801,
1.81074063407907));
#19728=CARTESIAN_POINT('Ctrl Pts',(-0.15420737101874,-0.0203947940315143,
1.81072326854061));
#19729=CARTESIAN_POINT('Ctrl Pts',(-0.154275728181463,-0.0198716866236958,
1.81068542668589));
#19730=CARTESIAN_POINT('Ctrl Pts',(-0.154311991230341,-0.0195880984587095,
1.8106649628452));
#19731=CARTESIAN_POINT('Ctrl Pts',(-0.15439900183165,-0.0188924093816475,
1.81061488322392));
#19732=CARTESIAN_POINT('Ctrl Pts',(-0.154448882006616,-0.0184801990277524,
1.81058531454102));
#19733=CARTESIAN_POINT('Ctrl Pts',(-0.15468090489266,-0.0164961782766216,
1.81044347774166));
#19734=CARTESIAN_POINT('Ctrl Pts',(-0.154840716091074,-0.0149217755762949,
1.81033237560722));
#19735=CARTESIAN_POINT('Ctrl Pts',(-0.155355261515561,-0.00894637900416368,
1.80991525300518));
#19736=CARTESIAN_POINT('Ctrl Pts',(-0.15554662219701,-0.004533140577823,
1.80961648263341));
#19737=CARTESIAN_POINT('Ctrl Pts',(-0.155549955676549,-0.000117426673429394,
1.80932156858097));
#19738=CARTESIAN_POINT('Ctrl Pts',(-0.155549955521704,-0.000117631611270232,
1.80932158226823));
#19739=CARTESIAN_POINT('Ctrl Pts',(-0.155560738863627,0.0141417017295138,
1.80836923805862));
#19740=CARTESIAN_POINT('Ctrl Pts',(-0.153610934688343,0.0283350059680006,
1.80745647397623));
#19741=CARTESIAN_POINT('Ctrl Pts',(-0.149198092134331,0.0440449895399718,
1.80633725968971));
#19742=CARTESIAN_POINT('Ctrl Pts',(-0.148602762839775,0.0460135851926938,
1.80619512336027));
#19743=CARTESIAN_POINT('Ctrl Pts',(-0.14750525529041,0.0493989841121755,
1.80594701719294));
#19744=CARTESIAN_POINT('Ctrl Pts',(-0.147021237269486,0.0508214077378316,
1.80584163231634));
#19745=CARTESIAN_POINT('Ctrl Pts',(-0.146300409230229,0.052843236139914,
1.8056901021855));
#19746=CARTESIAN_POINT('Ctrl Pts',(-0.146080350264335,0.0534485602310435,
1.80564451057016));
#19747=CARTESIAN_POINT('Ctrl Pts',(-0.145692988874763,0.0544938254972557,
1.80556538623048));
#19748=CARTESIAN_POINT('Ctrl Pts',(-0.145527435991347,0.0549344098854867,
1.8055319120577));
#19749=CARTESIAN_POINT('Ctrl Pts',(-0.145205745548454,0.0557788619924441,
1.80546751375657));
#19750=CARTESIAN_POINT('Ctrl Pts',(-0.145049915975545,0.0561828430569072,
1.80543660018784));
#19751=CARTESIAN_POINT('Ctrl Pts',(-0.14463836210943,0.0572366523974596,
1.80535568023318));
#19752=CARTESIAN_POINT('Ctrl Pts',(-0.144379947365159,0.0578854121581196,
1.80530558397854));
#19753=CARTESIAN_POINT('Ctrl Pts',(-0.143473777047417,0.0601165646048386,
1.80513231648243));
#19754=CARTESIAN_POINT('Ctrl Pts',(-0.142804325916678,0.0616899514174252,
1.80500841767145));
#19755=CARTESIAN_POINT('Ctrl Pts',(-0.13704350715295,0.0746328736371978,
1.80397451163622));
#19756=CARTESIAN_POINT('Ctrl Pts',(-0.130630140419206,0.0853617221118853,
1.80301710881141));
#19757=CARTESIAN_POINT('Ctrl Pts',(-0.11974069723175,0.0994307349326424,
1.80163736795009));
#19758=CARTESIAN_POINT('Ctrl Pts',(-0.116257570484368,0.103481825035288,
1.80122351873294));
#19759=CARTESIAN_POINT('Ctrl Pts',(-0.110651771172711,0.109360584763755,
1.80060435374106));
#19760=CARTESIAN_POINT('Ctrl Pts',(-0.108676792236485,0.1113234428085,1.80039416712177));
#19761=CARTESIAN_POINT('Ctrl Pts',(-0.105484411770058,0.114330247428091,
1.8000680034392));
#19762=CARTESIAN_POINT('Ctrl Pts',(-0.104301814567342,0.115410132263105,
1.79994996008178));
#19763=CARTESIAN_POINT('Ctrl Pts',(-0.102757966688457,0.116776773101693,
1.79979962313376));
#19764=CARTESIAN_POINT('Ctrl Pts',(-0.10241188418018,0.117080401635869,
1.79976616070373));
#19765=CARTESIAN_POINT('Ctrl Pts',(-0.101880673211268,0.117542291265832,
1.79971516827065));
#19766=CARTESIAN_POINT('Ctrl Pts',(-0.101696516859723,0.117701657893309,
1.79969755801851));
#19767=CARTESIAN_POINT('Ctrl Pts',(-0.101316590455687,0.118028884174733,
1.79966136685421));
#19768=CARTESIAN_POINT('Ctrl Pts',(-0.101120779604156,0.118196687496519,
1.7996427905456));
#19769=CARTESIAN_POINT('Ctrl Pts',(-0.100675826185169,0.118576082580841,
1.79960075005223));
#19770=CARTESIAN_POINT('Ctrl Pts',(-0.100426433879831,0.118787376104477,
1.79957730781075));
#19771=CARTESIAN_POINT('Ctrl Pts',(-0.0997798874355749,0.119331660390181,
1.79951684062115));
#19772=CARTESIAN_POINT('Ctrl Pts',(-0.0993817274198907,0.119663458847844,
1.79947990061539));
#19773=CARTESIAN_POINT('Ctrl Pts',(-0.0969100736687121,0.121702314961719,
1.79925236440348));
#19774=CARTESIAN_POINT('Ctrl Pts',(-0.0947941533135505,0.123357556214743,
1.79906525705705));
#19775=CARTESIAN_POINT('Ctrl Pts',(-0.0836215375643028,0.131640300423681,
1.79810995077965));
#19776=CARTESIAN_POINT('Ctrl Pts',(-0.0739152376547061,0.13732438993798,
1.79738602440817));
#19777=CARTESIAN_POINT('Ctrl Pts',(-0.0636886042805433,0.141913932313908,
1.79664456958818));
#19778=CARTESIAN_POINT('Ctrl Pts',(-0.0636886300450479,0.141913920751225,
1.78267615293977));
#19779=CARTESIAN_POINT('Ctrl Pts',(-0.0660993195437263,0.14083204301279,
1.7828565970601));
#19780=CARTESIAN_POINT('Ctrl Pts',(-0.0684825273057478,0.139688702071741,
1.78303880607663));
#19781=CARTESIAN_POINT('Ctrl Pts',(-0.0721719261371492,0.137801551123463,
1.78332771456659));
#19782=CARTESIAN_POINT('Ctrl Pts',(-0.0734979305663783,0.137098899853142,
1.78343297136628));
#19783=CARTESIAN_POINT('Ctrl Pts',(-0.0753778312888652,0.136067627770644,
1.78358434088179));
#19784=CARTESIAN_POINT('Ctrl Pts',(-0.075940205827141,0.135754564908042,
1.78362990145506));
#19785=CARTESIAN_POINT('Ctrl Pts',(-0.0769102537213168,0.135206644490763,
1.7837089809439));
#19786=CARTESIAN_POINT('Ctrl Pts',(-0.0773188377909223,0.134973409068957,
1.78374244142472));
#19787=CARTESIAN_POINT('Ctrl Pts',(-0.0781013399649563,0.134522007880192,
1.78380681971748));
#19788=CARTESIAN_POINT('Ctrl Pts',(-0.0784754183176416,0.134304127342873,
1.78383772700189));
#19789=CARTESIAN_POINT('Ctrl Pts',(-0.0794505923334774,0.133730675704304,
1.78391864458196));
#19790=CARTESIAN_POINT('Ctrl Pts',(-0.0800502055771495,0.133372616394951,
1.78396874479226));
#19791=CARTESIAN_POINT('Ctrl Pts',(-0.0821104010587525,0.132123472014965,
1.78414209602427));
#19792=CARTESIAN_POINT('Ctrl Pts',(-0.0835586318831108,0.131212363832694,
1.78426607572063));
#19793=CARTESIAN_POINT('Ctrl Pts',(-0.0853677588334433,0.130032111762796,
1.78442371875312));
#19794=CARTESIAN_POINT('Ctrl Pts',(-0.0857429610185856,0.129785010558621,
1.78445656564615));
#19795=CARTESIAN_POINT('Ctrl Pts',(-0.0873986339145944,0.128684301854563,
1.78460219098865));
#19796=CARTESIAN_POINT('Ctrl Pts',(-0.0886674266789305,0.1278133713383,
1.78471559824639));
#19797=CARTESIAN_POINT('Ctrl Pts',(-0.0901471572161616,0.126765010868033,
1.78485003112098));
#19798=CARTESIAN_POINT('Ctrl Pts',(-0.090370843407186,0.126605642033457,
1.78487041218998));
#19799=CARTESIAN_POINT('Ctrl Pts',(-0.0906681003255401,0.126392667387216,
1.78489757573141));
#19800=CARTESIAN_POINT('Ctrl Pts',(-0.0907420488753485,0.126339587429039,
1.78490433973949));
#19801=CARTESIAN_POINT('Ctrl Pts',(-0.102437483933876,0.117929088007935,
1.78597514634011));
#19802=CARTESIAN_POINT('Ctrl Pts',(-0.112848559638326,0.10800818693888,
1.78709972280912));
#19803=CARTESIAN_POINT('Ctrl Pts',(-0.123971048553361,0.0940195166007185,
1.7884711231809));
#19804=CARTESIAN_POINT('Ctrl Pts',(-0.126091641044852,0.0911558683767185,
1.78874191736275));
#19805=CARTESIAN_POINT('Ctrl Pts',(-0.129194697338093,0.0866497298841924,
1.78915038510548));
#19806=CARTESIAN_POINT('Ctrl Pts',(-0.130248259928525,0.0850578461985455,
1.78929146074993));
#19807=CARTESIAN_POINT('Ctrl Pts',(-0.131534996704143,0.0830336492029423,
1.78946646280861));
#19808=CARTESIAN_POINT('Ctrl Pts',(-0.131795728586652,0.0826191757504856,
1.78950206909926));
#19809=CARTESIAN_POINT('Ctrl Pts',(-0.132207560964326,0.0819575939476739,
1.78955853505648));
#19810=CARTESIAN_POINT('Ctrl Pts',(-0.132359932985498,0.0817112876269627,
1.78957947646506));
#19811=CARTESIAN_POINT('Ctrl Pts',(-0.132647573136666,0.0812434073068773,
1.7896191013932));
#19812=CARTESIAN_POINT('Ctrl Pts',(-0.132782972792836,0.081021923128343,
1.78963779308804));
#19813=CARTESIAN_POINT('Ctrl Pts',(-0.133093183275362,0.0805116205024207,
1.78968070943139));
#19814=CARTESIAN_POINT('Ctrl Pts',(-0.133267608817349,0.0802225711146323,
1.78970490880335));
#19815=CARTESIAN_POINT('Ctrl Pts',(-0.133732131629205,0.0794470907854553,
1.78976954596523));
#19816=CARTESIAN_POINT('Ctrl Pts',(-0.134020519326323,0.0789596332954653,
1.7898098755891));
#19817=CARTESIAN_POINT('Ctrl Pts',(-0.136135832341254,0.0753391723804295,
1.79010728011749));
#19818=CARTESIAN_POINT('Ctrl Pts',(-0.137855533453968,0.0721443898547238,
1.79035794716405));
#19819=CARTESIAN_POINT('Ctrl Pts',(-0.140324060946091,0.0671472110759991,
1.79073686992327));
#19820=CARTESIAN_POINT('Ctrl Pts',(-0.141153210864882,0.0653862495728781,
1.79086797575452));
#19821=CARTESIAN_POINT('Ctrl Pts',(-0.146464826947219,0.0535331182565205,
1.79173739516868));
#19822=CARTESIAN_POINT('Ctrl Pts',(-0.149894712614579,0.0430038453052157,
1.79244953890622));
#19823=CARTESIAN_POINT('Ctrl Pts',(-0.15337120981272,0.0265734408528152,
1.79357441874203));
#19824=CARTESIAN_POINT('Ctrl Pts',(-0.154248625780776,0.0208859992640989,
1.79396571069371));
#19825=CARTESIAN_POINT('Ctrl Pts',(-0.154946063020434,0.0137656402587616,
1.79446506825141));
#19826=CARTESIAN_POINT('Ctrl Pts',(-0.155064040519323,0.012366018279522,
1.79456366349082));
#19827=CARTESIAN_POINT('Ctrl Pts',(-0.155207222483695,0.0103398906956653,
1.7947071078982));
#19828=CARTESIAN_POINT('Ctrl Pts',(-0.155247620745165,0.00971449859113958,
1.79475148224923));
#19829=CARTESIAN_POINT('Ctrl Pts',(-0.15531155967217,0.00862209785140042,
1.79482917205834));
#19830=CARTESIAN_POINT('Ctrl Pts',(-0.155336775987848,0.00815519197361416,
1.79486243474348));
#19831=CARTESIAN_POINT('Ctrl Pts',(-0.155381489267641,0.00725164310437124,
1.79492691776882));
#19832=CARTESIAN_POINT('Ctrl Pts',(-0.155401251826188,0.00681501712472446,
1.79495812948408));
#19833=CARTESIAN_POINT('Ctrl Pts',(-0.155443880419716,0.00577629483704786,
1.7950325063112));
#19834=CARTESIAN_POINT('Ctrl Pts',(-0.155465088631871,0.0051741414487422,
1.7950757228151));
#19835=CARTESIAN_POINT('Ctrl Pts',(-0.1555281175846,0.00303062474474945,
1.79522992849819));
#19836=CARTESIAN_POINT('Ctrl Pts',(-0.155550516320546,0.00148882645850541,
1.79534152011039));
#19837=CARTESIAN_POINT('Ctrl Pts',(-0.155547567385575,-0.00716617543588156,
1.7959719428411));
#19838=CARTESIAN_POINT('Ctrl Pts',(-0.155057239775376,-0.0142696878047434,
1.7965050829819));
#19839=CARTESIAN_POINT('Ctrl Pts',(-0.152542314054278,-0.0324507130486709,
1.79790842307936));
#19840=CARTESIAN_POINT('Ctrl Pts',(-0.149799043234581,-0.0433870598182914,
1.79879230599892));
#19841=CARTESIAN_POINT('Ctrl Pts',(-0.144597648413662,-0.0574583069646395,
1.7999331806907));
#19842=CARTESIAN_POINT('Ctrl Pts',(-0.143166574684856,-0.0609366453009342,
1.80021518730951));
#19843=CARTESIAN_POINT('Ctrl Pts',(-0.141351425281628,-0.0649304991732725,
1.80053635122305));
#19844=CARTESIAN_POINT('Ctrl Pts',(-0.141088705842597,-0.0654994066505062,
1.80058203520829));
#19845=CARTESIAN_POINT('Ctrl Pts',(-0.140685242475547,-0.0663593969260929,
1.80065097868876));
#19846=CARTESIAN_POINT('Ctrl Pts',(-0.140547021498559,-0.0666516448698306,
1.80067438732942));
#19847=CARTESIAN_POINT('Ctrl Pts',(-0.140297049425733,-0.0671759387921151,
1.80071634337122));
#19848=CARTESIAN_POINT('Ctrl Pts',(-0.140185632876428,-0.0674081387414485,
1.80073491088125));
#19849=CARTESIAN_POINT('Ctrl Pts',(-0.139942102350116,-0.067912458271536,
1.80077520724378));
#19850=CARTESIAN_POINT('Ctrl Pts',(-0.13980977154196,-0.0681844687908162,
1.80079692237223));
#19851=CARTESIAN_POINT('Ctrl Pts',(-0.139435443380284,-0.0689482415791615,
1.80085784673591));
#19852=CARTESIAN_POINT('Ctrl Pts',(-0.13919163593693,-0.0694391200753304,
1.80089694555382));
#19853=CARTESIAN_POINT('Ctrl Pts',(-0.137711901960155,-0.0723792856437115,
1.80113084839836));
#19854=CARTESIAN_POINT('Ctrl Pts',(-0.136413851222573,-0.074797009417925,
1.80132200456924));
#19855=CARTESIAN_POINT('Ctrl Pts',(-0.127812274866051,-0.0898484976299198,
1.80251263430261));
#19856=CARTESIAN_POINT('Ctrl Pts',(-0.118824899933258,-0.101437051090246,
1.8034382554979));
#19857=CARTESIAN_POINT('Ctrl Pts',(-0.106863679347039,-0.113049832999375,
1.80455860297636));
#19858=CARTESIAN_POINT('Ctrl Pts',(-0.105345721639859,-0.114465667781599,
1.80469894264839));
#19859=CARTESIAN_POINT('Ctrl Pts',(-0.100946634805867,-0.118407163799,1.80510136841206));
#19860=CARTESIAN_POINT('Ctrl Pts',(-0.0980000889938683,-0.120857179759862,
1.80536591627675));
#19861=CARTESIAN_POINT('Ctrl Pts',(-0.094223240516612,-0.123768589372263,
1.80570078304102));
#19862=CARTESIAN_POINT('Ctrl Pts',(-0.0934750117855153,-0.124334648716937,
1.8057669226331));
#19863=CARTESIAN_POINT('Ctrl Pts',(-0.0922889535057659,-0.125215183091308,
1.80587147538308));
#19864=CARTESIAN_POINT('Ctrl Pts',(-0.0918545225953824,-0.125534217173092,
1.80590971093589));
#19865=CARTESIAN_POINT('Ctrl Pts',(-0.0910837666838125,-0.12609409606157,
1.80597744626916));
#19866=CARTESIAN_POINT('Ctrl Pts',(-0.0907481206592936,-0.126335870621284,
1.80600690981264));
#19867=CARTESIAN_POINT('Ctrl Pts',(-0.0899758631602345,-0.126887482348012,
1.80607462551528));
#19868=CARTESIAN_POINT('Ctrl Pts',(-0.0895386105955854,-0.127196408469037,
1.806112912097));
#19869=CARTESIAN_POINT('Ctrl Pts',(-0.0883231888106177,-0.1280457512492,
1.80621919341197));
#19870=CARTESIAN_POINT('Ctrl Pts',(-0.0875416752411319,-0.128581317137559,
1.80628737098144));
#19871=CARTESIAN_POINT('Ctrl Pts',(-0.0830573240377973,-0.131594579400806,
1.80667772327069));
#19872=CARTESIAN_POINT('Ctrl Pts',(-0.0792546492225045,-0.133919175292075,
1.80700553961995));
#19873=CARTESIAN_POINT('Ctrl Pts',(-0.0667617630725284,-0.140837575497677,
1.80807385880212));
#19874=CARTESIAN_POINT('Ctrl Pts',(-0.0577350301942027,-0.144772140236993,
1.80883464127416));
#19875=CARTESIAN_POINT('Ctrl Pts',(-0.0454155540406945,-0.148805527999693,
1.80983969709433));
#19876=CARTESIAN_POINT('Ctrl Pts',(-0.0424031260308537,-0.149691795115015,
1.81008277682033));
#19877=CARTESIAN_POINT('Ctrl Pts',(-0.0339685556882593,-0.151898203642045,
1.8107532468151));
#19878=CARTESIAN_POINT('Ctrl Pts',(-0.0284984445059328,-0.153018893773931,
1.81117672278218));
#19879=CARTESIAN_POINT('Ctrl Pts',(-0.0222966298226149,-0.153945247472467,
1.81163632006117));
#19880=CARTESIAN_POINT('Ctrl Pts',(-0.0216132823917812,-0.154042672635799,
1.81168668193879));
#19881=CARTESIAN_POINT('Ctrl Pts',(-0.0206004328109134,-0.154180202394673,
1.81176089314641));
#19882=CARTESIAN_POINT('Ctrl Pts',(-0.0202714272233383,-0.154223804538641,
1.81178493151334));
#19883=CARTESIAN_POINT('Ctrl Pts',(-0.0196861668887895,-0.154299462162193,
1.81182756935953));
#19884=CARTESIAN_POINT('Ctrl Pts',(-0.019429970062829,-0.15433193272133,
1.81184619184856));
#19885=CARTESIAN_POINT('Ctrl Pts',(-0.0188795836738217,-0.154400296799664,
1.81188610735996));
#19886=CARTESIAN_POINT('Ctrl Pts',(-0.0185853727809231,-0.154435987561571,
1.81190738885477));
#19887=CARTESIAN_POINT('Ctrl Pts',(-0.017774589932738,-0.154531993232262,
1.81196588787537));
#19888=CARTESIAN_POINT('Ctrl Pts',(-0.0172578081988455,-0.154590559402815,
1.81200300866115));
#19889=CARTESIAN_POINT('Ctrl Pts',(-0.0144534021128516,-0.154894140810337,
1.81220360099765));
#19890=CARTESIAN_POINT('Ctrl Pts',(-0.0121606943537004,-0.155090988527376,
1.81236452802214));
#19891=CARTESIAN_POINT('Ctrl Pts',(0.00442615334605453,-0.156144975493712,
1.81351220119229));
#19892=CARTESIAN_POINT('Ctrl Pts',(0.0187751646110651,-0.155075624351142,
1.81442184189406));
#19893=CARTESIAN_POINT('Ctrl Pts',(0.0356907355888509,-0.151429388518624,
1.8155796519892));
#19894=CARTESIAN_POINT('Ctrl Pts',(0.0385859211185941,-0.15071766147605,
1.81578069014362));
#19895=CARTESIAN_POINT('Ctrl Pts',(0.0450329377410033,-0.148934847196117,
1.81623688953109));
#19896=CARTESIAN_POINT('Ctrl Pts',(0.0485703607026916,-0.147819046283623,
1.81649314541671));
#19897=CARTESIAN_POINT('Ctrl Pts',(0.0529387295115218,-0.146267407488952,
1.81681872475852));
#19898=CARTESIAN_POINT('Ctrl Pts',(0.0538103341798763,-0.145949002890421,
1.81688414689994));
#19899=CARTESIAN_POINT('Ctrl Pts',(0.0551814079429259,-0.145434186813767,
1.81698781209391));
#19900=CARTESIAN_POINT('Ctrl Pts',(0.0556828093102768,-0.145242952362378,
1.81702588253904));
#19901=CARTESIAN_POINT('Ctrl Pts',(0.0566077790248279,-0.144884675386082,
1.81709641511479));
#19902=CARTESIAN_POINT('Ctrl Pts',(0.0570316243283967,-0.144718359672256,
1.81712885259955));
#19903=CARTESIAN_POINT('Ctrl Pts',(0.0579704130695654,-0.144345216931998,
1.81720096412459));
#19904=CARTESIAN_POINT('Ctrl Pts',(0.0584849901120479,-0.144137491165365,
1.81724066804496));
#19905=CARTESIAN_POINT('Ctrl Pts',(0.0599591696251532,-0.143533196780265,
1.81735493107821));
#19906=CARTESIAN_POINT('Ctrl Pts',(0.0609159111996078,-0.143129774210828,
1.8174297206714));
#19907=CARTESIAN_POINT('Ctrl Pts',(0.0677178553124872,-0.140181094127348,
1.81796607029896));
#19908=CARTESIAN_POINT('Ctrl Pts',(0.0734049020781071,-0.137288550936618,
1.81843946477828));
#19909=CARTESIAN_POINT('Ctrl Pts',(0.0889259439808886,-0.128153719506339,
1.81980497193102));
#19910=CARTESIAN_POINT('Ctrl Pts',(0.0982598328355665,-0.12114520778316,
1.82071862790115));
#19911=CARTESIAN_POINT('Ctrl Pts',(0.107372640040885,-0.112550941083126,
1.82167832073806));
#19912=CARTESIAN_POINT('Ctrl Pts',(0.108016307700081,-0.111933352892162,
1.82174649227641));
#19913=CARTESIAN_POINT('Ctrl Pts',(0.109290533549153,-0.110689527238917,
1.82188216856525));
#19914=CARTESIAN_POINT('Ctrl Pts',(0.109921111213798,-0.110063352362464,
1.82194967260876));
#19915=CARTESIAN_POINT('Ctrl Pts',(0.112790446884848,-0.107164794065537,
1.82225838512181));
#19916=CARTESIAN_POINT('Ctrl Pts',(0.114964542771656,-0.10482907839211,
1.82249668855405));
#19917=CARTESIAN_POINT('Ctrl Pts',(0.117424940355258,-0.102017076636863,
1.82277005737856));
#19918=CARTESIAN_POINT('Ctrl Pts',(0.117782272923036,-0.101604314631881,
1.8228098547045));
#19919=CARTESIAN_POINT('Ctrl Pts',(0.118353141528868,-0.100937834051706,
1.82287357603107));
#19920=CARTESIAN_POINT('Ctrl Pts',(0.118568047962958,-0.100685304094595,
1.82289759698814));
#19921=CARTESIAN_POINT('Ctrl Pts',(0.118949252924753,-0.100234448734355,
1.82294026134793));
#19922=CARTESIAN_POINT('Ctrl Pts',(0.119115865551268,-0.100036393689773,
1.82295892753767));
#19923=CARTESIAN_POINT('Ctrl Pts',(0.11947009688091,-0.0996131735623726,
1.82299865307639));
#19924=CARTESIAN_POINT('Ctrl Pts',(0.119657573375082,-0.0993878943018883,
1.82301970211499));
#19925=CARTESIAN_POINT('Ctrl Pts',(0.120166483775259,-0.0987728399755167,
1.8230769112006));
#19926=CARTESIAN_POINT('Ctrl Pts',(0.120486661144623,-0.0983820219601504,
1.82311298145283));
#19927=CARTESIAN_POINT('Ctrl Pts',(0.122127374922265,-0.0963592947283289,
1.82329826361165));
#19928=CARTESIAN_POINT('Ctrl Pts',(0.12341676408973,-0.0947022328146605,
1.82344536802031));
#19929=CARTESIAN_POINT('Ctrl Pts',(0.127126826336368,-0.0897297040578735,
1.82387489839765));
#19930=CARTESIAN_POINT('Ctrl Pts',(0.129450397223665,-0.0863437902506564,
1.82415223531415));
#19931=CARTESIAN_POINT('Ctrl Pts',(0.137192624616017,-0.0740453521775083,
1.8251223837964));
#19932=CARTESIAN_POINT('Ctrl Pts',(0.141846434226912,-0.064684847224075,
1.82579642226397));
#19933=CARTESIAN_POINT('Ctrl Pts',(0.146581187528148,-0.0521405823635516,
1.82669353215479));
#19934=CARTESIAN_POINT('Ctrl Pts',(0.147553220218096,-0.049322718362778,
1.82689452583116));
#19935=CARTESIAN_POINT('Ctrl Pts',(0.149552901486416,-0.0429361484432803,
1.82735093735407));
#19936=CARTESIAN_POINT('Ctrl Pts',(0.150534869711399,-0.0393552076327877,
1.82760745739826));
#19937=CARTESIAN_POINT('Ctrl Pts',(0.151601063376423,-0.034839371066159,
1.82793333279798));
#19938=CARTESIAN_POINT('Ctrl Pts',(0.151806269759443,-0.033934062359601,
1.82799877814057));
#19939=CARTESIAN_POINT('Ctrl Pts',(0.152117313596115,-0.0325025147192592,
1.82810247204166));
#19940=CARTESIAN_POINT('Ctrl Pts',(0.152228553651633,-0.031977460793193,
1.82814054783209));
#19941=CARTESIAN_POINT('Ctrl Pts',(0.152429134973468,-0.0310059448483054,
1.82821108547675));
#19942=CARTESIAN_POINT('Ctrl Pts',(0.152519237897706,-0.0305596444303453,
1.82824352265947));
#19943=CARTESIAN_POINT('Ctrl Pts',(0.152714790353047,-0.0295686176922568,
1.82831562752342));
#19944=CARTESIAN_POINT('Ctrl Pts',(0.152819286971521,-0.0290237120227464,
1.82835532505633));
#19945=CARTESIAN_POINT('Ctrl Pts',(0.153110884644325,-0.0274579085000242,
1.8284695516337));
#19946=CARTESIAN_POINT('Ctrl Pts',(0.153290682892403,-0.0264356989142027,
1.82854431092911));
#19947=CARTESIAN_POINT('Ctrl Pts',(0.154499878070304,-0.0191334435096642,
1.82907979760083));
#19948=CARTESIAN_POINT('Ctrl Pts',(0.155153109478316,-0.0127981444706719,
1.82955231542756));
#19949=CARTESIAN_POINT('Ctrl Pts',(0.15589327309689,0.0050602976572865,
1.8309074224547));
#19950=CARTESIAN_POINT('Ctrl Pts',(0.155091624561486,0.0165790394049576,
1.83181089860493));
#19951=CARTESIAN_POINT('Ctrl Pts',(0.152818973036498,0.0290432345926528,
1.83278231029944));
#19952=CARTESIAN_POINT('Ctrl Pts',(0.152598141460801,0.0301820365419172,
1.83287096904561));
#19953=CARTESIAN_POINT('Ctrl Pts',(0.151581035387582,0.0351302943827947,
1.83325553092566));
#19954=CARTESIAN_POINT('Ctrl Pts',(0.150654612573212,0.0389119779843826,
1.8335477137593));
#19955=CARTESIAN_POINT('Ctrl Pts',(0.149413908964097,0.0432629820613394,
1.83387897875532));
#19956=CARTESIAN_POINT('Ctrl Pts',(0.149236919992898,0.0438696199729306,
1.83392505225227));
#19957=CARTESIAN_POINT('Ctrl Pts',(0.148963475759938,0.0447860540657251,
1.83399446576866));
#19958=CARTESIAN_POINT('Ctrl Pts',(0.148869743022015,0.0450966447426477,
1.83401795793707));
#19959=CARTESIAN_POINT('Ctrl Pts',(0.148699835394235,0.0456533440427679,
1.83406000313021));
#19960=CARTESIAN_POINT('Ctrl Pts',(0.148624020592433,0.045899557459171,
1.83407857665016));
#19961=CARTESIAN_POINT('Ctrl Pts',(0.148458116425995,0.0464336207548007,
1.83411881663422));
#19962=CARTESIAN_POINT('Ctrl Pts',(0.148367801696054,0.0467213965250036,
1.83414046968378));
#19963=CARTESIAN_POINT('Ctrl Pts',(0.148112233844685,0.0475275148505829,
1.83420104506756));
#19964=CARTESIAN_POINT('Ctrl Pts',(0.147945095322541,0.0480452627835881,
1.8342398590029));
#19965=CARTESIAN_POINT('Ctrl Pts',(0.146940498640245,0.0511022643155373,
1.83446854775261));
#19966=CARTESIAN_POINT('Ctrl Pts',(0.146040333109687,0.053620658169714,
1.83465496131582));
#19967=CARTESIAN_POINT('Ctrl Pts',(0.139792189951052,0.0697742106026303,
1.83584546365845));
#19968=CARTESIAN_POINT('Ctrl Pts',(0.132605760892131,0.0826203013978173,
1.83677421386824));
#19969=CARTESIAN_POINT('Ctrl Pts',(0.122525980638904,0.095849447959219,
1.83789175117716));
#19970=CARTESIAN_POINT('Ctrl Pts',(0.121294500062462,0.0974031641989691,
1.8380257341323));
#19971=CARTESIAN_POINT('Ctrl Pts',(0.117532433172077,0.101967620598429,
1.83842840073955));
#19972=CARTESIAN_POINT('Ctrl Pts',(0.114917183916687,0.104906171616982,
1.83869980622522));
#19973=CARTESIAN_POINT('Ctrl Pts',(0.111537998011291,0.108424966472421,
1.83904234511952));
#19974=CARTESIAN_POINT('Ctrl Pts',(0.110876199861009,0.109101634216439,
1.83910906154016));
#19975=CARTESIAN_POINT('Ctrl Pts',(0.10982657322855,0.110155430521953,1.83921432763862));
#19976=CARTESIAN_POINT('Ctrl Pts',(0.10944287425874,0.110536656006763,1.83925269564785));
#19977=CARTESIAN_POINT('Ctrl Pts',(0.108762269989605,0.11120585507206,1.83932055947829));
#19978=CARTESIAN_POINT('Ctrl Pts',(0.108466188023637,0.111494661868445,
1.83935001843572));
#19979=CARTESIAN_POINT('Ctrl Pts',(0.107785543376571,0.112153304925547,
1.8394175970538));
#19980=CARTESIAN_POINT('Ctrl Pts',(0.10740022451946,0.112522348565853,1.83945575055955));
#19981=CARTESIAN_POINT('Ctrl Pts',(0.106331536040258,0.113535407207977,
1.83956129223723));
#19982=CARTESIAN_POINT('Ctrl Pts',(0.105644231564068,0.114175218466854,
1.83962885908791));
#19983=CARTESIAN_POINT('Ctrl Pts',(0.101762631557791,0.117723541423356,
1.84000878330593));
#19984=CARTESIAN_POINT('Ctrl Pts',(0.0984543531845678,0.120503937292651,
1.84032643315056));
#19985=CARTESIAN_POINT('Ctrl Pts',(0.0876887107061473,0.128812275736433,
1.84134267010741));
#19986=CARTESIAN_POINT('Ctrl Pts',(0.0798508008916404,0.133812249993449,
1.84205912617447));
#19987=CARTESIAN_POINT('Ctrl Pts',(0.063869432813875,0.142100795277643,
1.84345531006633));
#19988=CARTESIAN_POINT('Ctrl Pts',(0.0557983230588078,0.145459693439072,
1.84413190748522));
#19989=CARTESIAN_POINT('Ctrl Pts',(0.0463798087230875,0.148479185020984,
1.84486312267671));
#19990=CARTESIAN_POINT('Ctrl Pts',(0.0452683488239298,0.14882181242591,
1.84494850821844));
#19991=CARTESIAN_POINT('Ctrl Pts',(0.0437474753535629,0.149272033066379,
1.84506402214846));
#19992=CARTESIAN_POINT('Ctrl Pts',(0.0433413493375018,0.149390457876521,
1.84509474036294));
#19993=CARTESIAN_POINT('Ctrl Pts',(0.042696897616408,0.149575528304435,
1.8451432767349));
#19994=CARTESIAN_POINT('Ctrl Pts',(0.0424588914603739,0.14964326336967,
1.84516115710521));
#19995=CARTESIAN_POINT('Ctrl Pts',(0.0419830460689904,0.149777459337608,
1.84519681432051));
#19996=CARTESIAN_POINT('Ctrl Pts',(0.0417452103449352,0.149843921788952,
1.84521459088366));
#19997=CARTESIAN_POINT('Ctrl Pts',(0.0412001750947033,0.149994831822142,
1.84525522607425));
#19998=CARTESIAN_POINT('Ctrl Pts',(0.0408928704552919,0.150078903087757,
1.8452780629343));
#19999=CARTESIAN_POINT('Ctrl Pts',(0.0399183311950965,0.150342298394119,
1.8453502555376));
#20000=CARTESIAN_POINT('Ctrl Pts',(0.0392501462326343,0.15051812488837,
1.84539941460077));
#20001=CARTESIAN_POINT('Ctrl Pts',(0.0376800354154955,0.150920117894542,
1.84551418364878));
#20002=CARTESIAN_POINT('Ctrl Pts',(0.0367771982865184,0.151142663882436,
1.84557960291966));
#20003=CARTESIAN_POINT('Ctrl Pts',(0.0260358983979863,0.15368840576173,
1.84635170687233));
#20004=CARTESIAN_POINT('Ctrl Pts',(0.0159939699430354,0.155055637559006,
1.84701287198638));
#20005=CARTESIAN_POINT('Ctrl Pts',(-0.00477519838170218,0.155842517043863,
1.84838083111003));
#20006=CARTESIAN_POINT('Ctrl Pts',(-0.0154511770288652,0.155148025289232,
1.84908550015695));
#20007=CARTESIAN_POINT('Ctrl Pts',(-0.0277029342446309,0.153073298042157,
1.8499489559353));
#20008=CARTESIAN_POINT('Ctrl Pts',(-0.0294294398859672,0.15275076029185,
1.8500718556735));
#20009=CARTESIAN_POINT('Ctrl Pts',(-0.0318418007782946,0.152257678713395,
1.85024545977228));
#20010=CARTESIAN_POINT('Ctrl Pts',(-0.0325325655679186,0.152111581255175,
1.85029538769803));
#20011=CARTESIAN_POINT('Ctrl Pts',(-0.0336466039222151,0.151868025541415,
1.85037627150864));
#20012=CARTESIAN_POINT('Ctrl Pts',(-0.0340705118489478,0.151773486988713,
1.85040713391551));
#20013=CARTESIAN_POINT('Ctrl Pts',(-0.0349517304995187,0.151573082618227,
1.85047147030397));
#20014=CARTESIAN_POINT('Ctrl Pts',(-0.0354089684165464,0.151466919774893,
1.85050495350313));
#20015=CARTESIAN_POINT('Ctrl Pts',(-0.0364860651375931,0.151211692650571,
1.85058407059821));
#20016=CARTESIAN_POINT('Ctrl Pts',(-0.0371054977746631,0.151060884930411,
1.85062976001696));
#20017=CARTESIAN_POINT('Ctrl Pts',(-0.0391457136313872,0.150550866002977,
1.8507808845945));
#20018=CARTESIAN_POINT('Ctrl Pts',(-0.0405623092609289,0.150175393936783,
1.85088684038298));
#20019=CARTESIAN_POINT('Ctrl Pts',(-0.0438918500549089,0.149242345557987,
1.85113838253134));
#20020=CARTESIAN_POINT('Ctrl Pts',(-0.0457997631904259,0.148667929376365,
1.85128449512738));
#20021=CARTESIAN_POINT('Ctrl Pts',(-0.0526889163383386,0.146448613827277,
1.8518194535888));
#20022=CARTESIAN_POINT('Ctrl Pts',(-0.0575967032354593,0.144588822137862,
1.85221485904219));
#20023=CARTESIAN_POINT('Ctrl Pts',(-0.06283094935431,0.142296503403254,
1.85265170021791));
#20024=CARTESIAN_POINT('Ctrl Pts',(-0.063260249095217,0.142106171054403,
1.85268764120887));
#20025=CARTESIAN_POINT('Ctrl Pts',(-0.0636886270478348,0.141913922096325,
1.85272361624831));
#20026=CARTESIAN_POINT('Origin',(0.,0.,-0.129405622560373));
#20027=CARTESIAN_POINT('',(-0.0636886188644129,0.141913925768909,1.93667989110148));
#20028=CARTESIAN_POINT('',(-0.0637929161402304,0.142146585575849,1.92279372449516));
#20029=CARTESIAN_POINT('',(-0.0636886258329924,0.141913922641526,-0.129405622560373));
#20030=CARTESIAN_POINT('Ctrl Pts',(-0.0636886188644129,0.141913925768909,
1.93667989110148));
#20031=CARTESIAN_POINT('Ctrl Pts',(-0.0623139118484019,0.142530871503576,
1.93656459384097));
#20032=CARTESIAN_POINT('Ctrl Pts',(-0.0609299693695357,0.143127963941791,
1.93644886047932));
#20033=CARTESIAN_POINT('Ctrl Pts',(-0.0517943039187702,0.14691288511572,
1.93568741913531));
#20034=CARTESIAN_POINT('Ctrl Pts',(-0.0438049553579604,0.14948969874181,
1.93503240351246));
#20035=CARTESIAN_POINT('Ctrl Pts',(-0.0312589033511584,0.152443451415049,
1.93404478225449));
#20036=CARTESIAN_POINT('Ctrl Pts',(-0.026827496764667,0.153285417555423,
1.93370371892127));
#20037=CARTESIAN_POINT('Ctrl Pts',(-0.0214448949121712,0.154067465911734,
1.93330327514698));
#20038=CARTESIAN_POINT('Ctrl Pts',(-0.0205232561249677,0.154192942906666,
1.93323519557578));
#20039=CARTESIAN_POINT('Ctrl Pts',(-0.0192288309749084,0.154357361143084,
1.93314031154491));
#20040=CARTESIAN_POINT('Ctrl Pts',(-0.0188569699294528,0.154403230447954,
1.93311313799678));
#20041=CARTESIAN_POINT('Ctrl Pts',(-0.0182220015482922,0.154479226070539,
1.93306688649942));
#20042=CARTESIAN_POINT('Ctrl Pts',(-0.0179589779841986,0.154510024729143,
1.93304777115586));
#20043=CARTESIAN_POINT('Ctrl Pts',(-0.0174537511212499,0.154567876556912,
1.93301113852488));
#20044=CARTESIAN_POINT('Ctrl Pts',(-0.0172115624190806,0.154595032303292,
1.93299361537522));
#20045=CARTESIAN_POINT('Ctrl Pts',(-0.0165682151779505,0.154665637940117,
1.93294716369307));
#20046=CARTESIAN_POINT('Ctrl Pts',(-0.0161669459236324,0.154708096694891,
1.93291829049311));
#20047=CARTESIAN_POINT('Ctrl Pts',(-0.0147343356668726,0.154854048087741,
1.93281554837794));
#20048=CARTESIAN_POINT('Ctrl Pts',(-0.0137021001236858,0.154948796261485,
1.93274214984823));
#20049=CARTESIAN_POINT('Ctrl Pts',(-0.000670994318541644,0.156013668215569,
1.93182261060386));
#20050=CARTESIAN_POINT('Ctrl Pts',(0.0114024185719397,0.155598210855758,
1.93104392642662));
#20051=CARTESIAN_POINT('Ctrl Pts',(0.0332150902691036,0.152292320637181,
1.92958910232593));
#20052=CARTESIAN_POINT('Ctrl Pts',(0.0429516234219893,0.149837594639623,
1.92892106207387));
#20053=CARTESIAN_POINT('Ctrl Pts',(0.0531768037239526,0.146180503189244,
1.92816119596865));
#20054=CARTESIAN_POINT('Ctrl Pts',(0.0539675716987259,0.145890414773736,
1.92810205404783));
#20055=CARTESIAN_POINT('Ctrl Pts',(0.0552742669836312,0.14539898411847,
1.92800367805756));
#20056=CARTESIAN_POINT('Ctrl Pts',(0.0557915519445576,0.145201280609501,
1.92796456429893));
#20057=CARTESIAN_POINT('Ctrl Pts',(0.0567947883230385,0.144811696626983,
1.92788837004811));
#20058=CARTESIAN_POINT('Ctrl Pts',(0.0572808510281883,0.144620121539214,
1.92785130014233));
#20059=CARTESIAN_POINT('Ctrl Pts',(0.0577670814972464,0.144425644526231,
1.9278140601499));
#20060=CARTESIAN_POINT('Ctrl Pts',(0.0577682289553095,0.144425185562954,
1.92781397226615));
#20061=CARTESIAN_POINT('Ctrl Pts',(0.0577705286696384,0.14442426568541,
1.92781379612939));
#20062=CARTESIAN_POINT('Ctrl Pts',(0.0577716809171636,0.144423804774507,
1.92781370787704));
#20063=CARTESIAN_POINT('Ctrl Pts',(0.0577739902531458,0.144422880984219,
1.9278135309998));
#20064=CARTESIAN_POINT('Ctrl Pts',(0.0577751473352169,0.144422418107254,
1.92781344237538));
#20065=CARTESIAN_POINT('Ctrl Pts',(0.0577774663928809,0.144421490363398,
1.92781326474995));
#20066=CARTESIAN_POINT('Ctrl Pts',(0.0577786283594959,0.144421025499963,
1.92781317574961));
#20067=CARTESIAN_POINT('Ctrl Pts',(0.0577809572255915,0.144420093767015,
1.92781299736929));
#20068=CARTESIAN_POINT('Ctrl Pts',(0.057782124121597,0.144419626898754,
1.92781290798957));
#20069=CARTESIAN_POINT('Ctrl Pts',(0.0577844628997235,0.144418691134434,
1.92781272884639));
#20070=CARTESIAN_POINT('Ctrl Pts',(0.0577856347748191,0.144418222241045,
1.92781263908345));
#20071=CARTESIAN_POINT('Ctrl Pts',(0.0577879835587649,0.144417282406983,
1.92781245917018));
#20072=CARTESIAN_POINT('Ctrl Pts',(0.0577891604607995,0.144416811468895,
1.92781236902035));
#20073=CARTESIAN_POINT('Ctrl Pts',(0.0577915193551739,0.144415867522377,
1.92781218832892));
#20074=CARTESIAN_POINT('Ctrl Pts',(0.0577927013373603,0.144415394517866,
1.92781209778809));
#20075=CARTESIAN_POINT('Ctrl Pts',(0.057795070432269,0.144414446421968,
1.92781191631155));
#20076=CARTESIAN_POINT('Ctrl Pts',(0.0577962575422328,0.144413971331538,
1.92781182537605));
#20077=CARTESIAN_POINT('Ctrl Pts',(0.0577986369423441,0.144413019043491,
1.92781164310634));
#20078=CARTESIAN_POINT('Ctrl Pts',(0.0577998292292903,0.144412541847007,
1.92781155177237));
#20079=CARTESIAN_POINT('Ctrl Pts',(0.0578022190430724,0.144411585322508,
1.92781136870113));
#20080=CARTESIAN_POINT('Ctrl Pts',(0.0578034165613076,0.144411105997784,
1.92781127696451));
#20081=CARTESIAN_POINT('Ctrl Pts',(0.0578058168844282,0.144410145197635,
1.92781109308437));
#20082=CARTESIAN_POINT('Ctrl Pts',(0.0578070196837962,0.144409663724265,
1.92781100094125));
#20083=CARTESIAN_POINT('Ctrl Pts',(0.0578094306291128,0.144408698602372,
1.9278108162435));
#20084=CARTESIAN_POINT('Ctrl Pts',(0.0578106387657814,0.144408214957409,
1.92781072368956));
#20085=CARTESIAN_POINT('Ctrl Pts',(0.0578130604282165,0.144407245474843,
1.92781053816687));
#20086=CARTESIAN_POINT('Ctrl Pts',(0.057814273951153,0.144406759638215,
1.92781044519834));
#20087=CARTESIAN_POINT('Ctrl Pts',(0.0578167064520139,0.144405785745466,
1.92781025884137));
#20088=CARTESIAN_POINT('Ctrl Pts',(0.0578179254201832,0.144405297693089,
1.92781016545369));
#20089=CARTESIAN_POINT('Ctrl Pts',(0.0578203688550495,0.14440431935093,
1.92780997825508));
#20090=CARTESIAN_POINT('Ctrl Pts',(0.057821593319676,0.144403829061813,
1.9278098844443));
#20091=CARTESIAN_POINT('Ctrl Pts',(0.0578240478057935,0.144402846222325,
1.927809696395));
#20092=CARTESIAN_POINT('Ctrl Pts',(0.0578252778222605,0.144402353673801,
1.92780960215685));
#20093=CARTESIAN_POINT('Ctrl Pts',(0.0578277434745848,0.144401366289966,
1.927809413248));
#20094=CARTESIAN_POINT('Ctrl Pts',(0.0578289791022361,0.144400871457773,
1.92780931857791));
#20095=CARTESIAN_POINT('Ctrl Pts',(0.0578314560243601,0.144399879487104,
1.92780912880152));
#20096=CARTESIAN_POINT('Ctrl Pts',(0.0578326973169664,0.144399382349204,
1.92780903369534));
#20097=CARTESIAN_POINT('Ctrl Pts',(0.0578351856314596,0.144398385741596,
1.92780884304196));
#20098=CARTESIAN_POINT('Ctrl Pts',(0.0578364326485176,0.144397886273649,
1.9278087474951));
#20099=CARTESIAN_POINT('Ctrl Pts',(0.057838932463049,0.144396884984946,
1.92780855595642));
#20100=CARTESIAN_POINT('Ctrl Pts',(0.0578401852584092,0.144396383164863,
1.92780845996474));
#20101=CARTESIAN_POINT('Ctrl Pts',(0.0578426966671834,0.144395377156286,
1.92780826753348));
#20102=CARTESIAN_POINT('Ctrl Pts',(0.057843955267745,0.144394872972768,
1.92780817109488));
#20103=CARTESIAN_POINT('Ctrl Pts',(0.058263349400423,0.144226861272854,
1.92777603522118));
#20104=CARTESIAN_POINT('Ctrl Pts',(0.0586807511613323,0.144057540001483,
1.92774393501312));
#20105=CARTESIAN_POINT('Ctrl Pts',(0.0596249573297357,0.143669733141378,
1.92767105218755));
#20106=CARTESIAN_POINT('Ctrl Pts',(0.0601513048402488,0.143450159524081,
1.92763023315416));
#20107=CARTESIAN_POINT('Ctrl Pts',(0.0616491619313125,0.142815613159336,
1.9275135199763));
#20108=CARTESIAN_POINT('Ctrl Pts',(0.0626176511231864,0.142393638180758,
1.9274373892381));
#20109=CARTESIAN_POINT('Ctrl Pts',(0.0689594296508403,0.139553287951784,
1.92693438521286));
#20110=CARTESIAN_POINT('Ctrl Pts',(0.0741951774994299,0.136841448071204,
1.9264974890208));
#20111=CARTESIAN_POINT('Ctrl Pts',(0.0886274701633403,0.12829419562457,
1.92522888995344));
#20112=CARTESIAN_POINT('Ctrl Pts',(0.0973826318216243,0.121781805653149,
1.92437757624002));
#20113=CARTESIAN_POINT('Ctrl Pts',(0.108462282707068,0.111576142891768,
1.9232170303326));
#20114=CARTESIAN_POINT('Ctrl Pts',(0.111423856662008,0.108618747148631,
1.92289749086033));
#20115=CARTESIAN_POINT('Ctrl Pts',(0.115705287199864,0.103983693219156,
1.92242520471983));
#20116=CARTESIAN_POINT('Ctrl Pts',(0.117115706861975,0.102392550395139,
1.92226778376168));
#20117=CARTESIAN_POINT('Ctrl Pts',(0.118821857108639,0.100386384550469,
1.92207554879086));
#20118=CARTESIAN_POINT('Ctrl Pts',(0.11914867290999,0.0999982684501449,
1.92203864094211));
#20119=CARTESIAN_POINT('Ctrl Pts',(0.119661612000995,0.099383033384467,
1.92198058835522));
#20120=CARTESIAN_POINT('Ctrl Pts',(0.119848997320651,0.0991569793636126,
1.92195935398295));
#20121=CARTESIAN_POINT('Ctrl Pts',(0.120200351758247,0.0987306686046086,
1.92191949035984));
#20122=CARTESIAN_POINT('Ctrl Pts',(0.120364459124811,0.0985305357081057,
1.92190085145918));
#20123=CARTESIAN_POINT('Ctrl Pts',(0.120737300986166,0.0980735244724467,
1.92185845837926));
#20124=CARTESIAN_POINT('Ctrl Pts',(0.120945715434853,0.097816389093736,
1.92183472733057));
#20125=CARTESIAN_POINT('Ctrl Pts',(0.121594618114691,0.097010548112544,
1.92176072704574));
#20126=CARTESIAN_POINT('Ctrl Pts',(0.122032213544002,0.0964595070853536,
1.92171065978423));
#20127=CARTESIAN_POINT('Ctrl Pts',(0.12721840456848,0.0898370255894188,
1.92111504142826));
#20128=CARTESIAN_POINT('Ctrl Pts',(0.131513918716525,0.0834226674214282,
1.92059877771323));
#20129=CARTESIAN_POINT('Ctrl Pts',(0.136027103254726,0.0754619459107344,
1.91999332196306));
#20130=CARTESIAN_POINT('Ctrl Pts',(0.136720195103678,0.0741988303345223,
1.91989825731979));
#20131=CARTESIAN_POINT('Ctrl Pts',(0.141835793118025,0.0645608630874822,
1.91917917413033));
#20132=CARTESIAN_POINT('Ctrl Pts',(0.145502367260375,0.055808084062282,
1.91856029763987));
#20133=CARTESIAN_POINT('Ctrl Pts',(0.14966388251135,0.0426099853983275,
1.91762092243679));
#20134=CARTESIAN_POINT('Ctrl Pts',(0.150801413108891,0.0383903154641012,
1.91731996413983));
#20135=CARTESIAN_POINT('Ctrl Pts',(0.151966538816563,0.0332093583025964,
1.91694702433368));
#20136=CARTESIAN_POINT('Ctrl Pts',(0.152164920032293,0.0322881935172756,
1.91688059033774));
#20137=CARTESIAN_POINT('Ctrl Pts',(0.152462665451181,0.030841914450291,
1.91677606324851));
#20138=CARTESIAN_POINT('Ctrl Pts',(0.152567716070872,0.0303179821788781,
1.91673815157947));
#20139=CARTESIAN_POINT('Ctrl Pts',(0.152749314471582,0.0293874229549187,
1.91667073125739));
#20140=CARTESIAN_POINT('Ctrl Pts',(0.152826943796132,0.0289810100468157,
1.91664125732049));
#20141=CARTESIAN_POINT('Ctrl Pts',(0.153002218912614,0.0280431012866468,
1.91657316934394));
#20142=CARTESIAN_POINT('Ctrl Pts',(0.153098717875223,0.0275113993338287,
1.9165345192866));
#20143=CARTESIAN_POINT('Ctrl Pts',(0.153356150227412,0.026049655686807,
1.91642811753844));
#20144=CARTESIAN_POINT('Ctrl Pts',(0.153511389780534,0.0251186486230227,
1.91636018665901));
#20145=CARTESIAN_POINT('Ctrl Pts',(0.15426419225691,0.0203360152192596,
1.91601033961286));
#20146=CARTESIAN_POINT('Ctrl Pts',(0.154725255158399,0.0164646564458348,
1.91572417036638));
#20147=CARTESIAN_POINT('Ctrl Pts',(0.155203329134184,0.0105728759093058,
1.91528367340942));
#20148=CARTESIAN_POINT('Ctrl Pts',(0.1553272104684,0.00856248482435424,
1.91513250411983));
#20149=CARTESIAN_POINT('Ctrl Pts',(0.156028991951178,-0.00808786285475393,
1.91387357579896));
#20150=CARTESIAN_POINT('Ctrl Pts',(0.154574863219057,-0.022737484364409,
1.91271208571841));
#20151=CARTESIAN_POINT('Ctrl Pts',(0.150457012439278,-0.0395685038675411,
1.91140745841941));
#20152=CARTESIAN_POINT('Ctrl Pts',(0.149753199934081,-0.0421540099016685,
1.91120821240737));
#20153=CARTESIAN_POINT('Ctrl Pts',(0.14882635930982,-0.0452417254090879,
1.9109726790923));
#20154=CARTESIAN_POINT('Ctrl Pts',(0.148667086556234,-0.0457623900394041,
1.91093304609735));
#20155=CARTESIAN_POINT('Ctrl Pts',(0.148415293903251,-0.0465703134641446,
1.91087168863046));
#20156=CARTESIAN_POINT('Ctrl Pts',(0.148324668573028,-0.0468581503846347,
1.91084985699857));
#20157=CARTESIAN_POINT('Ctrl Pts',(0.148155097894984,-0.0473913059371092,
1.91080947299888));
#20158=CARTESIAN_POINT('Ctrl Pts',(0.148076381296406,-0.0476366897966697,
1.91079090801075));
#20159=CARTESIAN_POINT('Ctrl Pts',(0.147897175919077,-0.0481905917348518,
1.91074904956525));
#20160=CARTESIAN_POINT('Ctrl Pts',(0.147796331645468,-0.0484989910611065,
1.91072577725864));
#20161=CARTESIAN_POINT('Ctrl Pts',(0.147496274558364,-0.0494069902958142,
1.91065735060439));
#20162=CARTESIAN_POINT('Ctrl Pts',(0.147294369399312,-0.0500057044594937,
1.91061235063989));
#20163=CARTESIAN_POINT('Ctrl Pts',(0.145824664325777,-0.0542777118261522,
1.91029200147478));
#20164=CARTESIAN_POINT('Ctrl Pts',(0.144423123413583,-0.057903977461674,
1.91002398578684));
#20165=CARTESIAN_POINT('Ctrl Pts',(0.137997202822195,-0.0728399901529379,
1.90892136321839));
#20166=CARTESIAN_POINT('Ctrl Pts',(0.13176851512132,-0.0835822783268564,
1.90812824162826));
#20167=CARTESIAN_POINT('Ctrl Pts',(0.121675761418994,-0.097006975209353,
1.90700538139795));
#20168=CARTESIAN_POINT('Ctrl Pts',(0.118870109722951,-0.10042527567558,
1.90670642910167));
#20169=CARTESIAN_POINT('Ctrl Pts',(0.114138129585178,-0.105714021259405,
1.90621771070855));
#20170=CARTESIAN_POINT('Ctrl Pts',(0.11230228023296,-0.107662264840207,
1.90603149136525));
#20171=CARTESIAN_POINT('Ctrl Pts',(0.109851135057086,-0.110132540395431,
1.90578655647061));
#20172=CARTESIAN_POINT('Ctrl Pts',(0.10928069072764,-0.110698594922814,
1.90572980445913));
#20173=CARTESIAN_POINT('Ctrl Pts',(0.108345587247929,-0.111612230401133,
1.90563716229442));
#20174=CARTESIAN_POINT('Ctrl Pts',(0.107983575257947,-0.111962510309686,
1.9056013904273));
#20175=CARTESIAN_POINT('Ctrl Pts',(0.107283980489765,-0.112632883512432,
1.90553243498937));
#20176=CARTESIAN_POINT('Ctrl Pts',(0.106946650103483,-0.112953233424516,
1.90549926302742));
#20177=CARTESIAN_POINT('Ctrl Pts',(0.106170817040806,-0.11368342165538,
1.90542314207001));
#20178=CARTESIAN_POINT('Ctrl Pts',(0.105731371493073,-0.114092242566667,
1.9053801502359));
#20179=CARTESIAN_POINT('Ctrl Pts',(0.104557360878036,-0.115171829421012,
1.90526561526976));
#20180=CARTESIAN_POINT('Ctrl Pts',(0.103818719463163,-0.115838099990894,
1.90519388408949));
#20181=CARTESIAN_POINT('Ctrl Pts',(0.0982094045153399,-0.120801077818922,
1.90465152504069));
#20182=CARTESIAN_POINT('Ctrl Pts',(0.0930810058893311,-0.1247953988602,
1.90416858222044));
#20183=CARTESIAN_POINT('Ctrl Pts',(0.0790913646547553,-0.134348414460681,
1.90288243823438));
#20184=CARTESIAN_POINT('Ctrl Pts',(0.0698928320481996,-0.139355299402337,
1.90206491437551));
#20185=CARTESIAN_POINT('Ctrl Pts',(0.0565477471750089,-0.144963435782579,
1.90095065518525));
#20186=CARTESIAN_POINT('Ctrl Pts',(0.0527726565901035,-0.14637997583789,
1.90064314923597));
#20187=CARTESIAN_POINT('Ctrl Pts',(0.0469777448818165,-0.148301031846785,
1.90018646657215));
#20188=CARTESIAN_POINT('Ctrl Pts',(0.044995974897906,-0.148914297332099,
1.90003294433012));
#20189=CARTESIAN_POINT('Ctrl Pts',(0.0425186630961812,-0.149626933262349,
1.89984480049977));
#20190=CARTESIAN_POINT('Ctrl Pts',(0.0420342409723471,-0.149763742186795,
1.89980818772617));
#20191=CARTESIAN_POINT('Ctrl Pts',(0.041267062793292,-0.149976390534752,
1.89975049369711));
#20192=CARTESIAN_POINT('Ctrl Pts',(0.0409847479424406,-0.150053785788246,
1.89972932462665));
#20193=CARTESIAN_POINT('Ctrl Pts',(0.0404522447870206,-0.150198154011838,
1.89968951406292));
#20194=CARTESIAN_POINT('Ctrl Pts',(0.0402021108516058,-0.150265298260502,
1.89967086325216));
#20195=CARTESIAN_POINT('Ctrl Pts',(0.0396305107052771,-0.15041720527188,
1.89962835431003));
#20196=CARTESIAN_POINT('Ctrl Pts',(0.0393089398654413,-0.150501562360012,
1.89960451977919));
#20197=CARTESIAN_POINT('Ctrl Pts',(0.0384559687603771,-0.15072240037002,
1.89954150448339));
#20198=CARTESIAN_POINT('Ctrl Pts',(0.0379241061700692,-0.150857103583914,
1.89950242348854));
#20199=CARTESIAN_POINT('Ctrl Pts',(0.0342445308266668,-0.151768328666505,
1.89923343862731));
#20200=CARTESIAN_POINT('Ctrl Pts',(0.0310736355660963,-0.152449160651027,
1.89900864384737));
#20201=CARTESIAN_POINT('Ctrl Pts',(0.027113845374644,-0.153170669212571,
1.89873391068488));
#20202=CARTESIAN_POINT('Ctrl Pts',(0.0263431413328027,-0.153305099275667,
1.89868071803145));
#20203=CARTESIAN_POINT('Ctrl Pts',(0.0133147919287953,-0.155476419337986,
1.89778573908806));
#20204=CARTESIAN_POINT('Ctrl Pts',(0.000856941605050558,-0.156043300709219,
1.89698938853222));
#20205=CARTESIAN_POINT('Ctrl Pts',(-0.0158528065020981,-0.154800599955869,
1.89586831877824));
#20206=CARTESIAN_POINT('Ctrl Pts',(-0.0201536477079932,-0.154299587793208,
1.89557538589128));
#20207=CARTESIAN_POINT('Ctrl Pts',(-0.0270315373814551,-0.153205906079514,
1.89509559942364));
#20208=CARTESIAN_POINT('Ctrl Pts',(-0.029624239166737,-0.152725756468644,
1.89491212630646));
#20209=CARTESIAN_POINT('Ctrl Pts',(-0.0329853476588799,-0.152014500059913,
1.89467030267045));
#20210=CARTESIAN_POINT('Ctrl Pts',(-0.0337660351773859,-0.151842998568413,
1.89461385319813));
#20211=CARTESIAN_POINT('Ctrl Pts',(-0.0350355787411722,-0.151553830407656,
1.8945215820698));
#20212=CARTESIAN_POINT('Ctrl Pts',(-0.0355252545715611,-0.151439795185312,
1.89448587690474));
#20213=CARTESIAN_POINT('Ctrl Pts',(-0.0364672412318426,-0.151215606113075,
1.89441696476968));
#20214=CARTESIAN_POINT('Ctrl Pts',(-0.0369196280042995,-0.151105791664543,
1.89438376902945));
#20215=CARTESIAN_POINT('Ctrl Pts',(-0.0379561795988101,-0.150849241656922,
1.89430747264136));
#20216=CARTESIAN_POINT('Ctrl Pts',(-0.0385399955190969,-0.150701141351702,
1.89426432848549));
#20217=CARTESIAN_POINT('Ctrl Pts',(-0.0400926221504664,-0.150297664497885,
1.89414912260764));
#20218=CARTESIAN_POINT('Ctrl Pts',(-0.0410598363381574,-0.150036315793711,
1.89407686932073));
#20219=CARTESIAN_POINT('Ctrl Pts',(-0.0485572933935458,-0.147932519482521,
1.89351291813367));
#20220=CARTESIAN_POINT('Ctrl Pts',(-0.0549621882698234,-0.145674203725999,
1.89300773951047));
#20221=CARTESIAN_POINT('Ctrl Pts',(-0.0741008978795629,-0.137483890272898,
1.89142450855353));
#20222=CARTESIAN_POINT('Ctrl Pts',(-0.0861955022067965,-0.130242314560421,
1.8903125268345));
#20223=CARTESIAN_POINT('Ctrl Pts',(-0.098879039056098,-0.120098351628254,
1.88909576901242));
#20224=CARTESIAN_POINT('Ctrl Pts',(-0.100574065326758,-0.118682505787086,
1.88893214655533));
#20225=CARTESIAN_POINT('Ctrl Pts',(-0.102625517080303,-0.116893410734303,
1.88873342515567));
#20226=CARTESIAN_POINT('Ctrl Pts',(-0.10301088647724,-0.116553951097115,
1.88869606410842));
#20227=CARTESIAN_POINT('Ctrl Pts',(-0.103614958337856,-0.11601650711492,
1.88863746106276));
#20228=CARTESIAN_POINT('Ctrl Pts',(-0.10383478609371,-0.115819802777138,
1.88861612660645));
#20229=CARTESIAN_POINT('Ctrl Pts',(-0.104246254115159,-0.115449503513024,
1.88857618003708));
#20230=CARTESIAN_POINT('Ctrl Pts',(-0.104438018790505,-0.115276058186642,
1.88855755776809));
#20231=CARTESIAN_POINT('Ctrl Pts',(-0.104876734918884,-0.114877259443074,
1.88851494078897));
#20232=CARTESIAN_POINT('Ctrl Pts',(-0.1051233927569,-0.114651587714078,
1.8884909704763));
#20233=CARTESIAN_POINT('Ctrl Pts',(-0.105886020358606,-0.113949315736671,
1.88841681986465));
#20234=CARTESIAN_POINT('Ctrl Pts',(-0.10639950078149,-0.113470005496947,
1.88836683949049));
#20235=CARTESIAN_POINT('Ctrl Pts',(-0.111817851503183,-0.108343103499832,
1.88783862257071));
#20236=CARTESIAN_POINT('Ctrl Pts',(-0.116418926679245,-0.103383370112628,
1.88738282152953));
#20237=CARTESIAN_POINT('Ctrl Pts',(-0.126869503787302,-0.0905321453915931,
1.88628241338247));
#20238=CARTESIAN_POINT('Ctrl Pts',(-0.132322440281414,-0.0823572333029784,
1.88564671212012));
#20239=CARTESIAN_POINT('Ctrl Pts',(-0.138939060386207,-0.070064310026673,
1.88471129199374));
#20240=CARTESIAN_POINT('Ctrl Pts',(-0.140760978814372,-0.0663280668418696,
1.88442966549942));
#20241=CARTESIAN_POINT('Ctrl Pts',(-0.143460109140074,-0.0601793491092366,
1.88396671232258));
#20242=CARTESIAN_POINT('Ctrl Pts',(-0.144431086864539,-0.0578101790553955,
1.88378846569088));
#20243=CARTESIAN_POINT('Ctrl Pts',(-0.145624889027769,-0.0546792438807589,
1.88355257238348));
#20244=CARTESIAN_POINT('Ctrl Pts',(-0.145901018598313,-0.0539381196022179,
1.88349671071365));
#20245=CARTESIAN_POINT('Ctrl Pts',(-0.146342786573112,-0.0527242092940469,
1.88340516020472));
#20246=CARTESIAN_POINT('Ctrl Pts',(-0.146511816642267,-0.0522526650147942,
1.88336958439859));
#20247=CARTESIAN_POINT('Ctrl Pts',(-0.146833750503467,-0.0513407201127665,
1.88330075341295));
#20248=CARTESIAN_POINT('Ctrl Pts',(-0.146986958146747,-0.0509004317730084,
1.88326750871833));
#20249=CARTESIAN_POINT('Ctrl Pts',(-0.147334938952497,-0.049885730911101,
1.88319085862735));
#20250=CARTESIAN_POINT('Ctrl Pts',(-0.147528335133311,-0.049310857812194,
1.88314740837475));
#20251=CARTESIAN_POINT('Ctrl Pts',(-0.148036789552355,-0.0477697016574671,
1.88303085030205));
#20252=CARTESIAN_POINT('Ctrl Pts',(-0.148345743055192,-0.0468014517256314,
1.88295754373332));
#20253=CARTESIAN_POINT('Ctrl Pts',(-0.150816816489712,-0.0387868099640734,
1.88235001412697));
#20254=CARTESIAN_POINT('Ctrl Pts',(-0.15248473235312,-0.0315990997914103,
1.8817997888244));
#20255=CARTESIAN_POINT('Ctrl Pts',(-0.154916651951674,-0.0162367237744365,
1.88061301846293));
#20256=CARTESIAN_POINT('Ctrl Pts',(-0.155556275934555,-0.00806412838761236,
1.87997532808238));
#20257=CARTESIAN_POINT('Ctrl Pts',(-0.155544457945757,0.00723429139734965,
1.87879230499606));
#20258=CARTESIAN_POINT('Ctrl Pts',(-0.155050913173091,0.0143407065639603,
1.87824740076));
#20259=CARTESIAN_POINT('Ctrl Pts',(-0.153975580461275,0.0220866218302719,
1.87767406755209));
#20260=CARTESIAN_POINT('Ctrl Pts',(-0.153874026671416,0.0227833757103862,
1.87762268415822));
#20261=CARTESIAN_POINT('Ctrl Pts',(-0.153717768952236,0.0238067137171998,
1.87754751690442));
#20262=CARTESIAN_POINT('Ctrl Pts',(-0.153666749808939,0.0241338376219465,
1.87752353393448));
#20263=CARTESIAN_POINT('Ctrl Pts',(-0.153573985083642,0.0247164033597027,
1.87748090698197));
#20264=CARTESIAN_POINT('Ctrl Pts',(-0.153532646024826,0.024971906177771,
1.87746224040361));
#20265=CARTESIAN_POINT('Ctrl Pts',(-0.153443057870261,0.025516987892864,
1.87742248000592));
#20266=CARTESIAN_POINT('Ctrl Pts',(-0.153394626806776,0.0258065330954148,
1.87740139664903));
#20267=CARTESIAN_POINT('Ctrl Pts',(-0.153260296488616,0.0265958869554173,
1.87734401669949));
#20268=CARTESIAN_POINT('Ctrl Pts',(-0.153172771200874,0.0270954214691064,
1.87730781076817));
#20269=CARTESIAN_POINT('Ctrl Pts',(-0.152706232573947,0.0296835809709499,
1.8771207322495));
#20270=CARTESIAN_POINT('Ctrl Pts',(-0.152286913802738,0.0317648475622439,
1.87697201588019));
#20271=CARTESIAN_POINT('Ctrl Pts',(-0.150917164327716,0.0379108489640523,
1.87653620315642));
#20272=CARTESIAN_POINT('Ctrl Pts',(-0.149845556839695,0.0419468470795809,
1.87625437320726));
#20273=CARTESIAN_POINT('Ctrl Pts',(-0.145434218170894,0.0562187314632048,
1.87525772836485));
#20274=CARTESIAN_POINT('Ctrl Pts',(-0.141196900559897,0.0661445512695426,
1.87456249020457));
#20275=CARTESIAN_POINT('Ctrl Pts',(-0.134996332502071,0.0773032969624332,
1.87370628778152));
#20276=CARTESIAN_POINT('Ctrl Pts',(-0.133990388490475,0.0790340739154274,
1.87357126928923));
#20277=CARTESIAN_POINT('Ctrl Pts',(-0.130775697066839,0.0843272569238734,
1.87315055681715));
#20278=CARTESIAN_POINT('Ctrl Pts',(-0.128456330161063,0.0878199013314235,
1.87286173320249));
#20279=CARTESIAN_POINT('Ctrl Pts',(-0.12548286323063,0.0919272979402839,
1.87250580958281));
#20280=CARTESIAN_POINT('Ctrl Pts',(-0.12496074350913,0.0926357900390331,
1.87244380866279));
#20281=CARTESIAN_POINT('Ctrl Pts',(-0.124089448417226,0.0937973262303442,
1.872341131904));
#20282=CARTESIAN_POINT('Ctrl Pts',(-0.123743731231153,0.0942529499888229,
1.87230059078509));
#20283=CARTESIAN_POINT('Ctrl Pts',(-0.123114986575457,0.0950721561212634,
1.87222721170615));
#20284=CARTESIAN_POINT('Ctrl Pts',(-0.122832840070679,0.0954364090943262,
1.87219440868164));
#20285=CARTESIAN_POINT('Ctrl Pts',(-0.122225581883589,0.0962132295523254,
1.87212407114285));
#20286=CARTESIAN_POINT('Ctrl Pts',(-0.12189999123172,0.096625413493972,
1.8720865178758));
#20287=CARTESIAN_POINT('Ctrl Pts',(-0.121010337686681,0.0977400237365894,
1.87198433011952));
#20288=CARTESIAN_POINT('Ctrl Pts',(-0.120442257845122,0.0984392021951439,
1.87191953534296));
#20289=CARTESIAN_POINT('Ctrl Pts',(-0.117469973491451,0.10203316996237,
1.87158280784333));
#20290=CARTESIAN_POINT('Ctrl Pts',(-0.114967576059303,0.10484471544802,
1.8713069023548));
#20291=CARTESIAN_POINT('Ctrl Pts',(-0.102060968398646,0.118327683623285,
1.86991837965263));
#20292=CARTESIAN_POINT('Ctrl Pts',(-0.0902630936237239,0.127555096863481,
1.86874389162985));
#20293=CARTESIAN_POINT('Ctrl Pts',(-0.0734494952110326,0.137189854357054,
1.86726265251107));
#20294=CARTESIAN_POINT('Ctrl Pts',(-0.0694663952417378,0.139249106793601,
1.86692486348299));
#20295=CARTESIAN_POINT('Ctrl Pts',(-0.0648307877395254,0.141397186401546,
1.86655061419595));
#20296=CARTESIAN_POINT('Ctrl Pts',(-0.0642604913790529,0.141657278824543,
1.86650489022365));
#20297=CARTESIAN_POINT('Ctrl Pts',(-0.0636886258329876,0.141913922641528,
1.86645936880636));
#20298=CARTESIAN_POINT('',(-0.155675768969518,-0.000119712528699489,1.86559437743963));
#20299=CARTESIAN_POINT('Ctrl Pts',(-0.0636886270478345,0.141913922096325,
1.85272361624831));
#20300=CARTESIAN_POINT('Ctrl Pts',(-0.0739703217922353,0.137299667114694,
1.85358706958847));
#20301=CARTESIAN_POINT('Ctrl Pts',(-0.0837207957971725,0.131581474202708,
1.8544734650818));
#20302=CARTESIAN_POINT('Ctrl Pts',(-0.0954374813874821,0.12287613518474,
1.85557961065035));
#20303=CARTESIAN_POINT('Ctrl Pts',(-0.0980423574854303,0.120807937720802,
1.85582824336486));
#20304=CARTESIAN_POINT('Ctrl Pts',(-0.101000676165513,0.118300343388413,
1.85611202326769));
#20305=CARTESIAN_POINT('Ctrl Pts',(-0.10142029150064,0.117940800100071,
1.85615230925228));
#20306=CARTESIAN_POINT('Ctrl Pts',(-0.102090117918159,0.117360647488134,
1.85621665968603));
#20307=CARTESIAN_POINT('Ctrl Pts',(-0.102341545652814,0.117141460612512,
1.85624082411406));
#20308=CARTESIAN_POINT('Ctrl Pts',(-0.102786992214986,0.11675060531303,
1.85628364972048));
#20309=CARTESIAN_POINT('Ctrl Pts',(-0.102981289211346,0.116579259244726,
1.85630233432925));
#20310=CARTESIAN_POINT('Ctrl Pts',(-0.1033562579006,0.116246913990354,1.85633840169611));
#20311=CARTESIAN_POINT('Ctrl Pts',(-0.103536980980482,0.116085979476988,
1.85635578908285));
#20312=CARTESIAN_POINT('Ctrl Pts',(-0.104043187633436,0.115633078263097,
1.85640450518398));
#20313=CARTESIAN_POINT('Ctrl Pts',(-0.104367820397992,0.11534015675098,
1.8564357632608));
#20314=CARTESIAN_POINT('Ctrl Pts',(-0.105712739453047,0.114116286474028,
1.85656535170528));
#20315=CARTESIAN_POINT('Ctrl Pts',(-0.106721881152471,0.113173099976523,
1.85666280233229));
#20316=CARTESIAN_POINT('Ctrl Pts',(-0.109358462369601,0.110642205671764,
1.85691842795796));
#20317=CARTESIAN_POINT('Ctrl Pts',(-0.110963941663144,0.109031994706482,
1.85707513982447));
#20318=CARTESIAN_POINT('Ctrl Pts',(-0.116693554900108,0.103027787559818,
1.85764101744125));
#20319=CARTESIAN_POINT('Ctrl Pts',(-0.120597001966021,0.0984301048361011,
1.85803966682445));
#20320=CARTESIAN_POINT('Ctrl Pts',(-0.131779987069992,0.0835909908354916,
1.85926402258546));
#20321=CARTESIAN_POINT('Ctrl Pts',(-0.138093314372199,0.0726884210134969,
1.86008394891692));
#20322=CARTESIAN_POINT('Ctrl Pts',(-0.143697582786388,0.0595794521520465,
1.86107518217491));
#20323=CARTESIAN_POINT('Ctrl Pts',(-0.144341638058565,0.0580017029021563,
1.86119447459827));
#20324=CARTESIAN_POINT('Ctrl Pts',(-0.145212492752673,0.0557639722027207,
1.86136380472771));
#20325=CARTESIAN_POINT('Ctrl Pts',(-0.145460988165458,0.0551125170960898,
1.86141311654423));
#20326=CARTESIAN_POINT('Ctrl Pts',(-0.145856582605158,0.0540541121188796,
1.86149326803461));
#20327=CARTESIAN_POINT('Ctrl Pts',(-0.14600638017302,0.0536481748811687,
1.86152401751783));
#20328=CARTESIAN_POINT('Ctrl Pts',(-0.14631557021811,0.0527994120318984,
1.86158833113908));
#20329=CARTESIAN_POINT('Ctrl Pts',(-0.146474650321893,0.0523564781406016,
1.86162190526874));
#20330=CARTESIAN_POINT('Ctrl Pts',(-0.146846838923133,0.0513052033476025,
1.86170162234134));
#20331=CARTESIAN_POINT('Ctrl Pts',(-0.147058179511942,0.0506962504305998,
1.86174782317378));
#20332=CARTESIAN_POINT('Ctrl Pts',(-0.14775068431541,0.0486601085436864,
1.8619023978486));
#20333=CARTESIAN_POINT('Ctrl Pts',(-0.148214890967004,0.0472272874315404,
1.86201132564933));
#20334=CARTESIAN_POINT('Ctrl Pts',(-0.149265480596585,0.0438163767856777,
1.86227108473056));
#20335=CARTESIAN_POINT('Ctrl Pts',(-0.14983344478335,0.0418329612643452,
1.86242248946604));
#20336=CARTESIAN_POINT('Ctrl Pts',(-0.153816563203144,0.0267997043518521,
1.86357309985241));
#20337=CARTESIAN_POINT('Ctrl Pts',(-0.15555984041361,0.0133688473671373,
1.86462559282136));
#20338=CARTESIAN_POINT('Ctrl Pts',(-0.155549958218615,-0.000114009591826104,
1.86566652523707));
#20339=CARTESIAN_POINT('Ctrl Pts',(-0.155675768969518,-0.000119712528699489,
1.86559437743963));
#20340=CARTESIAN_POINT('Ctrl Pts',(-0.155742030728685,-0.00790775711175682,
1.86615350633922));
#20341=CARTESIAN_POINT('Ctrl Pts',(-0.151670179225866,-0.0672314883108279,
1.87041753953273));
#20342=CARTESIAN_POINT('Ctrl Pts',(-0.0754025780794165,-0.16768394396421,
1.87838647702017));
#20343=CARTESIAN_POINT('Ctrl Pts',(0.0999993571785868,-0.154284096420481,
1.88950118990195));
#20344=CARTESIAN_POINT('Ctrl Pts',(0.183856812913126,0.000355232096483363,
1.90061590278373));
#20345=CARTESIAN_POINT('Ctrl Pts',(0.0995331275448493,0.154430543530984,
1.9117134143148));
#20346=CARTESIAN_POINT('Ctrl Pts',(-0.0170231057640074,0.163110781870857,
1.91910602155194));
#20347=CARTESIAN_POINT('Ctrl Pts',(-0.0637929161402304,0.142146585575849,
1.92279372449516));
#20348=CARTESIAN_POINT('Origin',(0.,0.,-0.129405622560373));
#20349=CARTESIAN_POINT('',(-0.0636886213818939,0.141913924639106,2.00672033358865));
#20350=CARTESIAN_POINT('',(-0.0636886415377123,0.141913915593506,1.99275019838839));
#20351=CARTESIAN_POINT('',(-0.0636886258329924,0.141913922641526,-0.129405622560373));
#20352=CARTESIAN_POINT('',(-0.155549993634555,4.4500446807104E-5,1.94954854470546));
#20353=CARTESIAN_POINT('Ctrl Pts',(-0.0636886213818939,0.141913924639106,
2.00672033358865));
#20354=CARTESIAN_POINT('Ctrl Pts',(-0.0604714569255569,0.143357734818438,
2.00648001356466));
#20355=CARTESIAN_POINT('Ctrl Pts',(-0.0572055352928224,0.144691995296332,
2.00623663332487));
#20356=CARTESIAN_POINT('Ctrl Pts',(-0.0529634226839831,0.146258906037987,
2.00591977835086));
#20357=CARTESIAN_POINT('Ctrl Pts',(-0.0520271660241615,0.146594562150063,
2.00584980477329));
#20358=CARTESIAN_POINT('Ctrl Pts',(-0.050520897669163,0.147118325172964,
2.00573713147982));
#20359=CARTESIAN_POINT('Ctrl Pts',(-0.0499528928161396,0.147312155588118,
2.00569462082771));
#20360=CARTESIAN_POINT('Ctrl Pts',(-0.0489426529835277,0.147650383106395,
2.00561896627509));
#20361=CARTESIAN_POINT('Ctrl Pts',(-0.0485008624848558,0.147796093460381,
2.00558586601961));
#20362=CARTESIAN_POINT('Ctrl Pts',(-0.0475793198585017,0.148095457699797,
2.00551678554075));
#20363=CARTESIAN_POINT('Ctrl Pts',(-0.0470994623809972,0.14824876694907,
2.00548079445697));
#20364=CARTESIAN_POINT('Ctrl Pts',(-0.0458521025636008,0.148640617430633,
2.00538718085255));
#20365=CARTESIAN_POINT('Ctrl Pts',(-0.0450834895714874,0.148875543265897,
2.00532944102159));
#20366=CARTESIAN_POINT('Ctrl Pts',(-0.0417466256309887,0.149867242375032,
2.00507849826894));
#20367=CARTESIAN_POINT('Ctrl Pts',(-0.0391610406471848,0.150563549137276,
2.00488335147288));
#20368=CARTESIAN_POINT('Ctrl Pts',(-0.0322603539253661,0.152232158534698,
2.00436026948027));
#20369=CARTESIAN_POINT('Ctrl Pts',(-0.0279198218369057,0.153087678703914,
2.00402888924305));
#20370=CARTESIAN_POINT('Ctrl Pts',(-0.0113209751961112,0.155629921774353,
2.00275348700118));
#20371=CARTESIAN_POINT('Ctrl Pts',(0.00108548628479758,0.156037230747702,
2.00177921278012));
#20372=CARTESIAN_POINT('Ctrl Pts',(0.0172812209132271,0.154635934541401,
2.00054174380077));
#20373=CARTESIAN_POINT('Ctrl Pts',(0.0211404622240561,0.15415576580977,
2.00024990730944));
#20374=CARTESIAN_POINT('Ctrl Pts',(0.0256017097638221,0.153429965195873,
1.99991897493799));
#20375=CARTESIAN_POINT('Ctrl Pts',(0.0262247728270713,0.15332469823797,
1.99987290410674));
#20376=CARTESIAN_POINT('Ctrl Pts',(0.0271667963785254,0.153159632273694,
1.99980348938374));
#20377=CARTESIAN_POINT('Ctrl Pts',(0.0274862293766622,0.153102628924415,
1.99977999338458));
#20378=CARTESIAN_POINT('Ctrl Pts',(0.0280590364333624,0.152998560073275,
1.99973793857796));
#20379=CARTESIAN_POINT('Ctrl Pts',(0.0283124726969926,0.152951864334157,
1.99971935928006));
#20380=CARTESIAN_POINT('Ctrl Pts',(0.0288624201043101,0.152849122539985,
1.99967910328604));
#20381=CARTESIAN_POINT('Ctrl Pts',(0.029158883754855,0.152792843608296,
1.99965744002884));
#20382=CARTESIAN_POINT('Ctrl Pts',(0.0299897630777745,0.152632607959033,
1.99959682703767));
#20383=CARTESIAN_POINT('Ctrl Pts',(0.0305238067040571,0.15252670634936,
1.999557985876));
#20384=CARTESIAN_POINT('Ctrl Pts',(0.0336816342138033,0.151883254942315,
1.9993289524563));
#20385=CARTESIAN_POINT('Ctrl Pts',(0.0362919410380928,0.151280775250069,
1.99914223320763));
#20386=CARTESIAN_POINT('Ctrl Pts',(0.0530689033031117,0.146949208971719,
1.99795129631909));
#20387=CARTESIAN_POINT('Ctrl Pts',(0.0666651674916582,0.141301942789719,
1.99702238066316));
#20388=CARTESIAN_POINT('Ctrl Pts',(0.0810038995866349,0.132808974960902,
1.99590253524051));
#20389=CARTESIAN_POINT('Ctrl Pts',(0.0827159391236219,0.131749491483096,
1.99576645296893));
#20390=CARTESIAN_POINT('Ctrl Pts',(0.0876815728064243,0.128541601264236,
1.99536390160295));
#20391=CARTESIAN_POINT('Ctrl Pts',(0.0908753095805218,0.126303900129376,
1.99509479698976));
#20392=CARTESIAN_POINT('Ctrl Pts',(0.0947335850372766,0.123378447797612,
1.99475481818793));
#20393=CARTESIAN_POINT('Ctrl Pts',(0.0954805306749854,0.122801309874749,
1.99468828033741));
#20394=CARTESIAN_POINT('Ctrl Pts',(0.0966467673505241,0.121883128041626,
1.9945832276294));
#20395=CARTESIAN_POINT('Ctrl Pts',(0.0970696220021085,0.121546628959793,
1.99454489314459));
#20396=CARTESIAN_POINT('Ctrl Pts',(0.0978131222422792,0.120948612296067,
1.99447705198347));
#20397=CARTESIAN_POINT('Ctrl Pts',(0.0981344958270651,0.120688004465343,
1.99444758197771));
#20398=CARTESIAN_POINT('Ctrl Pts',(0.0988685113443571,0.120087907344095,
1.99437993431787));
#20399=CARTESIAN_POINT('Ctrl Pts',(0.0992804493847016,0.119747569422287,
1.99434172259801));
#20400=CARTESIAN_POINT('Ctrl Pts',(0.100413889967894,0.118801266651526,
1.99423589202157));
#20401=CARTESIAN_POINT('Ctrl Pts',(0.101131642354956,0.118190867238116,
1.99416809294457));
#20402=CARTESIAN_POINT('Ctrl Pts',(0.105145081894065,0.114714385140549,
1.99378448509582));
#20403=CARTESIAN_POINT('Ctrl Pts',(0.108324132669722,0.1117172933804,1.99346326255191));
#20404=CARTESIAN_POINT('Ctrl Pts',(0.117981278881326,0.101812746566546,
1.99242911224421));
#20405=CARTESIAN_POINT('Ctrl Pts',(0.123956568369346,0.0944464983789309,
1.99169751173491));
#20406=CARTESIAN_POINT('Ctrl Pts',(0.130396529658678,0.0848350179764151,
1.9908002854657));
#20407=CARTESIAN_POINT('Ctrl Pts',(0.131532842463569,0.083062306311319,
1.99063706535839));
#20408=CARTESIAN_POINT('Ctrl Pts',(0.136315302920027,0.0752570374541442,
1.98992931818662));
#20409=CARTESIAN_POINT('Ctrl Pts',(0.139585554413716,0.0690027834368368,
1.98938964386267));
#20410=CARTESIAN_POINT('Ctrl Pts',(0.142703606915621,0.0619029767534948,
1.98882114286199));
#20411=CARTESIAN_POINT('Ctrl Pts',(0.142982273183565,0.0612565715941229,
1.98876977436984));
#20412=CARTESIAN_POINT('Ctrl Pts',(0.143386922127637,0.0603001245453035,
1.98869436582078));
#20413=CARTESIAN_POINT('Ctrl Pts',(0.143516302372836,0.0599915445405849,
1.98867012801401));
#20414=CARTESIAN_POINT('Ctrl Pts',(0.14374390815649,0.0594437401300686,
1.98862726482745));
#20415=CARTESIAN_POINT('Ctrl Pts',(0.143842533692127,0.059204686281806,
1.98860861554447));
#20416=CARTESIAN_POINT('Ctrl Pts',(0.144052317873465,0.0586925815079835,
1.98856878426623));
#20417=CARTESIAN_POINT('Ctrl Pts',(0.144163296323181,0.0584194608496645,
1.98854761319517));
#20418=CARTESIAN_POINT('Ctrl Pts',(0.144465163676944,0.0576704593376156,
1.98848974694982));
#20419=CARTESIAN_POINT('Ctrl Pts',(0.144654479533428,0.0571939416999642,
1.98845314503952));
#20420=CARTESIAN_POINT('Ctrl Pts',(0.145642557620112,0.0546706075163413,
1.98826040235285));
#20421=CARTESIAN_POINT('Ctrl Pts',(0.146400294784007,0.0526078410272297,
1.98810657625707));
#20422=CARTESIAN_POINT('Ctrl Pts',(0.151662877575025,0.0372861153084749,
1.98698641468158));
#20423=CARTESIAN_POINT('Ctrl Pts',(0.154403138817001,0.0234875087747944,
1.98609524939235));
#20424=CARTESIAN_POINT('Ctrl Pts',(0.155676291218612,0.00269541956444296,
1.98470463298604));
#20425=CARTESIAN_POINT('Ctrl Pts',(0.155644636198529,-0.0041352483516464,
1.9842411822829));
#20426=CARTESIAN_POINT('Ctrl Pts',(0.155094191013136,-0.011941530850703,
1.98369293930793));
#20427=CARTESIAN_POINT('Ctrl Pts',(0.155013979377042,-0.0129411884848262,
1.98362239085475));
#20428=CARTESIAN_POINT('Ctrl Pts',(0.154870105744432,-0.0145401501702901,
1.98350896883183));
#20429=CARTESIAN_POINT('Ctrl Pts',(0.154812616410037,-0.0151399934626027,
1.98346628839282));
#20430=CARTESIAN_POINT('Ctrl Pts',(0.154704534637707,-0.0162026608399094,
1.98339043820738));
#20431=CARTESIAN_POINT('Ctrl Pts',(0.154655346662608,-0.0166656231748197,
1.98335731288039));
#20432=CARTESIAN_POINT('Ctrl Pts',(0.154548731894783,-0.017627950266065,
1.98328828696969));
#20433=CARTESIAN_POINT('Ctrl Pts',(0.154490961571659,-0.018127270687945,
1.98325237596203));
#20434=CARTESIAN_POINT('Ctrl Pts',(0.154335129211849,-0.0194192779922778,
1.98315920236655));
#20435=CARTESIAN_POINT('Ctrl Pts',(0.154233381047045,-0.0202114965602983,
1.98310182453138));
#20436=CARTESIAN_POINT('Ctrl Pts',(0.153770262929164,-0.0236099980672875,
1.98285459344487));
#20437=CARTESIAN_POINT('Ctrl Pts',(0.153348915995802,-0.0262075210822798,
1.98266286686325));
#20438=CARTESIAN_POINT('Ctrl Pts',(0.152062956231254,-0.0330346839489465,
1.9821512342244));
#20439=CARTESIAN_POINT('Ctrl Pts',(0.151087858235822,-0.0372409160313285,
1.98182806772955));
#20440=CARTESIAN_POINT('Ctrl Pts',(0.1466408255629,-0.0533465025791879,
1.98056024066003));
#20441=CARTESIAN_POINT('Ctrl Pts',(0.141927179329378,-0.0648537737352712,
1.97958446705739));
#20442=CARTESIAN_POINT('Ctrl Pts',(0.135460343054487,-0.0764663958901571,
1.97857167519509));
#20443=CARTESIAN_POINT('Ctrl Pts',(0.135015159455912,-0.0772497315233394,
1.97850323477643));
#20444=CARTESIAN_POINT('Ctrl Pts',(0.132966853505567,-0.0807820845763594,
1.97819418700037));
#20445=CARTESIAN_POINT('Ctrl Pts',(0.131286263845199,-0.0834856274826196,
1.97795646698831));
#20446=CARTESIAN_POINT('Ctrl Pts',(0.129221591909066,-0.0865903022054238,
1.97768367850536));
#20447=CARTESIAN_POINT('Ctrl Pts',(0.128917034029391,-0.0870430848047933,
1.97764390083446));
#20448=CARTESIAN_POINT('Ctrl Pts',(0.128423592765812,-0.0877684069465211,
1.97758020084116));
#20449=CARTESIAN_POINT('Ctrl Pts',(0.128236213354629,-0.0880419560598212,
1.97755618170201));
#20450=CARTESIAN_POINT('Ctrl Pts',(0.127900975753297,-0.088528017718981,
1.97751351425601));
#20451=CARTESIAN_POINT('Ctrl Pts',(0.127753460378654,-0.088740762252881,
1.977494843191));
#20452=CARTESIAN_POINT('Ctrl Pts',(0.127437706578511,-0.0891937186337115,
1.97745509988986));
#20453=CARTESIAN_POINT('Ctrl Pts',(0.127269320148192,-0.0894338227663322,
1.97743403800241));
#20454=CARTESIAN_POINT('Ctrl Pts',(0.126808685480241,-0.0900867114633001,
1.97737677696216));
#20455=CARTESIAN_POINT('Ctrl Pts',(0.126515097934635,-0.0904985541826887,
1.97734066783917));
#20456=CARTESIAN_POINT('Ctrl Pts',(0.124989292510319,-0.0926170075093756,
1.97715494415612));
#20457=CARTESIAN_POINT('Ctrl Pts',(0.123724457173736,-0.0943000169714633,
1.97700744879639));
#20458=CARTESIAN_POINT('Ctrl Pts',(0.119883600746526,-0.0992003376135383,
1.9765764217289));
#20459=CARTESIAN_POINT('Ctrl Pts',(0.117213329133151,-0.10234171158765,
1.97629802048815));
#20460=CARTESIAN_POINT('Ctrl Pts',(0.107341338496447,-0.113061338500483,
1.97532531852297));
#20461=CARTESIAN_POINT('Ctrl Pts',(0.0995047140663776,-0.120016043834059,
1.97464976000939));
#20462=CARTESIAN_POINT('Ctrl Pts',(0.0858590321600602,-0.12986412210963,
1.97352352515621));
#20463=CARTESIAN_POINT('Ctrl Pts',(0.0804644437138974,-0.133273854104561,
1.97308940418812));
#20464=CARTESIAN_POINT('Ctrl Pts',(0.0740106587693025,-0.13681812882779,
1.97257345784011));
#20465=CARTESIAN_POINT('Ctrl Pts',(0.0731404578968763,-0.137285291733489,
1.97250396685572));
#20466=CARTESIAN_POINT('Ctrl Pts',(0.0717362247230707,-0.138022006649275,
1.97239192242702));
#20467=CARTESIAN_POINT('Ctrl Pts',(0.0712049731881711,-0.138296825821093,
1.97234955466334));
#20468=CARTESIAN_POINT('Ctrl Pts',(0.07026909053954,-0.138774140732129,
1.97227494746398));
#20469=CARTESIAN_POINT('Ctrl Pts',(0.0698651335014268,-0.138977949093029,
1.97224275442924));
#20470=CARTESIAN_POINT('Ctrl Pts',(0.0690212691370247,-0.139399094900101,
1.97217552066247));
#20471=CARTESIAN_POINT('Ctrl Pts',(0.0685812118368766,-0.139616118786712,
1.97214046944005));
#20472=CARTESIAN_POINT('Ctrl Pts',(0.0676825380167003,-0.140054045538962,
1.97206890499292));
#20473=CARTESIAN_POINT('Ctrl Pts',(0.0672238495825327,-0.140274786259309,
1.97203238664851));
#20474=CARTESIAN_POINT('Ctrl Pts',(0.0661008095077572,-0.140808468407406,
1.97194299272089));
#20475=CARTESIAN_POINT('Ctrl Pts',(0.0654353150787797,-0.141118961514586,
1.97189003345686));
#20476=CARTESIAN_POINT('Ctrl Pts',(0.063603008704174,-0.14195809477838,
1.97174424648088));
#20477=CARTESIAN_POINT('Ctrl Pts',(0.062431849225154,-0.142477041693043,
1.97165109157827));
#20478=CARTESIAN_POINT('Ctrl Pts',(0.0518180626325385,-0.147024076377469,
1.97080694902398));
#20479=CARTESIAN_POINT('Ctrl Pts',(0.042006506597302,-0.150121842374042,
1.9700246440002));
#20480=CARTESIAN_POINT('Ctrl Pts',(0.0215053315239889,-0.154426406878573,
1.9684030039209));
#20481=CARTESIAN_POINT('Ctrl Pts',(0.0108479864099955,-0.155538926101167,
1.96756713370226));
#20482=CARTESIAN_POINT('Ctrl Pts',(-0.000955858027842796,-0.155551065268592,
1.96669512941088));
#20483=CARTESIAN_POINT('Ctrl Pts',(-0.00207170853954404,-0.155540206336629,
1.96661324912423));
#20484=CARTESIAN_POINT('Ctrl Pts',(-0.00360320139091767,-0.155508817798688,
1.96650171335142));
#20485=CARTESIAN_POINT('Ctrl Pts',(-0.00401898546064192,-0.1554986277756,
1.96647151801203));
#20486=CARTESIAN_POINT('Ctrl Pts',(-0.00468073718734669,-0.155479753563257,
1.96642360107445));
#20487=CARTESIAN_POINT('Ctrl Pts',(-0.00492672961068839,-0.155472153154082,
1.96640582002003));
#20488=CARTESIAN_POINT('Ctrl Pts',(-0.00543559407843104,-0.155455221861582,
1.96636910349563));
#20489=CARTESIAN_POINT('Ctrl Pts',(-0.00569846076860234,-0.155445808026944,
1.9663501731504));
#20490=CARTESIAN_POINT('Ctrl Pts',(-0.0063259462810383,-0.155421742568673,
1.96630506949476));
#20491=CARTESIAN_POINT('Ctrl Pts',(-0.00669054305884584,-0.155406474447979,
1.96627893050278));
#20492=CARTESIAN_POINT('Ctrl Pts',(-0.00792530370060249,-0.155350413253704,
1.9661906277238));
#20493=CARTESIAN_POINT('Ctrl Pts',(-0.00879519914416804,-0.155303592688903,
1.96612878940414));
#20494=CARTESIAN_POINT('Ctrl Pts',(-0.0189396985458115,-0.154672071287271,
1.96541149714302));
#20495=CARTESIAN_POINT('Ctrl Pts',(-0.0281459778217095,-0.153264557204525,
1.96479752282471));
#20496=CARTESIAN_POINT('Ctrl Pts',(-0.0490372648985847,-0.148123062779557,
1.96338054238323));
#20497=CARTESIAN_POINT('Ctrl Pts',(-0.0605147332264084,-0.143815901292031,
1.96258099869321));
#20498=CARTESIAN_POINT('Ctrl Pts',(-0.0728982800061205,-0.137421263632336,
1.96161218079769));
#20499=CARTESIAN_POINT('Ctrl Pts',(-0.0744138140669874,-0.136606540071449,
1.96149175063737));
#20500=CARTESIAN_POINT('Ctrl Pts',(-0.0765273766854905,-0.135424719365902,
1.96132099965181));
#20501=CARTESIAN_POINT('Ctrl Pts',(-0.0771369531147193,-0.135078438075342,
1.96127142004941));
#20502=CARTESIAN_POINT('Ctrl Pts',(-0.0781196302719578,-0.13451138906466,
1.96119094344579));
#20503=CARTESIAN_POINT('Ctrl Pts',(-0.0784941907023739,-0.134293158578411,
1.96116013803356));
#20504=CARTESIAN_POINT('Ctrl Pts',(-0.0792650525500041,-0.133839703855469,
1.96109646609591));
#20505=CARTESIAN_POINT('Ctrl Pts',(-0.0796612301690202,-0.133604278686816,
1.96106359251929));
#20506=CARTESIAN_POINT('Ctrl Pts',(-0.0805902996664638,-0.133046585558012,
1.96098614423926));
#20507=CARTESIAN_POINT('Ctrl Pts',(-0.0811223105533769,-0.13272287307985,
1.96094151719078));
#20508=CARTESIAN_POINT('Ctrl Pts',(-0.0822430216212552,-0.132031698771067,
1.96084691083047));
#20509=CARTESIAN_POINT('Ctrl Pts',(-0.0828312336650479,-0.131663475520993,
1.96079690418931));
#20510=CARTESIAN_POINT('Ctrl Pts',(-0.0844136829933907,-0.130658054236761,
1.960661407425));
#20511=CARTESIAN_POINT('Ctrl Pts',(-0.085403142529092,-0.13001346129073,
1.96057564577962));
#20512=CARTESIAN_POINT('Ctrl Pts',(-0.0935766449473686,-0.12455519115846,
1.95985836514297));
#20513=CARTESIAN_POINT('Ctrl Pts',(-0.100353851602388,-0.119162243733623,
1.95920492475817));
#20514=CARTESIAN_POINT('Ctrl Pts',(-0.113253623320465,-0.107013002611593,
1.95783995513486));
#20515=CARTESIAN_POINT('Ctrl Pts',(-0.119302950469435,-0.100224613700158,
1.9571297266313));
#20516=CARTESIAN_POINT('Ctrl Pts',(-0.127193279130592,-0.0896366120549464,
1.95612278647015));
#20517=CARTESIAN_POINT('Ctrl Pts',(-0.129528093174465,-0.086228377536606,
1.95581227193964));
#20518=CARTESIAN_POINT('Ctrl Pts',(-0.132065883290486,-0.0821876903225205,
1.95546284378582));
#20519=CARTESIAN_POINT('Ctrl Pts',(-0.132403694690286,-0.0816423642520919,
1.95541606687148));
#20520=CARTESIAN_POINT('Ctrl Pts',(-0.132908365124097,-0.0808163077729507,
1.95534580096908));
#20521=CARTESIAN_POINT('Ctrl Pts',(-0.133077723808474,-0.0805371253105897,
1.95532215436101));
#20522=CARTESIAN_POINT('Ctrl Pts',(-0.133379244285927,-0.0800365302871452,
1.95527993779332));
#20523=CARTESIAN_POINT('Ctrl Pts',(-0.133511735243091,-0.0798153214779604,
1.95526134664775));
#20524=CARTESIAN_POINT('Ctrl Pts',(-0.133797301256218,-0.079335835604815,
1.95522118769646));
#20525=CARTESIAN_POINT('Ctrl Pts',(-0.133950178411043,-0.0790774452190182,
1.95519963278577));
#20526=CARTESIAN_POINT('Ctrl Pts',(-0.134374618096505,-0.078355301794799,
1.95513962743399));
#20527=CARTESIAN_POINT('Ctrl Pts',(-0.134644530442156,-0.07789057550641,
1.95510128208874));
#20528=CARTESIAN_POINT('Ctrl Pts',(-0.136187198456087,-0.0752024779054694,
1.95488098073415));
#20529=CARTESIAN_POINT('Ctrl Pts',(-0.137407375798178,-0.0729491661319911,
1.95470219627397));
#20530=CARTESIAN_POINT('Ctrl Pts',(-0.145268243243652,-0.0575346408648738,
1.95351124157567));
#20531=CARTESIAN_POINT('Ctrl Pts',(-0.150065138145776,-0.043516229409762,
1.95257692528643));
#20532=CARTESIAN_POINT('Ctrl Pts',(-0.153601606067318,-0.0249002894026177,
1.95130390485614));
#20533=CARTESIAN_POINT('Ctrl Pts',(-0.154218412415422,-0.0207401610576978,
1.95101799420024));
#20534=CARTESIAN_POINT('Ctrl Pts',(-0.15489124737387,-0.0144562234771152,
1.95058054668062));
#20535=CARTESIAN_POINT('Ctrl Pts',(-0.155073574330454,-0.0123477406578274,
1.95043284499954));
#20536=CARTESIAN_POINT('Ctrl Pts',(-0.155262955910089,-0.00947614583061637,
1.95023014598214));
#20537=CARTESIAN_POINT('Ctrl Pts',(-0.155307501279662,-0.00871566560299412,
1.95017631942679));
#20538=CARTESIAN_POINT('Ctrl Pts',(-0.155369221036843,-0.00751037771224534,
1.95009076532835));
#20539=CARTESIAN_POINT('Ctrl Pts',(-0.155390075623419,-0.00706576317293903,
1.95005915298214));
#20540=CARTESIAN_POINT('Ctrl Pts',(-0.155428039236629,-0.00617468537339508,
1.94999568854372));
#20541=CARTESIAN_POINT('Ctrl Pts',(-0.155445133542863,-0.00572822578035388,
1.94996383630101));
#20542=CARTESIAN_POINT('Ctrl Pts',(-0.155475548762664,-0.00483299192687254,
1.94989985476956));
#20543=CARTESIAN_POINT('Ctrl Pts',(-0.155488850626594,-0.00438422137019486,
1.94986772519707));
#20544=CARTESIAN_POINT('Ctrl Pts',(-0.155516523312597,-0.00329078632529114,
1.94978930068499));
#20545=CARTESIAN_POINT('Ctrl Pts',(-0.155528828583525,-0.00264608277559738,
1.94974294167468));
#20546=CARTESIAN_POINT('Ctrl Pts',(-0.155545899167395,-0.00131941042582578,
1.94964729242611));
#20547=CARTESIAN_POINT('Ctrl Pts',(-0.155550188730665,-0.000637452225819819,
1.94959798844521));
#20548=CARTESIAN_POINT('Ctrl Pts',(-0.155549993634555,4.4500446807104E-5,
1.94954854470546));
#20549=CARTESIAN_POINT('Ctrl Pts',(-0.155549993659165,4.44143407372304E-5,
1.94954855094842));
#20550=CARTESIAN_POINT('Ctrl Pts',(-0.155548101258003,0.00667207072290408,
1.94906802487631));
#20551=CARTESIAN_POINT('Ctrl Pts',(-0.155122636147792,0.0132920259975428,
1.94857436416224));
#20552=CARTESIAN_POINT('Ctrl Pts',(-0.152482240194681,0.0337989542877253,
1.94700207819705));
#20553=CARTESIAN_POINT('Ctrl Pts',(-0.148808679883158,0.04742510843954,
1.94588882031672));
#20554=CARTESIAN_POINT('Ctrl Pts',(-0.142496832313422,0.0624127955721348,
1.94467037371801));
#20555=CARTESIAN_POINT('Ctrl Pts',(-0.141594005450325,0.064434798587637,
1.94450631040506));
#20556=CARTESIAN_POINT('Ctrl Pts',(-0.140428729685775,0.0669017081128451,
1.94430712885515));
#20557=CARTESIAN_POINT('Ctrl Pts',(-0.140206899836237,0.0673653614850748,
1.94426973631914));
#20558=CARTESIAN_POINT('Ctrl Pts',(-0.139854102774855,0.0680934615613401,
1.94421109503832));
#20559=CARTESIAN_POINT('Ctrl Pts',(-0.139724677045046,0.0683586439229629,
1.94418975363807));
#20560=CARTESIAN_POINT('Ctrl Pts',(-0.139480430694265,0.068855492180789,
1.94414980124356));
#20561=CARTESIAN_POINT('Ctrl Pts',(-0.139365788459261,0.0690872373071932,
1.94413118005838));
#20562=CARTESIAN_POINT('Ctrl Pts',(-0.139101652413358,0.069617845835817,
1.94408857496985));
#20563=CARTESIAN_POINT('Ctrl Pts',(-0.138951773153954,0.0699165138289534,
1.94406461541404));
#20564=CARTESIAN_POINT('Ctrl Pts',(-0.138556092845935,0.0706986975422221,
1.94400191900117));
#20565=CARTESIAN_POINT('Ctrl Pts',(-0.138308720321889,0.0711814203634465,
1.94396327780331));
#20566=CARTESIAN_POINT('Ctrl Pts',(-0.136622386882318,0.0744301498470395,
1.9437035044587));
#20567=CARTESIAN_POINT('Ctrl Pts',(-0.135102939975808,0.0771538913108513,
1.94348709331092));
#20568=CARTESIAN_POINT('Ctrl Pts',(-0.132994460943277,0.0806799590927155,
1.94320628877225));
#20569=CARTESIAN_POINT('Ctrl Pts',(-0.132478311159367,0.0815247177059097,
1.94313896498887));
#20570=CARTESIAN_POINT('Ctrl Pts',(-0.125401180664853,0.0928628115699695,
1.94223388428348));
#20571=CARTESIAN_POINT('Ctrl Pts',(-0.117618537093517,0.102542095411774,
1.94144055988637));
#20572=CARTESIAN_POINT('Ctrl Pts',(-0.105686486376321,0.114213745264046,
1.94032367419196));
#20573=CARTESIAN_POINT('Ctrl Pts',(-0.102478641422242,0.117100538816519,
1.94003167995245));
#20574=CARTESIAN_POINT('Ctrl Pts',(-0.0978121326962387,0.120961264864625,
1.93961440727012));
#20575=CARTESIAN_POINT('Ctrl Pts',(-0.0964505514090239,0.12204970964807,
1.9394935083316));
#20576=CARTESIAN_POINT('Ctrl Pts',(-0.0943479378588876,0.123673375188351,
1.93930789324801));
#20577=CARTESIAN_POINT('Ctrl Pts',(-0.0936199731629827,0.124225350357299,
1.93924382275595));
#20578=CARTESIAN_POINT('Ctrl Pts',(-0.092419108691455,0.125119348610096,
1.93913841884149));
#20579=CARTESIAN_POINT('Ctrl Pts',(-0.0919490639791205,0.125465185070119,
1.93909723271501));
#20580=CARTESIAN_POINT('Ctrl Pts',(-0.0910373313247781,0.126128119133708,
1.9390174750252));
#20581=CARTESIAN_POINT('Ctrl Pts',(-0.0905959042477838,0.126445562400733,
1.93897891745529));
#20582=CARTESIAN_POINT('Ctrl Pts',(-0.0901487438348547,0.126763585110641,
1.93893991474853));
#20583=CARTESIAN_POINT('Ctrl Pts',(-0.0901446605611322,0.126766488858149,
1.9389395585975));
#20584=CARTESIAN_POINT('Ctrl Pts',(-0.0901364395265637,0.126772334502643,
1.93893884155237));
#20585=CARTESIAN_POINT('Ctrl Pts',(-0.0901323017632664,0.126775276393433,
1.93893848065817));
#20586=CARTESIAN_POINT('Ctrl Pts',(-0.0901239694976532,0.126781199901523,
1.93893775393067));
#20587=CARTESIAN_POINT('Ctrl Pts',(-0.0901197749909123,0.126784181513591,
1.9389373880971));
#20588=CARTESIAN_POINT('Ctrl Pts',(-0.0901113268814691,0.126790186114276,
1.93893665128568));
#20589=CARTESIAN_POINT('Ctrl Pts',(-0.0901070732741274,0.126793209097343,
1.93893628030756));
#20590=CARTESIAN_POINT('Ctrl Pts',(-0.0900985044965344,0.126799298166471,
1.93893553299229));
#20591=CARTESIAN_POINT('Ctrl Pts',(-0.0900941893217961,0.126802364246373,
1.9389351566549));
#20592=CARTESIAN_POINT('Ctrl Pts',(-0.0900854948267593,0.126808541315933,
1.93893439839629));
#20593=CARTESIAN_POINT('Ctrl Pts',(-0.090081115501624,0.126811652299147,
1.9389340164748));
#20594=CARTESIAN_POINT('Ctrl Pts',(-0.0900722899994163,0.126817921067967,
1.93893324681243));
#20595=CARTESIAN_POINT('Ctrl Pts',(-0.0900678438172105,0.12682107884677,
1.93893285907127));
#20596=CARTESIAN_POINT('Ctrl Pts',(-0.0900603829372504,0.126826377141611,
1.93893220843461));
#20597=CARTESIAN_POINT('Ctrl Pts',(-0.0900573683296655,0.12682851778368,
1.938931945544));
#20598=CARTESIAN_POINT('Ctrl Pts',(-0.0900511162572359,0.126832956981182,
1.93893140033362));
#20599=CARTESIAN_POINT('Ctrl Pts',(-0.0900478787803757,0.126835255520377,
1.9389311180132));
#20600=CARTESIAN_POINT('Ctrl Pts',(-0.0900411605587199,0.126840024926912,
1.93893053216451));
#20601=CARTESIAN_POINT('Ctrl Pts',(-0.090037679800594,0.126842495774667,
1.93893022863553));
#20602=CARTESIAN_POINT('Ctrl Pts',(-0.0900304521547473,0.126847625937275,
1.93892959837756));
#20603=CARTESIAN_POINT('Ctrl Pts',(-0.0900267052510161,0.126850285229312,
1.93892927164769));
#20604=CARTESIAN_POINT('Ctrl Pts',(-0.0900189196155608,0.126855810413918,
1.93892859274869));
#20605=CARTESIAN_POINT('Ctrl Pts',(-0.0900148808639589,0.126858676280229,
1.93892824057845));
#20606=CARTESIAN_POINT('Ctrl Pts',(-0.0900064825288195,0.126864635069674,
1.93892750827155));
#20607=CARTESIAN_POINT('Ctrl Pts',(-0.0900021229232172,0.126867727960606,
1.93892712813372));
#20608=CARTESIAN_POINT('Ctrl Pts',(-0.0899930500161233,0.126874163966456,
1.93892633702837));
#20609=CARTESIAN_POINT('Ctrl Pts',(-0.0899883366882774,0.126877507043088,
1.93892592605944));
#20610=CARTESIAN_POINT('Ctrl Pts',(-0.0899785189308473,0.126884469775336,
1.9389250700331));
#20611=CARTESIAN_POINT('Ctrl Pts',(-0.0899734144694325,0.126888089385367,
1.93892462497399));
#20612=CARTESIAN_POINT('Ctrl Pts',(-0.0899627716653422,0.126895635308622,
1.93892369704063));
#20613=CARTESIAN_POINT('Ctrl Pts',(-0.0899572332835722,0.12689956156762,
1.93892321416424));
#20614=CARTESIAN_POINT('Ctrl Pts',(-0.0899456733374862,0.126907755485385,
1.93892220630185));
#20615=CARTESIAN_POINT('Ctrl Pts',(-0.0899396517265052,0.126912023078093,
1.93892168131331));
#20616=CARTESIAN_POINT('Ctrl Pts',(-0.0899270690720986,0.126920939221072,
1.93892058432729));
#20617=CARTESIAN_POINT('Ctrl Pts',(-0.0899205076215407,0.126925587939331,
1.9389200122962));
#20618=CARTESIAN_POINT('Ctrl Pts',(-0.0899067785459363,0.126935313245102,
1.93891881541226));
#20619=CARTESIAN_POINT('Ctrl Pts',(-0.0898996109391876,0.126940389672184,
1.93891819056332));
#20620=CARTESIAN_POINT('Ctrl Pts',(-0.0898845921144436,0.126951024781039,
1.93891688130013));
#20621=CARTESIAN_POINT('Ctrl Pts',(-0.0898767408832245,0.126956583290319,
1.93891619688757));
#20622=CARTESIAN_POINT('Ctrl Pts',(-0.0895000149489004,0.127223244996466,
1.93888335750843));
#20623=CARTESIAN_POINT('Ctrl Pts',(-0.0891300083491297,0.127482737447264,
1.93885114137481));
#20624=CARTESIAN_POINT('Ctrl Pts',(-0.0882758946293854,0.128076207105572,
1.93877685726191));
#20625=CARTESIAN_POINT('Ctrl Pts',(-0.0877910163221103,0.128409056669391,
1.93873474707374));
#20626=CARTESIAN_POINT('Ctrl Pts',(-0.0863635310489605,0.129377103783548,
1.93861094337733));
#20627=CARTESIAN_POINT('Ctrl Pts',(-0.0854158534726185,0.130004716555484,
1.93852896683716));
#20628=CARTESIAN_POINT('Ctrl Pts',(-0.0778307606187714,0.134909313282266,
1.93787439070659));
#20629=CARTESIAN_POINT('Ctrl Pts',(-0.0708862440772289,0.138683750813039,
1.93728355898094));
#20630=CARTESIAN_POINT('Ctrl Pts',(-0.0636886188644129,0.141913925768909,
1.93667989110148));
#20631=CARTESIAN_POINT('',(-0.155681301642334,0.000117756784957245,1.93559437743963));
#20632=CARTESIAN_POINT('Ctrl Pts',(-0.0637929161402304,0.142146585575849,
1.92279372449516));
#20633=CARTESIAN_POINT('Ctrl Pts',(-0.0640110746858145,0.142048797739288,
1.92281092584587));
#20634=CARTESIAN_POINT('Ctrl Pts',(-0.111163659106404,0.120769939794772,
1.9265330314905));
#20635=CARTESIAN_POINT('Ctrl Pts',(-0.151792203072743,0.0668263219655577,
1.93079991580532));
#20636=CARTESIAN_POINT('Ctrl Pts',(-0.155745145114401,0.00770521701255957,
1.93504959876944));
#20637=CARTESIAN_POINT('Ctrl Pts',(-0.155681301642334,0.000117756784957245,
1.93559437743963));
#20638=CARTESIAN_POINT('Ctrl Pts',(-0.155549951651874,0.000122642161511279,
1.93566981437342));
#20639=CARTESIAN_POINT('Ctrl Pts',(-0.155560736539099,-0.0135560851688855,
1.93658042514193));
#20640=CARTESIAN_POINT('Ctrl Pts',(-0.153767332752135,-0.027176334668751,
1.93745914173611));
#20641=CARTESIAN_POINT('Ctrl Pts',(-0.149678189266885,-0.0423854174351624,
1.93853915783634));
#20642=CARTESIAN_POINT('Ctrl Pts',(-0.149101152578633,-0.0443726220478013,
1.93868214852758));
#20643=CARTESIAN_POINT('Ctrl Pts',(-0.148034862048453,-0.0477887131809654,
1.93893161318147));
#20644=CARTESIAN_POINT('Ctrl Pts',(-0.147564112081982,-0.0492231046750981,
1.93903749322602));
#20645=CARTESIAN_POINT('Ctrl Pts',(-0.14686248590787,-0.051260403880581,
1.93918960192921));
#20646=CARTESIAN_POINT('Ctrl Pts',(-0.146648607158145,-0.0518691118966943,
1.93923527091572));
#20647=CARTESIAN_POINT('Ctrl Pts',(-0.146272139818397,-0.0529196108580932,
1.93931447824197));
#20648=CARTESIAN_POINT('Ctrl Pts',(-0.14611131986409,-0.0533620305000578,
1.93934795762436));
#20649=CARTESIAN_POINT('Ctrl Pts',(-0.145798875265619,-0.0542095709404938,
1.93941232979911));
#20650=CARTESIAN_POINT('Ctrl Pts',(-0.145647563888115,-0.0546148032749892,
1.93944321189659));
#20651=CARTESIAN_POINT('Ctrl Pts',(-0.145248203127353,-0.0556708821345272,
1.9395239689754));
#20652=CARTESIAN_POINT('Ctrl Pts',(-0.144997471423163,-0.0563206967374926,
1.93957393317563));
#20653=CARTESIAN_POINT('Ctrl Pts',(-0.144119881127544,-0.0585504176402177,
1.9397463356803));
#20654=CARTESIAN_POINT('Ctrl Pts',(-0.143471516458125,-0.0601216689818702,
1.93986949203347));
#20655=CARTESIAN_POINT('Ctrl Pts',(-0.13778994016593,-0.0732748776776057,
1.94091500987123));
#20656=CARTESIAN_POINT('Ctrl Pts',(-0.131390254839332,-0.0842124674285625,
1.94188623597532));
#20657=CARTESIAN_POINT('Ctrl Pts',(-0.120123636345364,-0.0990038605818356,
1.94332818916026));
#20658=CARTESIAN_POINT('Ctrl Pts',(-0.116235013735456,-0.103541694654355,
1.9437907613586));
#20659=CARTESIAN_POINT('Ctrl Pts',(-0.110523633345129,-0.109478149551362,
1.94441507031621));
#20660=CARTESIAN_POINT('Ctrl Pts',(-0.108916751362631,-0.111076916040401,
1.94458528672098));
#20661=CARTESIAN_POINT('Ctrl Pts',(-0.106277395288187,-0.113590568266269,
1.94485554400103));
#20662=CARTESIAN_POINT('Ctrl Pts',(-0.105266745636878,-0.114527789496645,
1.94495692894366));
#20663=CARTESIAN_POINT('Ctrl Pts',(-0.10391954959005,-0.115744202793354,
1.94508918933754));
#20664=CARTESIAN_POINT('Ctrl Pts',(-0.103594136406815,-0.11603554706154,
1.94512091922421));
#20665=CARTESIAN_POINT('Ctrl Pts',(-0.103086545641807,-0.116486158639652,
1.94517007012003));
#20666=CARTESIAN_POINT('Ctrl Pts',(-0.102905219930328,-0.116646374826935,
1.94518756082316));
#20667=CARTESIAN_POINT('Ctrl Pts',(-0.102528959477556,-0.116977271716535,
1.94522371436903));
#20668=CARTESIAN_POINT('Ctrl Pts',(-0.102333974904538,-0.117147886072938,
1.94524237179416));
#20669=CARTESIAN_POINT('Ctrl Pts',(-0.101886782017343,-0.117537217900752,
1.94528498574661));
#20670=CARTESIAN_POINT('Ctrl Pts',(-0.101634295378522,-0.117755611120077,
1.94530891820904));
#20671=CARTESIAN_POINT('Ctrl Pts',(-0.100961303073109,-0.118333951857486,
1.94537237735447));
#20672=CARTESIAN_POINT('Ctrl Pts',(-0.100539570695256,-0.118692475032757,
1.94541180197351));
#20673=CARTESIAN_POINT('Ctrl Pts',(-0.0975562448091676,-0.121201350091304,
1.94568836694548));
#20674=CARTESIAN_POINT('Ctrl Pts',(-0.0949275562336637,-0.123271048982066,
1.94592006649189));
#20675=CARTESIAN_POINT('Ctrl Pts',(-0.0817561470005722,-0.132970103526315,
1.94703534216842));
#20676=CARTESIAN_POINT('Ctrl Pts',(-0.070350950316552,-0.139341033582169,
1.94786705265347));
#20677=CARTESIAN_POINT('Ctrl Pts',(-0.0542188616325873,-0.145860713403675,
1.94903065356432));
#20678=CARTESIAN_POINT('Ctrl Pts',(-0.0500857603310041,-0.147331070074396,
1.94932729914623));
#20679=CARTESIAN_POINT('Ctrl Pts',(-0.0433536771466576,-0.149409982102765,
1.94981258546593));
#20680=CARTESIAN_POINT('Ctrl Pts',(-0.0407914414924076,-0.150129746886196,
1.9499977434002));
#20681=CARTESIAN_POINT('Ctrl Pts',(-0.0374348984835355,-0.150980375436686,
1.95024146484683));
#20682=CARTESIAN_POINT('Ctrl Pts',(-0.0366561654422768,-0.151171329567979,
1.95029808901912));
#20683=CARTESIAN_POINT('Ctrl Pts',(-0.0353863436199081,-0.151472315699011,
1.95039056688825));
#20684=CARTESIAN_POINT('Ctrl Pts',(-0.0348961284046633,-0.151586001825782,
1.95042630302709));
#20685=CARTESIAN_POINT('Ctrl Pts',(-0.0339517266349029,-0.151800194801551,
1.9504952202802));
#20686=CARTESIAN_POINT('Ctrl Pts',(-0.0334976232380456,-0.151901047106464,
1.95052838992999));
#20687=CARTESIAN_POINT('Ctrl Pts',(-0.0324560232737575,-0.152127479352476,
1.95060454890341));
#20688=CARTESIAN_POINT('Ctrl Pts',(-0.0318682410799109,-0.152251694941682,
1.95064758127769));
#20689=CARTESIAN_POINT('Ctrl Pts',(-0.0303031505197865,-0.152572984277758,
1.9507623187657));
#20690=CARTESIAN_POINT('Ctrl Pts',(-0.0293246562348661,-0.152764069445282,
1.95083421305952));
#20691=CARTESIAN_POINT('Ctrl Pts',(-0.0218612065856581,-0.154147220851159,
1.95138389247779));
#20692=CARTESIAN_POINT('Ctrl Pts',(-0.0153091534947095,-0.154935097947975,
1.95187438267373));
#20693=CARTESIAN_POINT('Ctrl Pts',(0.00264210595473488,-0.155943908639876,
1.95324023937947));
#20694=CARTESIAN_POINT('Ctrl Pts',(0.0140474868714411,-0.155332272976203,
1.95413432988196));
#20695=CARTESIAN_POINT('Ctrl Pts',(0.0285342290034816,-0.152945947004194,
1.95525864861734));
#20696=CARTESIAN_POINT('Ctrl Pts',(0.0317686288650324,-0.152307000450994,
1.95550865138042));
#20697=CARTESIAN_POINT('Ctrl Pts',(0.0361528408756284,-0.151295149191254,
1.95584416164348));
#20698=CARTESIAN_POINT('Ctrl Pts',(0.0373220407423635,-0.151010978301856,
1.95593330400824));
#20699=CARTESIAN_POINT('Ctrl Pts',(0.0390602217786782,-0.150567096423929,
1.95606521545951));
#20700=CARTESIAN_POINT('Ctrl Pts',(0.0396317490393489,-0.150417671661262,
1.95610848980886));
#20701=CARTESIAN_POINT('Ctrl Pts',(0.0406637968119638,-0.150141553979984,
1.95618643712328));
#20702=CARTESIAN_POINT('Ctrl Pts',(0.0411246079561466,-0.150015989945517,
1.95622116968572));
#20703=CARTESIAN_POINT('Ctrl Pts',(0.0418471583835612,-0.149815526370937,
1.95627551078566));
#20704=CARTESIAN_POINT('Ctrl Pts',(0.0421092864472314,-0.149742060238919,
1.95629519999308));
#20705=CARTESIAN_POINT('Ctrl Pts',(0.0426192405377143,-0.149597691421681,
1.95633345412609));
#20706=CARTESIAN_POINT('Ctrl Pts',(0.0428670804370714,-0.149526861664821,
1.95635202248165));
#20707=CARTESIAN_POINT('Ctrl Pts',(0.0434283408213854,-0.149364949827743,
1.95639402068006));
#20708=CARTESIAN_POINT('Ctrl Pts',(0.0437416508320479,-0.149273497350764,
1.95641742871764));
#20709=CARTESIAN_POINT('Ctrl Pts',(0.0446900127946774,-0.148993436476291,
1.9564881789221));
#20710=CARTESIAN_POINT('Ctrl Pts',(0.0453241611516411,-0.148801753398515,
1.95653534662211));
#20711=CARTESIAN_POINT('Ctrl Pts',(0.0502554040324811,-0.147276744341285,
1.95690116946907));
#20712=CARTESIAN_POINT('Ctrl Pts',(0.0544945527977949,-0.145761443306784,
1.95720996619881));
#20713=CARTESIAN_POINT('Ctrl Pts',(0.0724785450229919,-0.13843842106018,
1.95851950745904));
#20714=CARTESIAN_POINT('Ctrl Pts',(0.0854134863931019,-0.130854572180079,
1.95946785406036));
#20715=CARTESIAN_POINT('Ctrl Pts',(0.0999867259902557,-0.119215689626974,
1.96074032589194));
#20716=CARTESIAN_POINT('Ctrl Pts',(0.102817442610874,-0.116783113634066,
1.96099830622388));
#20717=CARTESIAN_POINT('Ctrl Pts',(0.10621759508231,-0.113641682313828,
1.96132362886396));
#20718=CARTESIAN_POINT('Ctrl Pts',(0.106872098250807,-0.113026386384555,
1.96138699407023));
#20719=CARTESIAN_POINT('Ctrl Pts',(0.107900315546164,-0.112042847203186,
1.96148774838475));
#20720=CARTESIAN_POINT('Ctrl Pts',(0.108277566805066,-0.111678315795256,
1.96152497726155));
#20721=CARTESIAN_POINT('Ctrl Pts',(0.108982608753773,-0.110990115293288,
1.9615950535961));
#20722=CARTESIAN_POINT('Ctrl Pts',(0.10931082052639,-0.110666883985498,
1.96162788171888));
#20723=CARTESIAN_POINT('Ctrl Pts',(0.110043680296804,-0.109938704051317,
1.96170165090116));
#20724=CARTESIAN_POINT('Ctrl Pts',(0.11044753645901,-0.109532971728526,
1.96174262630041));
#20725=CARTESIAN_POINT('Ctrl Pts',(0.111467986905762,-0.108496398734033,
1.96184699482639));
#20726=CARTESIAN_POINT('Ctrl Pts',(0.11208146429014,-0.107862532633251,
1.96191052251609));
#20727=CARTESIAN_POINT('Ctrl Pts',(0.115602048949649,-0.104162476548154,
1.9622797125985));
#20728=CARTESIAN_POINT('Ctrl Pts',(0.118388376396759,-0.100984361141317,
1.96259045386355));
#20729=CARTESIAN_POINT('Ctrl Pts',(0.122266767131115,-0.0961792326710502,
1.9630518419119));
#20730=CARTESIAN_POINT('Ctrl Pts',(0.123463153748043,-0.0946385558650066,
1.9631985754465));
#20731=CARTESIAN_POINT('Ctrl Pts',(0.133411101221104,-0.0813180772806547,
1.96445686522506));
#20732=CARTESIAN_POINT('Ctrl Pts',(0.140482878825809,-0.0683786857792587,
1.965621005447));
#20733=CARTESIAN_POINT('Ctrl Pts',(0.146473468126477,-0.0524117917164091,
1.96690107004666));
#20734=CARTESIAN_POINT('Ctrl Pts',(0.14725870156279,-0.0501632263856047,
1.96707776412079));
#20735=CARTESIAN_POINT('Ctrl Pts',(0.148153895696174,-0.0473972780055289,
1.96729006915772));
#20736=CARTESIAN_POINT('Ctrl Pts',(0.148313212175785,-0.0468963739310325,
1.96732831695149));
#20737=CARTESIAN_POINT('Ctrl Pts',(0.148558747110719,-0.0461106247203761,
1.96738799185357));
#20738=CARTESIAN_POINT('Ctrl Pts',(0.148646690361068,-0.0458263298112838,
1.96740951706766));
#20739=CARTESIAN_POINT('Ctrl Pts',(0.148809376701129,-0.0452950163672011,
1.9674496197778));
#20740=CARTESIAN_POINT('Ctrl Pts',(0.148884320082321,-0.0450480669636376,
1.96746820841262));
#20741=CARTESIAN_POINT('Ctrl Pts',(0.149053707856101,-0.0444848693626846,
1.96751048770032));
#20742=CARTESIAN_POINT('Ctrl Pts',(0.149147760425931,-0.0441685068037201,
1.96753415534039));
#20743=CARTESIAN_POINT('Ctrl Pts',(0.149432761146161,-0.0431985649693213,
1.96760647523785));
#20744=CARTESIAN_POINT('Ctrl Pts',(0.149620428951448,-0.0425440172648214,
1.96765494146853));
#20745=CARTESIAN_POINT('Ctrl Pts',(0.152302537149554,-0.0329520656819254,
1.96836054361617));
#20746=CARTESIAN_POINT('Ctrl Pts',(0.153997129445366,-0.0238085451989766,
1.96897494828362));
#20747=CARTESIAN_POINT('Ctrl Pts',(0.155746566149695,-0.00520983802281561,
1.97020584323075));
#20748=CARTESIAN_POINT('Ctrl Pts',(0.155776822276914,0.00420721082647058,
1.97082027010685));
#20749=CARTESIAN_POINT('Ctrl Pts',(0.154577538798896,0.0179028727148061,
1.97175363156202));
#20750=CARTESIAN_POINT('Ctrl Pts',(0.15401643567276,0.0222184585224185,
1.97205335550352));
#20751=CARTESIAN_POINT('Ctrl Pts',(0.153114953172941,0.0274317145151927,
1.97242491744402));
#20752=CARTESIAN_POINT('Ctrl Pts',(0.152946219868382,0.0283573906583666,
1.97249125687299));
#20753=CARTESIAN_POINT('Ctrl Pts',(0.152668586831669,0.0298058754014483,
1.97259566049395));
#20754=CARTESIAN_POINT('Ctrl Pts',(0.152565373205549,0.0303297625996239,
1.97263354389921));
#20755=CARTESIAN_POINT('Ctrl Pts',(0.152377424019499,0.0312585065662062,
1.97270092603383));
#20756=CARTESIAN_POINT('Ctrl Pts',(0.152293766683983,0.0316635785518406,
1.97273039014181));
#20757=CARTESIAN_POINT('Ctrl Pts',(0.152097075569938,0.0325971500418707,
1.97279847277301));
#20758=CARTESIAN_POINT('Ctrl Pts',(0.151982901599042,0.0331254010646873,
1.97283712736884));
#20759=CARTESIAN_POINT('Ctrl Pts',(0.151661618571396,0.0345752540631672,
1.97294358591539));
#20760=CARTESIAN_POINT('Ctrl Pts',(0.151448867041889,0.0354955678896996,
1.97301156944475));
#20761=CARTESIAN_POINT('Ctrl Pts',(0.150312665755701,0.0402142416495102,
1.97336228895718));
#20762=CARTESIAN_POINT('Ctrl Pts',(0.149254734739986,0.0439784242627081,
1.97364930384012));
#20763=CARTESIAN_POINT('Ctrl Pts',(0.14744170478517,0.0496060762246703,
1.97408994132385));
#20764=CARTESIAN_POINT('Ctrl Pts',(0.146790359846765,0.0515015412662265,
1.97424037166348));
#20765=CARTESIAN_POINT('Ctrl Pts',(0.141079630016337,0.0671308543243121,
1.97549741846902));
#20766=CARTESIAN_POINT('Ctrl Pts',(0.134142594246796,0.0800980642564889,
1.97665763748276));
#20767=CARTESIAN_POINT('Ctrl Pts',(0.123907165038909,0.094074733064713,
1.97796213274712));
#20768=CARTESIAN_POINT('Ctrl Pts',(0.122261383105815,0.0962039371820799,
1.97816225282094));
#20769=CARTESIAN_POINT('Ctrl Pts',(0.120216671396456,0.0987119621131707,
1.97839867162313));
#20770=CARTESIAN_POINT('Ctrl Pts',(0.119870057847602,0.099132581936461,
1.97843834526732));
#20771=CARTESIAN_POINT('Ctrl Pts',(0.119328068000838,0.0997832941153622,
1.97849974763129));
#20772=CARTESIAN_POINT('Ctrl Pts',(0.119134225432632,0.10001464858772,1.97852158380102));
#20773=CARTESIAN_POINT('Ctrl Pts',(0.118773693421933,0.100442414401462,
1.97856196530536));
#20774=CARTESIAN_POINT('Ctrl Pts',(0.118607191035839,0.100638974042889,
1.9785805233094));
#20775=CARTESIAN_POINT('Ctrl Pts',(0.118230071907623,0.101081935404589,
1.97862235188254));
#20776=CARTESIAN_POINT('Ctrl Pts',(0.118019173255387,0.101328092440981,
1.9786456013857));
#20777=CARTESIAN_POINT('Ctrl Pts',(0.117395715765617,0.102051193492218,
1.97871391940527));
#20778=CARTESIAN_POINT('Ctrl Pts',(0.116981017506722,0.102526297859334,
1.97875883421953));
#20779=CARTESIAN_POINT('Ctrl Pts',(0.114008381015845,0.105890419083415,
1.97907717527905));
#20780=CARTESIAN_POINT('Ctrl Pts',(0.111346343472478,0.108686199328353,
1.97934337155746));
#20781=CARTESIAN_POINT('Ctrl Pts',(0.107502417612416,0.112433576911384,
1.9797075088671));
#20782=CARTESIAN_POINT('Ctrl Pts',(0.106406748769801,0.11347106712033,1.97980915839058));
#20783=CARTESIAN_POINT('Ctrl Pts',(0.0970379267721891,0.122087359682084,
1.98066225229508));
#20784=CARTESIAN_POINT('Ctrl Pts',(0.0879821903299919,0.128766590670259,
1.98138525082455));
#20785=CARTESIAN_POINT('Ctrl Pts',(0.0733075636240313,0.137313514834558,
1.98252264179783));
#20786=CARTESIAN_POINT('Ctrl Pts',(0.0681720049969127,0.13993414765087,
1.98291464267102));
#20787=CARTESIAN_POINT('Ctrl Pts',(0.0616174750374206,0.14283230052867,
1.98341484555509));
#20788=CARTESIAN_POINT('Ctrl Pts',(0.0603239672736994,0.143383395304276,
1.9835135397042));
#20789=CARTESIAN_POINT('Ctrl Pts',(0.0584431362821732,0.144154761955004,
1.98365710211376));
#20790=CARTESIAN_POINT('Ctrl Pts',(0.0578616440850284,0.144389146738122,
1.98370149445126));
#20791=CARTESIAN_POINT('Ctrl Pts',(0.0568439868182705,0.144792204005907,
1.98377920519604));
#20792=CARTESIAN_POINT('Ctrl Pts',(0.0564084452870791,0.1449624381343,1.98381247074526));
#20793=CARTESIAN_POINT('Ctrl Pts',(0.0555644131828359,0.145287953602485,
1.98387695162242));
#20794=CARTESIAN_POINT('Ctrl Pts',(0.0551560223134122,0.145443482733775,
1.98390815829549));
#20795=CARTESIAN_POINT('Ctrl Pts',(0.0541832565978876,0.145809258712592,
1.98398251089069));
#20796=CARTESIAN_POINT('Ctrl Pts',(0.0536183090507699,0.146017951422052,
1.98402570812693));
#20797=CARTESIAN_POINT('Ctrl Pts',(0.0516041997633292,0.146748702472518,
1.98417977864457));
#20798=CARTESIAN_POINT('Ctrl Pts',(0.0501485553628911,0.147252494676002,
1.98429125297095));
#20799=CARTESIAN_POINT('Ctrl Pts',(0.0350952223025728,0.152213299112027,
1.98544570799005));
#20800=CARTESIAN_POINT('Ctrl Pts',(0.0209544844935645,0.154794307967004,
1.98655363889075));
#20801=CARTESIAN_POINT('Ctrl Pts',(0.00397247037820749,0.155522618564707,
1.98786981194419));
#20802=CARTESIAN_POINT('Ctrl Pts',(0.00127734512879936,0.155568102748949,
1.98807794384487));
#20803=CARTESIAN_POINT('Ctrl Pts',(-0.00491239393441548,0.155511687676728,
1.98855270517993));
#20804=CARTESIAN_POINT('Ctrl Pts',(-0.00840533025798109,0.155362063480086,
1.98881824994742));
#20805=CARTESIAN_POINT('Ctrl Pts',(-0.013769047219835,0.154950848646218,
1.98921974672633));
#20806=CARTESIAN_POINT('Ctrl Pts',(-0.0156449340752918,0.15477270129951,
1.98935897347611));
#20807=CARTESIAN_POINT('Ctrl Pts',(-0.018001654008732,0.154505600647192,
1.98953201452612));
#20808=CARTESIAN_POINT('Ctrl Pts',(-0.0184858234917176,0.154448420275091,
1.98956746457538));
#20809=CARTESIAN_POINT('Ctrl Pts',(-0.0192567164188641,0.15435370089626,
1.98962374045148));
#20810=CARTESIAN_POINT('Ctrl Pts',(-0.0195436123189996,0.154317637776339,
1.98964464709067));
#20811=CARTESIAN_POINT('Ctrl Pts',(-0.0200880085121741,0.154247664059228,
1.98968424586134));
#20812=CARTESIAN_POINT('Ctrl Pts',(-0.0203455211128352,0.15421390898873,
1.98970294598705));
#20813=CARTESIAN_POINT('Ctrl Pts',(-0.0209384454349284,0.154134676719266,
1.98974593334415));
#20814=CARTESIAN_POINT('Ctrl Pts',(-0.0212737942596107,0.154088749583705,
1.98977019501605));
#20815=CARTESIAN_POINT('Ctrl Pts',(-0.0221728474411851,0.15396263027935,
1.98983510817946));
#20816=CARTESIAN_POINT('Ctrl Pts',(-0.0227362731291761,0.15388043604397,
1.98987565005046));
#20817=CARTESIAN_POINT('Ctrl Pts',(-0.0269596957111709,0.153240607256606,
1.99017859863609));
#20818=CARTESIAN_POINT('Ctrl Pts',(-0.0305995653447674,0.15255550191493,
1.99043432520309));
#20819=CARTESIAN_POINT('Ctrl Pts',(-0.0352501274613738,0.151506976033766,
1.99075818682216));
#20820=CARTESIAN_POINT('Ctrl Pts',(-0.0362859753383801,0.15126223375246,
1.99083013610978));
#20821=CARTESIAN_POINT('Ctrl Pts',(-0.0463681469430712,0.14877056514731,
1.99152932766559));
#20822=CARTESIAN_POINT('Ctrl Pts',(-0.0551930951174727,0.145726577715912,
1.99213366936552));
#20823=CARTESIAN_POINT('Ctrl Pts',(-0.0636886415377083,0.141913915593508,
1.99275019838839));
#20824=CARTESIAN_POINT('Origin',(0.,0.,-0.129405622560373));
#20825=CARTESIAN_POINT('',(-0.0636886254669799,0.141913922805787,2.07648623881325));
#20826=CARTESIAN_POINT('',(-0.0636886258537358,0.141913922632217,2.0626609697501));
#20827=CARTESIAN_POINT('',(-0.0636886258329924,0.141913922641526,-0.129405622560373));
#20828=CARTESIAN_POINT('Ctrl Pts',(-0.0636886254669799,0.141913922805787,
2.07648623881325));
#20829=CARTESIAN_POINT('Ctrl Pts',(-0.0622956641982391,0.142539060824529,
2.07638267759085));
#20830=CARTESIAN_POINT('Ctrl Pts',(-0.0608933350929393,0.143143763334241,
2.07627981250369));
#20831=CARTESIAN_POINT('Ctrl Pts',(-0.0501327721664988,0.147597046993911,
2.07549941429699));
#20832=CARTESIAN_POINT('Ctrl Pts',(-0.0404280348378697,0.150544919973361,
2.07484504960544));
#20833=CARTESIAN_POINT('Ctrl Pts',(-0.0239636770900797,0.153837741954139,
2.07372675016692));
#20834=CARTESIAN_POINT('Ctrl Pts',(-0.0173453381300696,0.154723722205612,
2.07327545982922));
#20835=CARTESIAN_POINT('Ctrl Pts',(-0.00917324058954642,0.155286731958653,
2.07270451787251));
#20836=CARTESIAN_POINT('Ctrl Pts',(-0.00765393403831012,0.155369026745032,
2.07259781559541));
#20837=CARTESIAN_POINT('Ctrl Pts',(-0.00548686378400635,0.155454546052616,
2.07244472355231));
#20838=CARTESIAN_POINT('Ctrl Pts',(-0.00483987275185744,0.155476034074275,
2.07239890342213));
#20839=CARTESIAN_POINT('Ctrl Pts',(-0.00372170098785285,0.15550618480947,
2.07231950943887));
#20840=CARTESIAN_POINT('Ctrl Pts',(-0.00325057630437787,0.155516746098265,
2.0722859952406));
#20841=CARTESIAN_POINT('Ctrl Pts',(-0.00234720658276474,0.155532890365862,
2.07222160905139));
#20842=CARTESIAN_POINT('Ctrl Pts',(-0.00191497130348025,0.155538812655423,
2.07219074797147));
#20843=CARTESIAN_POINT('Ctrl Pts',(-0.000788335713863414,0.155549552366646,
2.07211016307335));
#20844=CARTESIAN_POINT('Ctrl Pts',(-9.39245730269155E-5,0.15555152157355,
2.07206035083724));
#20845=CARTESIAN_POINT('Ctrl Pts',(0.00228679373086063,0.155542331271888,
2.07188906877831));
#20846=CARTESIAN_POINT('Ctrl Pts',(0.00397283951082572,0.155508399686774,
2.07176689353877));
#20847=CARTESIAN_POINT('Ctrl Pts',(0.018481944479607,0.154980299326433,
2.07070760637421));
#20848=CARTESIAN_POINT('Ctrl Pts',(0.0311962335365942,0.152928504996118,
2.06971983604702));
#20849=CARTESIAN_POINT('Ctrl Pts',(0.0513942273877773,0.147043716425067,
2.06808843719609));
#20850=CARTESIAN_POINT('Ctrl Pts',(0.0590840368682289,0.144126085969458,
2.06745302953144));
#20851=CARTESIAN_POINT('Ctrl Pts',(0.0672742269164555,0.140252268742962,
2.06678245623224));
#20852=CARTESIAN_POINT('Ctrl Pts',(0.0680372619129649,0.139883707299498,
2.06672005190177));
#20853=CARTESIAN_POINT('Ctrl Pts',(0.0692099695305363,0.139305399607361,
2.06662429172185));
#20854=CARTESIAN_POINT('Ctrl Pts',(0.0696217724159812,0.139100046951471,
2.06659069358713));
#20855=CARTESIAN_POINT('Ctrl Pts',(0.0703044445062772,0.138755829520914,
2.06653505070542));
#20856=CARTESIAN_POINT('Ctrl Pts',(0.0705758245664816,0.138617993544725,
2.06651294569131));
#20857=CARTESIAN_POINT('Ctrl Pts',(0.0711015258838092,0.138349041863207,
2.06647015581293));
#20858=CARTESIAN_POINT('Ctrl Pts',(0.071355893154698,0.138218019386713,
2.06644946536296));
#20859=CARTESIAN_POINT('Ctrl Pts',(0.0718329076586678,0.137970645371728,
2.06641069289501));
#20860=CARTESIAN_POINT('Ctrl Pts',(0.0720556317983023,0.137854457796708,
2.06639260142267));
#20861=CARTESIAN_POINT('Ctrl Pts',(0.0725737291287578,0.137582585449572,
2.06635054368474));
#20862=CARTESIAN_POINT('Ctrl Pts',(0.0728688831807168,0.137426488888788,
2.06632660368311));
#20863=CARTESIAN_POINT('Ctrl Pts',(0.0736413827011932,0.137014752700159,
2.06626399196991));
#20864=CARTESIAN_POINT('Ctrl Pts',(0.0741179055563197,0.136757565796549,
2.06622541549945));
#20865=CARTESIAN_POINT('Ctrl Pts',(0.0773134334108142,0.135011280343933,
2.0659669680923));
#20866=CARTESIAN_POINT('Ctrl Pts',(0.0799889817691292,0.133443542656156,
2.06575176360514));
#20867=CARTESIAN_POINT('Ctrl Pts',(0.0839499587037952,0.13096062448432,
2.06543217899248));
#20868=CARTESIAN_POINT('Ctrl Pts',(0.0852710787834631,0.130104281934588,
2.06532541506364));
#20869=CARTESIAN_POINT('Ctrl Pts',(0.0991200002206248,0.12082590642526,
2.06420188264494));
#20870=CARTESIAN_POINT('Ctrl Pts',(0.110371135606979,0.110643264007005,
2.06324251820545));
#20871=CARTESIAN_POINT('Ctrl Pts',(0.122213737910105,0.0962908557984671,
2.06197063074967));
#20872=CARTESIAN_POINT('Ctrl Pts',(0.124355547833521,0.0935084012003883,
2.0617276108558));
#20873=CARTESIAN_POINT('Ctrl Pts',(0.126914874213432,0.0899399455299788,
2.06141892142732));
#20874=CARTESIAN_POINT('Ctrl Pts',(0.127422369815464,0.0892194973758358,
2.06135674751774));
#20875=CARTESIAN_POINT('Ctrl Pts',(0.128220074770713,0.0880663743923654,
2.06125744846909));
#20876=CARTESIAN_POINT('Ctrl Pts',(0.12851428513708,0.0876364785720714,
2.06122047559546));
#20877=CARTESIAN_POINT('Ctrl Pts',(0.129064946059366,0.086823124805228,
2.06115060713536));
#20878=CARTESIAN_POINT('Ctrl Pts',(0.129321861696096,0.0864399871661661,
2.06111772955062));
#20879=CARTESIAN_POINT('Ctrl Pts',(0.129897051895842,0.0855739033981351,
2.0610434839389));
#20880=CARTESIAN_POINT('Ctrl Pts',(0.130214343201089,0.085090315794578,
2.06100207970718));
#20881=CARTESIAN_POINT('Ctrl Pts',(0.131019008067323,0.0838488753252864,
2.06089591357245));
#20882=CARTESIAN_POINT('Ctrl Pts',(0.131502501246128,0.083088545966045,
2.06083100906028));
#20883=CARTESIAN_POINT('Ctrl Pts',(0.134370274215221,0.0784910230070833,
2.06043919870676));
#20884=CARTESIAN_POINT('Ctrl Pts',(0.136592827608566,0.0745560390962183,
2.06010646297214));
#20885=CARTESIAN_POINT('Ctrl Pts',(0.143560052001153,0.0608606203188363,
2.05895571260128));
#20886=CARTESIAN_POINT('Ctrl Pts',(0.14745357345234,0.0507039054977666,
2.05811184178448));
#20887=CARTESIAN_POINT('Ctrl Pts',(0.152150601679885,0.0331591216091712,
2.05670598908298));
#20888=CARTESIAN_POINT('Ctrl Pts',(0.153541963938232,0.0259658791828275,
2.056144187482));
#20889=CARTESIAN_POINT('Ctrl Pts',(0.154523041124068,0.0178645303840552,
2.05554432202067));
#20890=CARTESIAN_POINT('Ctrl Pts',(0.154617496066022,0.0170276739353214,
2.05548274864821));
#20891=CARTESIAN_POINT('Ctrl Pts',(0.154742616542637,0.0158320777304281,
2.05539537736457));
#20892=CARTESIAN_POINT('Ctrl Pts',(0.154778838314392,0.0154739547903644,
2.05536928295235));
#20893=CARTESIAN_POINT('Ctrl Pts',(0.15483929429916,0.0148547695061723,
2.05532430197778));
#20894=CARTESIAN_POINT('Ctrl Pts',(0.154864112046803,0.0145937671816337,
2.05530538301099));
#20895=CARTESIAN_POINT('Ctrl Pts',(0.154911074279437,0.0140862633715494,
2.05526867841813));
#20896=CARTESIAN_POINT('Ctrl Pts',(0.154933290361797,0.0138397720427953,
2.05525088870563));
#20897=CARTESIAN_POINT('Ctrl Pts',(0.154991877454541,0.0131719130729797,
2.05520278705388));
#20898=CARTESIAN_POINT('Ctrl Pts',(0.155027118778209,0.0127504441300064,
2.05517253791291));
#20899=CARTESIAN_POINT('Ctrl Pts',(0.155152729507844,0.0111706283486375,
2.05505953482104));
#20900=CARTESIAN_POINT('Ctrl Pts',(0.155231842067868,0.0100113852145024,
2.05497738296713));
#20901=CARTESIAN_POINT('Ctrl Pts',(0.155791944253617,0.000184292898756712,
2.05428663311222));
#20902=CARTESIAN_POINT('Ctrl Pts',(0.155559588040781,-0.00851028121019744,
2.05371232045842));
#20903=CARTESIAN_POINT('Ctrl Pts',(0.153576290564738,-0.0263983953322103,
2.05252664374666));
#20904=CARTESIAN_POINT('Ctrl Pts',(0.151720657765623,-0.0355440268302073,
2.05191743976547));
#20905=CARTESIAN_POINT('Ctrl Pts',(0.147820621115431,-0.0486169568909168,
2.05099111143999));
#20906=CARTESIAN_POINT('Ctrl Pts',(0.146410455189692,-0.052711642173404,
2.05069281224681));
#20907=CARTESIAN_POINT('Ctrl Pts',(0.144488664299424,-0.0576169385761271,
2.05032281033137));
#20908=CARTESIAN_POINT('Ctrl Pts',(0.144137925963014,-0.0584888361298803,
2.05025654971203));
#20909=CARTESIAN_POINT('Ctrl Pts',(0.143575610955702,-0.0598509097843598,
2.05015223521));
#20910=CARTESIAN_POINT('Ctrl Pts',(0.143369370442994,-0.0603432769178193,
2.05011436152183));
#20911=CARTESIAN_POINT('Ctrl Pts',(0.142998787155785,-0.0612153621307606,
2.05004697991034));
#20912=CARTESIAN_POINT('Ctrl Pts',(0.142835455174496,-0.0615955065556782,
2.05001750653184));
#20913=CARTESIAN_POINT('Ctrl Pts',(0.142455079509633,-0.0624711569885374,
2.04994937828776));
#20914=CARTESIAN_POINT('Ctrl Pts',(0.142236964852003,-0.0629661889398991,
2.04991068721747));
#20915=CARTESIAN_POINT('Ctrl Pts',(0.141630197430357,-0.0643240640977797,
2.04980406592847));
#20916=CARTESIAN_POINT('Ctrl Pts',(0.141236251522508,-0.0651845014442556,
2.04973595530566));
#20917=CARTESIAN_POINT('Ctrl Pts',(0.139166658612167,-0.0695979544481655,
2.04938370417014));
#20918=CARTESIAN_POINT('Ctrl Pts',(0.137364850536351,-0.0730898544289354,
2.04909524074928));
#20919=CARTESIAN_POINT('Ctrl Pts',(0.134456082216056,-0.0782387950555005,
2.04865443721661));
#20920=CARTESIAN_POINT('Ctrl Pts',(0.133446198495531,-0.0799491001134729,
2.04850534812784));
#20921=CARTESIAN_POINT('Ctrl Pts',(0.124705413320081,-0.0941249997566661,
2.04724720115719));
#20922=CARTESIAN_POINT('Ctrl Pts',(0.115281025177264,-0.105456923556556,
2.04608427625801));
#20923=CARTESIAN_POINT('Ctrl Pts',(0.102440643361194,-0.117084491343859,
2.04478028848023));
#20924=CARTESIAN_POINT('Ctrl Pts',(0.100425413734909,-0.118817515964591,
2.04458268605807));
#20925=CARTESIAN_POINT('Ctrl Pts',(0.097945823662672,-0.120841686436793,
2.04434883590489));
#20926=CARTESIAN_POINT('Ctrl Pts',(0.097523232928543,-0.121182988148829,
2.04430929680956));
#20927=CARTESIAN_POINT('Ctrl Pts',(0.09686332253773,-0.121710271299456,
2.04424805299734));
#20928=CARTESIAN_POINT('Ctrl Pts',(0.0966272411214427,-0.121897783697298,
2.04422624174622));
#20929=CARTESIAN_POINT('Ctrl Pts',(0.0961883335620947,-0.122244318519215,
2.04418587641576));
#20930=CARTESIAN_POINT('Ctrl Pts',(0.0959856593201225,-0.122403521724124,
2.04416730981567));
#20931=CARTESIAN_POINT('Ctrl Pts',(0.0955266422449359,-0.122762244343472,
2.04412542363151));
#20932=CARTESIAN_POINT('Ctrl Pts',(0.0952700700840349,-0.122961464557996,
2.0441021253196));
#20933=CARTESIAN_POINT('Ctrl Pts',(0.0945112639360413,-0.123546852840624,
2.0440335514161));
#20934=CARTESIAN_POINT('Ctrl Pts',(0.094007284397356,-0.123930764439978,
2.0439884312012));
#20935=CARTESIAN_POINT('Ctrl Pts',(0.0903602841157865,-0.126673855575282,
2.04366485355056));
#20936=CARTESIAN_POINT('Ctrl Pts',(0.087130866571543,-0.128916505453164,
2.04339389888893));
#20937=CARTESIAN_POINT('Ctrl Pts',(0.0733305352821005,-0.137744237186509,
2.04228342656825));
#20938=CARTESIAN_POINT('Ctrl Pts',(0.0620732647582102,-0.143170522243238,
2.04148551987718));
#20939=CARTESIAN_POINT('Ctrl Pts',(0.0461828845534744,-0.14859935672349,
2.04036212179378));
#20940=CARTESIAN_POINT('Ctrl Pts',(0.0420205066458944,-0.149829568925271,
2.04006850765254));
#20941=CARTESIAN_POINT('Ctrl Pts',(0.0352505636585199,-0.151526154500328,
2.03958770926936));
#20942=CARTESIAN_POINT('Ctrl Pts',(0.0326729245129962,-0.152102782015107,
2.03940392408859));
#20943=CARTESIAN_POINT('Ctrl Pts',(0.029297282843071,-0.152768162252996,
2.03916174674579));
#20944=CARTESIAN_POINT('Ctrl Pts',(0.0285114137604122,-0.152916779401914,
2.03910526267879));
#20945=CARTESIAN_POINT('Ctrl Pts',(0.0272296083086953,-0.153148959611894,
2.03901294912769));
#20946=CARTESIAN_POINT('Ctrl Pts',(0.0267343437212509,-0.153236191070581,
2.03897723633928));
#20947=CARTESIAN_POINT('Ctrl Pts',(0.0257798507721272,-0.153399538704556,
2.03890831930405));
#20948=CARTESIAN_POINT('Ctrl Pts',(0.0253206859403374,-0.153475998238991,
2.0388751263305));
#20949=CARTESIAN_POINT('Ctrl Pts',(0.0242668610774355,-0.15364662195843,
2.03879885022507));
#20950=CARTESIAN_POINT('Ctrl Pts',(0.0236719869564152,-0.153739396383812,
2.03875572366253));
#20951=CARTESIAN_POINT('Ctrl Pts',(0.0220866021974973,-0.153977227696996,
2.03864059534232));
#20952=CARTESIAN_POINT('Ctrl Pts',(0.0210952189776232,-0.154116177914693,
2.03856840242787));
#20953=CARTESIAN_POINT('Ctrl Pts',(0.0134071135609243,-0.155118156869436,
2.03800691375735));
#20954=CARTESIAN_POINT('Ctrl Pts',(0.00666297273687062,-0.155553762860099,
2.03750427294359));
#20955=CARTESIAN_POINT('Ctrl Pts',(-0.0141459425090446,-0.155542087656156,
2.03592200441384));
#20956=CARTESIAN_POINT('Ctrl Pts',(-0.0281371985521883,-0.153628472660792,
2.03480803373935));
#20957=CARTESIAN_POINT('Ctrl Pts',(-0.0438165474941609,-0.149267641069909,
2.03358864838604));
#20958=CARTESIAN_POINT('Ctrl Pts',(-0.0459398808129136,-0.148627881769986,
2.03342434272078));
#20959=CARTESIAN_POINT('Ctrl Pts',(-0.0485380148355302,-0.147784058772046,
2.03322490826515));
#20960=CARTESIAN_POINT('Ctrl Pts',(-0.0490262957991695,-0.147622793808001,
2.03318749845901));
#20961=CARTESIAN_POINT('Ctrl Pts',(-0.049793555065181,-0.147365163708992,
2.03312883620861));
#20962=CARTESIAN_POINT('Ctrl Pts',(-0.0500730680785558,-0.14727042288991,
2.0331074910005));
#20963=CARTESIAN_POINT('Ctrl Pts',(-0.050596937468862,-0.147091193700875,
2.03306753540786));
#20964=CARTESIAN_POINT('Ctrl Pts',(-0.0508413499077227,-0.147006892650091,
2.03304891481324));
#20965=CARTESIAN_POINT('Ctrl Pts',(-0.0514011033278442,-0.146812263398327,
2.03300631622792));
#20966=CARTESIAN_POINT('Ctrl Pts',(-0.0517162995560982,-0.146701528531079,
2.03298236255744));
#20967=CARTESIAN_POINT('Ctrl Pts',(-0.0525420369383522,-0.146408438122534,
2.03291969164084));
#20968=CARTESIAN_POINT('Ctrl Pts',(-0.0530519918333324,-0.146224425404003,
2.03288106992796));
#20969=CARTESIAN_POINT('Ctrl Pts',(-0.0564831615006314,-0.144966005381496,
2.03262169656346));
#20970=CARTESIAN_POINT('Ctrl Pts',(-0.0593727811244302,-0.143806698817963,
2.0324056494206));
#20971=CARTESIAN_POINT('Ctrl Pts',(-0.0672834943167241,-0.140353789861725,
2.03181566243648));
#20972=CARTESIAN_POINT('Ctrl Pts',(-0.0722204444082067,-0.137878469120591,
2.03144906853591));
#20973=CARTESIAN_POINT('Ctrl Pts',(-0.0832715841753618,-0.131580739529127,
2.03060954000382));
#20974=CARTESIAN_POINT('Ctrl Pts',(-0.0892722067334473,-0.127585728471211,
2.03013901343866));
#20975=CARTESIAN_POINT('Ctrl Pts',(-0.100077927781603,-0.119254925037336,
2.02922907721691));
#20976=CARTESIAN_POINT('Ctrl Pts',(-0.104931359887628,-0.115007487633497,
2.02879253407257));
#20977=CARTESIAN_POINT('Ctrl Pts',(-0.110567754109858,-0.109420312700081,
2.02823919231511));
#20978=CARTESIAN_POINT('Ctrl Pts',(-0.111613216522664,-0.108353692626021,
2.02813442941121));
#20979=CARTESIAN_POINT('Ctrl Pts',(-0.113086240088601,-0.106806917631759,
2.02798363728355));
#20980=CARTESIAN_POINT('Ctrl Pts',(-0.113526459297088,-0.10633888455524,
2.02793815422475));
#20981=CARTESIAN_POINT('Ctrl Pts',(-0.114283910416013,-0.1055235120114,
2.02785915778206));
#20982=CARTESIAN_POINT('Ctrl Pts',(-0.114602492455259,-0.10517743332744,
2.02782570242702));
#20983=CARTESIAN_POINT('Ctrl Pts',(-0.115211541653921,-0.104509764894284,
2.02776129753977));
#20984=CARTESIAN_POINT('Ctrl Pts',(-0.115502244748372,-0.104188395417229,
2.02773035839867));
#20985=CARTESIAN_POINT('Ctrl Pts',(-0.1162591682289,-0.103344562661583,
2.02764927582197));
#20986=CARTESIAN_POINT('Ctrl Pts',(-0.116723205660322,-0.102820163682231,
2.02759904181125));
#20987=CARTESIAN_POINT('Ctrl Pts',(-0.118315558996756,-0.100996007108689,
2.02742481519868));
#20988=CARTESIAN_POINT('Ctrl Pts',(-0.119425794932187,-0.0996807103456938,
2.02730008422493));
#20989=CARTESIAN_POINT('Ctrl Pts',(-0.128250601605122,-0.0888668690956211,
2.02628133144113));
#20990=CARTESIAN_POINT('Ctrl Pts',(-0.134839949250607,-0.0785085994329739,
2.02534176834917));
#20991=CARTESIAN_POINT('Ctrl Pts',(-0.144172332924226,-0.0591288899052643,
2.0236736350441));
#20992=CARTESIAN_POINT('Ctrl Pts',(-0.147442357570033,-0.0504250050080329,
2.02295370601324));
#20993=CARTESIAN_POINT('Ctrl Pts',(-0.150149450267487,-0.0406411573268049,
2.02220710332032));
#20994=CARTESIAN_POINT('Ctrl Pts',(-0.15037466444079,-0.0397997672469219,
2.0221433980682));
#20995=CARTESIAN_POINT('Ctrl Pts',(-0.150684189515607,-0.0386032469044976,
2.02205355582785));
#20996=CARTESIAN_POINT('Ctrl Pts',(-0.150774330790832,-0.0382496643579215,
2.02202709937596));
#20997=CARTESIAN_POINT('Ctrl Pts',(-0.150927308030161,-0.0376406611782481,
2.02198169459924));
#20998=CARTESIAN_POINT('Ctrl Pts',(-0.150990741503492,-0.0373853937764408,
2.02196271220281));
#20999=CARTESIAN_POINT('Ctrl Pts',(-0.151112275946203,-0.0368909627182981,
2.02192604165093));
#21000=CARTESIAN_POINT('Ctrl Pts',(-0.151170456807011,-0.0366518220965108,
2.02190834879256));
#21001=CARTESIAN_POINT('Ctrl Pts',(-0.151325436000783,-0.0360081646349967,
2.02186084218308));
#21002=CARTESIAN_POINT('Ctrl Pts',(-0.151421180792036,-0.0356033919664265,
2.02183108850226));
#21003=CARTESIAN_POINT('Ctrl Pts',(-0.151767844169232,-0.0341111350924579,
2.02172182735174));
#21004=CARTESIAN_POINT('Ctrl Pts',(-0.152008688745958,-0.0330213082348758,
2.02164287205648));
#21005=CARTESIAN_POINT('Ctrl Pts',(-0.15442992732813,-0.0214767975179839,
2.02081443718909));
#21006=CARTESIAN_POINT('Ctrl Pts',(-0.155540202820391,-0.0108248506606018,
2.02011743063371));
#21007=CARTESIAN_POINT('Ctrl Pts',(-0.155560302101737,0.0112373727802485,
2.01866513464362));
#21008=CARTESIAN_POINT('Ctrl Pts',(-0.154322110730638,0.0225812930458725,
2.01791198472153));
#21009=CARTESIAN_POINT('Ctrl Pts',(-0.151636560304613,0.0346872309812885,
2.017043532115));
#21010=CARTESIAN_POINT('Ctrl Pts',(-0.151405004891444,0.035684377805913,
2.01697153646969));
#21011=CARTESIAN_POINT('Ctrl Pts',(-0.151020102685495,0.0372706528698454,
2.01685623147798));
#21012=CARTESIAN_POINT('Ctrl Pts',(-0.150873107501336,0.0378613047096332,
2.01681312567815));
#21013=CARTESIAN_POINT('Ctrl Pts',(-0.150607328735998,0.0389031191262123,
2.01673678304527));
#21014=CARTESIAN_POINT('Ctrl Pts',(-0.150489974184245,0.0393546415062859,
2.01670359257791));
#21015=CARTESIAN_POINT('Ctrl Pts',(-0.15024263460625,0.0402889968625491,
2.01663469185344));
#21016=CARTESIAN_POINT('Ctrl Pts',(-0.150112349265498,0.040771744000529,
2.0165989722337));
#21017=CARTESIAN_POINT('Ctrl Pts',(-0.149771074962268,0.0420124580669351,
2.01650685191165));
#21018=CARTESIAN_POINT('Ctrl Pts',(-0.149556660921137,0.0427694594317817,
2.01645034084643));
#21019=CARTESIAN_POINT('Ctrl Pts',(-0.148630377915502,0.0459475995510569,
2.01621177482298));
#21020=CARTESIAN_POINT('Ctrl Pts',(-0.147865423946665,0.0483527264690689,
2.01602800578432));
#21021=CARTESIAN_POINT('Ctrl Pts',(-0.145713541323103,0.0545890290017992,
2.01554265878334));
#21022=CARTESIAN_POINT('Ctrl Pts',(-0.144234082964366,0.0583859759634611,
2.01523822225201));
#21023=CARTESIAN_POINT('Ctrl Pts',(-0.13938954509522,0.0695074335783611,
2.01431977051335));
#21024=CARTESIAN_POINT('Ctrl Pts',(-0.135602763390633,0.0766328738180134,
2.01369489681868));
#21025=CARTESIAN_POINT('Ctrl Pts',(-0.128732118665179,0.0874439088646362,
2.01270179098782));
#21026=CARTESIAN_POINT('Ctrl Pts',(-0.125999973096993,0.0913367763181533,
2.01233409209679));
#21027=CARTESIAN_POINT('Ctrl Pts',(-0.12261310589936,0.0957206704723943,
2.01191213571528));
#21028=CARTESIAN_POINT('Ctrl Pts',(-0.122127775013948,0.0963391255181204,
2.01185241959857));
#21029=CARTESIAN_POINT('Ctrl Pts',(-0.119619790163518,0.0994856284254031,
2.0115477288606));
#21030=CARTESIAN_POINT('Ctrl Pts',(-0.117523064912813,0.101953997502343,
2.01130577849402));
#21031=CARTESIAN_POINT('Ctrl Pts',(-0.114982703484846,0.104762021570553,
2.01102872129042));
#21032=CARTESIAN_POINT('Ctrl Pts',(-0.11461262420535,0.105166770707655,
2.01098874083407));
#21033=CARTESIAN_POINT('Ctrl Pts',(-0.114014822348431,0.105813672377685,
2.01092477967614));
#21034=CARTESIAN_POINT('Ctrl Pts',(-0.113788455328879,0.106057062078243,
2.01090070090923));
#21035=CARTESIAN_POINT('Ctrl Pts',(-0.113384324958633,0.10648879952654,
2.01085796658071));
#21036=CARTESIAN_POINT('Ctrl Pts',(-0.113206869704387,0.106677430728051,
2.01083928799336));
#21037=CARTESIAN_POINT('Ctrl Pts',(-0.112827804047411,0.107078358440092,
2.01079957229733));
#21038=CARTESIAN_POINT('Ctrl Pts',(-0.112626065590584,0.107290528779731,
2.01077854535154));
#21039=CARTESIAN_POINT('Ctrl Pts',(-0.112075729295951,0.107866060231829,
2.01072147774326));
#21040=CARTESIAN_POINT('Ctrl Pts',(-0.111725960018593,0.108228304633786,
2.01068552608728));
#21041=CARTESIAN_POINT('Ctrl Pts',(-0.109924909567356,0.110075556614684,
2.01050198180508));
#21042=CARTESIAN_POINT('Ctrl Pts',(-0.108445668527572,0.111533187983041,
2.01035644954798));
#21043=CARTESIAN_POINT('Ctrl Pts',(-0.104006035602545,0.115736091994582,
2.00993306327408));
#21044=CARTESIAN_POINT('Ctrl Pts',(-0.100967307051048,0.118396396922867,
2.00966012666005));
#21045=CARTESIAN_POINT('Ctrl Pts',(-0.0897110258034188,0.127501920840473,
2.0086930532087));
#21046=CARTESIAN_POINT('Ctrl Pts',(-0.0809533057685513,0.133234309466336,
2.00801826008367));
#21047=CARTESIAN_POINT('Ctrl Pts',(-0.0690575512143196,0.139411751654174,
2.00712180705218));
#21048=CARTESIAN_POINT('Ctrl Pts',(-0.0663902784791855,0.140701465633334,
2.00692214555917));
#21049=CARTESIAN_POINT('Ctrl Pts',(-0.0636886213818939,0.141913924639106,
2.00672033358865));
#21050=CARTESIAN_POINT('Ctrl Pts',(-0.0636886415377083,0.141913915593508,
1.99275019838839));
#21051=CARTESIAN_POINT('Ctrl Pts',(-0.0659295067654324,0.140908251972531,
1.99291281988216));
#21052=CARTESIAN_POINT('Ctrl Pts',(-0.0681474586421175,0.139849106147085,
1.99307621311931));
#21053=CARTESIAN_POINT('Ctrl Pts',(-0.0760409509781415,0.135847058992824,
1.99366877675381));
#21054=CARTESIAN_POINT('Ctrl Pts',(-0.0815570810836566,0.132608729824859,
1.99410418843428));
#21055=CARTESIAN_POINT('Ctrl Pts',(-0.0877197972569616,0.128460573608094,
1.99462516695988));
#21056=CARTESIAN_POINT('Ctrl Pts',(-0.0885757879803293,0.127871855750594,
1.99469833746096));
#21057=CARTESIAN_POINT('Ctrl Pts',(-0.0898799526677652,0.126955522475936,
1.99481109878956));
#21058=CARTESIAN_POINT('Ctrl Pts',(-0.0903323895013006,0.126634000059944,
1.99485045751132));
#21059=CARTESIAN_POINT('Ctrl Pts',(-0.0911528169516215,0.126044332574184,
1.99492227244918));
#21060=CARTESIAN_POINT('Ctrl Pts',(-0.0915213711699218,0.125776978908624,
1.99495469797023));
#21061=CARTESIAN_POINT('Ctrl Pts',(-0.092321649304316,0.125191067702659,
1.99502546976428));
#21062=CARTESIAN_POINT('Ctrl Pts',(-0.0927529081027762,0.124871887900985,
1.99506383988522));
#21063=CARTESIAN_POINT('Ctrl Pts',(-0.0939251448602356,0.123994878451579,
1.99516877859051));
#21064=CARTESIAN_POINT('Ctrl Pts',(-0.0946627882311197,0.123432650357648,
1.99523551843242));
#21065=CARTESIAN_POINT('Ctrl Pts',(-0.0983201738720321,0.120592941957311,
1.99557002540584));
#21066=CARTESIAN_POINT('Ctrl Pts',(-0.101162728139163,0.118218494110107,
1.99584161487959));
#21067=CARTESIAN_POINT('Ctrl Pts',(-0.106137774128673,0.113751823680932,
1.99633903664036));
#21068=CARTESIAN_POINT('Ctrl Pts',(-0.108299950952198,0.111695224259176,
1.99656340298458));
#21069=CARTESIAN_POINT('Ctrl Pts',(-0.117750360549141,0.102173775519954,
1.99758138346462));
#21070=CARTESIAN_POINT('Ctrl Pts',(-0.124335348921754,0.0940495339662865,
1.99839750342246));
#21071=CARTESIAN_POINT('Ctrl Pts',(-0.132310083693187,0.0818945281708711,
1.99951703491615));
#21072=CARTESIAN_POINT('Ctrl Pts',(-0.1344264485133,0.0783722357780731,
1.99983059234704));
#21073=CARTESIAN_POINT('Ctrl Pts',(-0.137410555344571,0.0729284065147789,
2.00029512154242));
#21074=CARTESIAN_POINT('Ctrl Pts',(-0.138382735207229,0.07106639839316,
2.00045060351455));
#21075=CARTESIAN_POINT('Ctrl Pts',(-0.139541706178438,0.0687325981454354,
2.00064079708964));
#21076=CARTESIAN_POINT('Ctrl Pts',(-0.13976424258211,0.0682789449655296,
2.00067755127871));
#21077=CARTESIAN_POINT('Ctrl Pts',(-0.140112366600801,0.0675604405742558,
2.00073541291713));
#21078=CARTESIAN_POINT('Ctrl Pts',(-0.140239420301018,0.0672963104678515,
2.00075660906916));
#21079=CARTESIAN_POINT('Ctrl Pts',(-0.140477259860115,0.0667982705375294,
2.00079643410837));
#21080=CARTESIAN_POINT('Ctrl Pts',(-0.140588207116117,0.0665644462598389,
2.00081507248054));
#21081=CARTESIAN_POINT('Ctrl Pts',(-0.140839960601495,0.0660304318748239,
2.00085750625565));
#21082=CARTESIAN_POINT('Ctrl Pts',(-0.140980390860375,0.0657300679613546,
2.00088127832179));
#21083=CARTESIAN_POINT('Ctrl Pts',(-0.141349461711278,0.0649340444014101,
2.00094403294516));
#21084=CARTESIAN_POINT('Ctrl Pts',(-0.141576458335859,0.0644376203551805,
2.00098291700644));
#21085=CARTESIAN_POINT('Ctrl Pts',(-0.14311136559926,0.0610336301267154,
2.00124789887992));
#21086=CARTESIAN_POINT('Ctrl Pts',(-0.144332348369394,0.0580873819299934,
2.00146905772512));
#21087=CARTESIAN_POINT('Ctrl Pts',(-0.149151565430716,0.0453660745643028,
2.00239813675768));
#21088=CARTESIAN_POINT('Ctrl Pts',(-0.151854011060097,0.0352799077316714,
2.00307236675239));
#21089=CARTESIAN_POINT('Ctrl Pts',(-0.15487204992713,0.0167446394367718,
2.00431361254714));
#21090=CARTESIAN_POINT('Ctrl Pts',(-0.155548050857297,0.00839699159754889,
2.00487332405944));
#21091=CARTESIAN_POINT('Ctrl Pts',(-0.155550386707495,-0.00164427078440397,
2.00557165516019));
#21092=CARTESIAN_POINT('Ctrl Pts',(-0.155523545903709,-0.00332456260169045,
2.00568931425222));
#21093=CARTESIAN_POINT('Ctrl Pts',(-0.155447185702821,-0.00569698472505324,
2.00585671346099));
#21094=CARTESIAN_POINT('Ctrl Pts',(-0.15542024968967,-0.00638976808876266,
2.00590575005783));
#21095=CARTESIAN_POINT('Ctrl Pts',(-0.155369015268921,-0.00751386706984123,
2.00598557497369));
#21096=CARTESIAN_POINT('Ctrl Pts',(-0.155347549631766,-0.007945308081525,
2.00601627455787));
#21097=CARTESIAN_POINT('Ctrl Pts',(-0.155298910944775,-0.00884719239914593,
2.00608058128611));
#21098=CARTESIAN_POINT('Ctrl Pts',(-0.155271396753662,-0.00931761209518696,
2.00611419877615));
#21099=CARTESIAN_POINT('Ctrl Pts',(-0.155200977947752,-0.0104344956134807,
2.00619419707285));
#21100=CARTESIAN_POINT('Ctrl Pts',(-0.155156171393645,-0.0110808262140838,
2.00624063688124));
#21101=CARTESIAN_POINT('Ctrl Pts',(-0.15499233291652,-0.0132478660049204,
2.00639684259684));
#21102=CARTESIAN_POINT('Ctrl Pts',(-0.154854973906559,-0.0147670567423603,
2.00650717859744));
#21103=CARTESIAN_POINT('Ctrl Pts',(-0.153993412492537,-0.0229517811484808,
2.0071062994384));
#21104=CARTESIAN_POINT('Ctrl Pts',(-0.152861266896919,-0.0295662744533617,
2.00760771898174));
#21105=CARTESIAN_POINT('Ctrl Pts',(-0.148882868968545,-0.0462472926325519,
2.00891576340107));
#21106=CARTESIAN_POINT('Ctrl Pts',(-0.14544236669537,-0.0561374759163516,
2.00973461506975));
#21107=CARTESIAN_POINT('Ctrl Pts',(-0.140564199489494,-0.0666240533041674,
2.01062124352319));
#21108=CARTESIAN_POINT('Ctrl Pts',(-0.140080496477213,-0.0676351481426719,
2.01070690244764));
#21109=CARTESIAN_POINT('Ctrl Pts',(-0.138982764533249,-0.0698674585557329,
2.01089628655035));
#21110=CARTESIAN_POINT('Ctrl Pts',(-0.138363472299371,-0.0710860068342946,
2.01099984404389));
#21111=CARTESIAN_POINT('Ctrl Pts',(-0.136497972403392,-0.0746398817964052,
2.01130209409804));
#21112=CARTESIAN_POINT('Ctrl Pts',(-0.135208043454808,-0.0769519049034672,
2.01149902210868));
#21113=CARTESIAN_POINT('Ctrl Pts',(-0.133596917796872,-0.0796739109222784,
2.01173026854864));
#21114=CARTESIAN_POINT('Ctrl Pts',(-0.133331993312816,-0.0801164658845744,
2.01176784593683));
#21115=CARTESIAN_POINT('Ctrl Pts',(-0.132896011811974,-0.0808366182512552,
2.01182895191934));
#21116=CARTESIAN_POINT('Ctrl Pts',(-0.132726277524423,-0.0811150051817774,
2.01185256308669));
#21117=CARTESIAN_POINT('Ctrl Pts',(-0.132420803846081,-0.0816124968203796,
2.01189473601011));
#21118=CARTESIAN_POINT('Ctrl Pts',(-0.132285394682787,-0.0818317987438611,
2.01191331881083));
#21119=CARTESIAN_POINT('Ctrl Pts',(-0.131990981301701,-0.0823059754455963,
2.01195348175341));
#21120=CARTESIAN_POINT('Ctrl Pts',(-0.131831784095458,-0.082560725804757,
2.01197504891143));
#21121=CARTESIAN_POINT('Ctrl Pts',(-0.131385162524668,-0.0832708323799327,
2.01203514248444));
#21122=CARTESIAN_POINT('Ctrl Pts',(-0.131096106371519,-0.0837251657150525,
2.01207356325924));
#21123=CARTESIAN_POINT('Ctrl Pts',(-0.129407878379087,-0.0863485132256423,
2.0122953030524));
#21124=CARTESIAN_POINT('Ctrl Pts',(-0.127957146095269,-0.0884840979293851,
2.01247540146454));
#21125=CARTESIAN_POINT('Ctrl Pts',(-0.117882336006377,-0.102548566536947,
2.01366590282081));
#21126=CARTESIAN_POINT('Ctrl Pts',(-0.107655117128448,-0.113238416168053,
2.01459894161699));
#21127=CARTESIAN_POINT('Ctrl Pts',(-0.0946054956039685,-0.123487249446223,
2.01571369326784));
#21128=CARTESIAN_POINT('Ctrl Pts',(-0.0931139176140669,-0.124615803709299,
2.01584003214628));
#21129=CARTESIAN_POINT('Ctrl Pts',(-0.0883233405260521,-0.128106403820624,
2.01624313652608));
#21130=CARTESIAN_POINT('Ctrl Pts',(-0.0849523402498439,-0.130366246246945,
2.01652293427757));
#21131=CARTESIAN_POINT('Ctrl Pts',(-0.0807552845029284,-0.132947903467398,
2.01686885663126));
#21132=CARTESIAN_POINT('Ctrl Pts',(-0.0800096575520494,-0.133397959710826,
2.01693021839148));
#21133=CARTESIAN_POINT('Ctrl Pts',(-0.0787707053861322,-0.134131660107886,
2.0170320467989));
#21134=CARTESIAN_POINT('Ctrl Pts',(-0.0782795257203924,-0.134418905321041,
2.0170723825358));
#21135=CARTESIAN_POINT('Ctrl Pts',(-0.0773880969538388,-0.134933675965478,
2.01714553144304));
#21136=CARTESIAN_POINT('Ctrl Pts',(-0.0769883907661303,-0.135162132783489,
2.0171783105862));
#21137=CARTESIAN_POINT('Ctrl Pts',(-0.0761289369420461,-0.135648314579584,
2.01724875337051));
#21138=CARTESIAN_POINT('Ctrl Pts',(-0.0756688830354267,-0.135905483391047,
2.01728643642874));
#21139=CARTESIAN_POINT('Ctrl Pts',(-0.074411443319843,-0.136600024594322,
2.01738937399213));
#21140=CARTESIAN_POINT('Ctrl Pts',(-0.0736115254526333,-0.137032743792812,
2.01745479287816));
#21141=CARTESIAN_POINT('Ctrl Pts',(-0.0693768245629854,-0.139275746310099,
2.01780082568479));
#21142=CARTESIAN_POINT('Ctrl Pts',(-0.0658792464462353,-0.140963815223183,
2.01808567991663));
#21143=CARTESIAN_POINT('Ctrl Pts',(-0.048753792805651,-0.148452635883011,
2.01947755859141));
#21144=CARTESIAN_POINT('Ctrl Pts',(-0.0344081616866966,-0.152417350352893,
2.02064487763983));
#21145=CARTESIAN_POINT('Ctrl Pts',(-0.0153185102369249,-0.154857564493456,
2.02211552489108));
#21146=CARTESIAN_POINT('Ctrl Pts',(-0.0108910606314268,-0.155231813569472,
2.02245016133008));
#21147=CARTESIAN_POINT('Ctrl Pts',(-0.0057931781380897,-0.15544348797723,
2.02282389775578));
#21148=CARTESIAN_POINT('Ctrl Pts',(-0.00513298184586722,-0.155466689058483,
2.02287207477008));
#21149=CARTESIAN_POINT('Ctrl Pts',(-0.00414677422885363,-0.15549505793179,
2.02294368909488));
#21150=CARTESIAN_POINT('Ctrl Pts',(-0.00382087365323242,-0.155503407382418,
2.02296729710379));
#21151=CARTESIAN_POINT('Ctrl Pts',(-0.00323727622467037,-0.155516523139748,
2.0230094666264));
#21152=CARTESIAN_POINT('Ctrl Pts',(-0.00297959274270772,-0.155521673593919,
2.02302804917019));
#21153=CARTESIAN_POINT('Ctrl Pts',(-0.00242150752508936,-0.155531440742266,
2.02306821410918));
#21154=CARTESIAN_POINT('Ctrl Pts',(-0.00212110567102773,-0.155535827618446,
2.02308978350927));
#21155=CARTESIAN_POINT('Ctrl Pts',(-0.00128210490235176,-0.155545648669994,
2.02314988964436));
#21156=CARTESIAN_POINT('Ctrl Pts',(-0.000743480522906277,-0.155549155808656,
2.02318832066765));
#21157=CARTESIAN_POINT('Ctrl Pts',(0.00237865322313336,-0.155553267237506,
2.02341023810044));
#21158=CARTESIAN_POINT('Ctrl Pts',(0.00496203411082411,-0.155492306120507,
2.02359049786631));
#21159=CARTESIAN_POINT('Ctrl Pts',(0.0222427478418889,-0.154653346680389,
2.02478099672134));
#21160=CARTESIAN_POINT('Ctrl Pts',(0.0367683410044081,-0.151857156426241,
2.02571392410982));
#21161=CARTESIAN_POINT('Ctrl Pts',(0.0524565458918681,-0.146450064412463,
2.02682873158536));
#21162=CARTESIAN_POINT('Ctrl Pts',(0.0542160878541514,-0.145807839304556,
2.02695525247829));
#21163=CARTESIAN_POINT('Ctrl Pts',(0.0597462589502703,-0.143675409901083,
2.02735834430233));
#21164=CARTESIAN_POINT('Ctrl Pts',(0.0634701756898142,-0.142069598330497,
2.02763794011654));
#21165=CARTESIAN_POINT('Ctrl Pts',(0.067912342471643,-0.139944540441079,
2.0279836390518));
#21166=CARTESIAN_POINT('Ctrl Pts',(0.0686946310004803,-0.13956220217551,
2.02804498671529));
#21167=CARTESIAN_POINT('Ctrl Pts',(0.0699826999816077,-0.138919213582391,
2.02814679655859));
#21168=CARTESIAN_POINT('Ctrl Pts',(0.0704903413816263,-0.138662316277217,
2.0281871279123));
#21169=CARTESIAN_POINT('Ctrl Pts',(0.071406190636718,-0.13819251207748,
2.02826027213041));
#21170=CARTESIAN_POINT('Ctrl Pts',(0.0718148863433307,-0.137980565829659,
2.02829305098781));
#21171=CARTESIAN_POINT('Ctrl Pts',(0.0726894720928879,-0.137522074529898,
2.02836349677016));
#21172=CARTESIAN_POINT('Ctrl Pts',(0.0731550606901421,-0.13727497011088,
2.02840118312784));
#21173=CARTESIAN_POINT('Ctrl Pts',(0.0744207125545904,-0.136594976242711,
2.0285041389027));
#21174=CARTESIAN_POINT('Ctrl Pts',(0.0752182377442761,-0.136157433279345,
2.02856957279891));
#21175=CARTESIAN_POINT('Ctrl Pts',(0.079401847608405,-0.133814222606186,
2.02891582871522));
#21176=CARTESIAN_POINT('Ctrl Pts',(0.0827191925923217,-0.131789338564454,
2.02920089756358));
#21177=CARTESIAN_POINT('Ctrl Pts',(0.0982980443006547,-0.121460080779554,
2.0305928701092));
#21178=CARTESIAN_POINT('Ctrl Pts',(0.109406498338138,-0.111557733315848,
2.03176003242717));
#21179=CARTESIAN_POINT('Ctrl Pts',(0.121806201721761,-0.096844003671483,
2.03323042458583));
#21180=CARTESIAN_POINT('Ctrl Pts',(0.124520793115587,-0.0933278790597643,
2.0335649718279));
#21181=CARTESIAN_POINT('Ctrl Pts',(0.127462404890553,-0.0891603844616638,
2.03393862094529));
#21182=CARTESIAN_POINT('Ctrl Pts',(0.12783988429209,-0.0886182985843388,
2.03398679519217));
#21183=CARTESIAN_POINT('Ctrl Pts',(0.128398489373458,-0.0878051063402355,
2.03405840622056));
#21184=CARTESIAN_POINT('Ctrl Pts',(0.128582227877228,-0.0875358181102728,
2.03408201367779));
#21185=CARTESIAN_POINT('Ctrl Pts',(0.128909713173859,-0.0870525977554549,
2.03412418260647));
#21186=CARTESIAN_POINT('Ctrl Pts',(0.129053775439971,-0.0868388851538524,
2.03414276510544));
#21187=CARTESIAN_POINT('Ctrl Pts',(0.129364619923896,-0.0863752735065383,
2.0341829303934));
#21188=CARTESIAN_POINT('Ctrl Pts',(0.129531209083509,-0.0861252497175579,
2.0342045001853));
#21189=CARTESIAN_POINT('Ctrl Pts',(0.129994446390192,-0.0854256199753461,
2.03426460851578));
#21190=CARTESIAN_POINT('Ctrl Pts',(0.13028948905437,-0.0849749475159753,
2.03430304133015));
#21191=CARTESIAN_POINT('Ctrl Pts',(0.131986233785652,-0.0823535862488677,
2.03452498982694));
#21192=CARTESIAN_POINT('Ctrl Pts',(0.133336121663183,-0.0801496091288603,
2.03470527780933));
#21193=CARTESIAN_POINT('Ctrl Pts',(0.142002027821914,-0.0651752387698346,
2.03589577624097));
#21194=CARTESIAN_POINT('Ctrl Pts',(0.147529322219419,-0.051454796736749,
2.03682868415735));
#21195=CARTESIAN_POINT('Ctrl Pts',(0.151493585331642,-0.0353412780026672,
2.03794350148228));
#21196=CARTESIAN_POINT('Ctrl Pts',(0.151908232938729,-0.0335141866107135,
2.0380700542804));
#21197=CARTESIAN_POINT('Ctrl Pts',(0.153115356514492,-0.0277114093767737,
2.03847314391399));
#21198=CARTESIAN_POINT('Ctrl Pts',(0.15378542477098,-0.0237122930794578,
2.03875270434106));
#21199=CARTESIAN_POINT('Ctrl Pts',(0.154408745376138,-0.0188281690260305,
2.03909836412465));
#21200=CARTESIAN_POINT('Ctrl Pts',(0.154511714464416,-0.017963591954249,
2.03915970931702));
#21201=CARTESIAN_POINT('Ctrl Pts',(0.154669955749086,-0.0165327243716809,
2.03926151590604));
#21202=CARTESIAN_POINT('Ctrl Pts',(0.154729389912909,-0.0159669054030455,
2.03930184649137));
#21203=CARTESIAN_POINT('Ctrl Pts',(0.154831300044196,-0.0149426564381052,
2.03937498988753));
#21204=CARTESIAN_POINT('Ctrl Pts',(0.154874847585,-0.0144843374709726,2.03940776869491));
#21205=CARTESIAN_POINT('Ctrl Pts',(0.154963888522164,-0.0135008739957278,
2.03947821500318));
#21206=CARTESIAN_POINT('Ctrl Pts',(0.155008748383423,-0.0129756794247699,
2.03951590193954));
#21207=CARTESIAN_POINT('Ctrl Pts',(0.155123750300299,-0.0115434895315819,
2.03961886090853));
#21208=CARTESIAN_POINT('Ctrl Pts',(0.155188605578905,-0.0106361031847316,
2.03968429743742));
#21209=CARTESIAN_POINT('Ctrl Pts',(0.155488530187161,-0.00584982621565138,
2.04003059250408));
#21210=CARTESIAN_POINT('Ctrl Pts',(0.155586120954347,-0.00196404125308456,
2.04031569901426));
#21211=CARTESIAN_POINT('Ctrl Pts',(0.155355274765412,0.0167267659171037,
2.04170768804703));
#21212=CARTESIAN_POINT('Ctrl Pts',(0.153059088353099,0.0314295179295453,
2.04287482287781));
#21213=CARTESIAN_POINT('Ctrl Pts',(0.14742072770436,0.049826088298067,2.04434517027508));
#21214=CARTESIAN_POINT('Ctrl Pts',(0.145938587913794,0.0540134028880944,
2.04467970185316));
#21215=CARTESIAN_POINT('Ctrl Pts',(0.144032292147096,0.0587446816994504,
2.04505333563792));
#21216=CARTESIAN_POINT('Ctrl Pts',(0.143781530833612,0.0593557936702136,
2.04510150939863));
#21217=CARTESIAN_POINT('Ctrl Pts',(0.14340120603529,0.060266100583725,2.04517311984791));
#21218=CARTESIAN_POINT('Ctrl Pts',(0.143274586949353,0.060566504866436,
2.04519672720823));
#21219=CARTESIAN_POINT('Ctrl Pts',(0.143046172096064,0.0611036952659292,
2.04523889603256));
#21220=CARTESIAN_POINT('Ctrl Pts',(0.142944731838423,0.0613406273986872,
2.04525747852366));
#21221=CARTESIAN_POINT('Ctrl Pts',(0.14272376745547,0.0618532049718055,
2.04529764387293));
#21222=CARTESIAN_POINT('Ctrl Pts',(0.142604033824519,0.0621287558470869,
2.04531921373367));
#21223=CARTESIAN_POINT('Ctrl Pts',(0.142267403643778,0.0628973648551534,
2.04537932244987));
#21224=CARTESIAN_POINT('Ctrl Pts',(0.142048740364277,0.0633896523820206,
2.04541775557892));
#21225=CARTESIAN_POINT('Ctrl Pts',(0.140766338828488,0.0662368274106565,
2.04563970953407));
#21226=CARTESIAN_POINT('Ctrl Pts',(0.139646530920521,0.0685662304735617,
2.04582000247452));
#21227=CARTESIAN_POINT('Ctrl Pts',(0.131764316718353,0.0839675578371414,
2.04701050083198));
#21228=CARTESIAN_POINT('Ctrl Pts',(0.123233717778808,0.0960517886135503,
2.04794340532696));
#21229=CARTESIAN_POINT('Ctrl Pts',(0.111844816772437,0.10812053272599,2.04905822438335));
#21230=CARTESIAN_POINT('Ctrl Pts',(0.110534485942555,0.10945976276432,2.04918478278833));
#21231=CARTESIAN_POINT('Ctrl Pts',(0.10631357635864,0.113620673047407,2.04958787203721));
#21232=CARTESIAN_POINT('Ctrl Pts',(0.103316939964868,0.116352219073762,
2.04986742624574));
#21233=CARTESIAN_POINT('Ctrl Pts',(0.0995513782355839,0.119524406202461,
2.05021307914925));
#21234=CARTESIAN_POINT('Ctrl Pts',(0.0988808017010345,0.120079755107775,
2.05027442390733));
#21235=CARTESIAN_POINT('Ctrl Pts',(0.0977644013866712,0.120988627589063,
2.05037622992446));
#21236=CARTESIAN_POINT('Ctrl Pts',(0.0973212306734331,0.121345392285756,
2.05041656037475));
#21237=CARTESIAN_POINT('Ctrl Pts',(0.09651592023044,0.121986440216716,2.05048970362646));
#21238=CARTESIAN_POINT('Ctrl Pts',(0.0961544548621177,0.122271563564431,
2.05052248242505));
#21239=CARTESIAN_POINT('Ctrl Pts',(0.0953764311930852,0.122879683914416,
2.05059292882575));
#21240=CARTESIAN_POINT('Ctrl Pts',(0.0949594872700195,0.123202175755229,
2.05063061586382));
#21241=CARTESIAN_POINT('Ctrl Pts',(0.0938185158527525,0.124075445405476,
2.05073357539418));
#21242=CARTESIAN_POINT('Ctrl Pts',(0.0930912928756452,0.124621993222729,
2.05079901238577));
#21243=CARTESIAN_POINT('Ctrl Pts',(0.0892324214041446,0.127469522413765,
2.05114531433386));
#21244=CARTESIAN_POINT('Ctrl Pts',(0.0860204253786639,0.129658727421358,
2.05143042746388));
#21245=CARTESIAN_POINT('Ctrl Pts',(0.0701911626035577,0.139600304146264,
2.05282241939508));
#21246=CARTESIAN_POINT('Ctrl Pts',(0.0565927783511996,0.145643931207016,
2.05398954939497));
#21247=CARTESIAN_POINT('Ctrl Pts',(0.0380785072864503,0.150882527151424,
2.05545988892454));
#21248=CARTESIAN_POINT('Ctrl Pts',(0.0337566275612232,0.15190789615462,
2.0557944177489));
#21249=CARTESIAN_POINT('Ctrl Pts',(0.0287477011328726,0.15287186950894,
2.05616804883819));
#21250=CARTESIAN_POINT('Ctrl Pts',(0.0280982637039318,0.152992569840399,
2.05621622251342));
#21251=CARTESIAN_POINT('Ctrl Pts',(0.0271271835369517,0.153166656571019,
2.0562878328609));
#21252=CARTESIAN_POINT('Ctrl Pts',(0.0268061213803905,0.153223172639232,
2.05631144020418));
#21253=CARTESIAN_POINT('Ctrl Pts',(0.026230909977021,0.153322562880539,
2.05635360901016));
#21254=CARTESIAN_POINT('Ctrl Pts',(0.0259768308311037,0.15336581493275,
2.05637219149988));
#21255=CARTESIAN_POINT('Ctrl Pts',(0.0254263389596023,0.153458118225076,
2.05641235685994));
#21256=CARTESIAN_POINT('Ctrl Pts',(0.0251298920779448,0.153506942156976,
2.05643392673278));
#21257=CARTESIAN_POINT('Ctrl Pts',(0.0243368569494294,0.15363519387694,
2.05649147407643));
#21258=CARTESIAN_POINT('Ctrl Pts',(0.0238400161101844,0.153713073791213,
2.05652736551064));
#21259=CARTESIAN_POINT('Ctrl Pts',(0.0214381625993784,0.154077639172716,
2.05670012900236));
#21260=CARTESIAN_POINT('Ctrl Pts',(0.0195282040905837,0.154331344407538,
2.05683525062925));
#21261=CARTESIAN_POINT('Ctrl Pts',(0.0139052288375949,0.154972191310408,
2.05722774966487));
#21262=CARTESIAN_POINT('Ctrl Pts',(0.0101822269931536,0.155261270864672,
2.05748087595686));
#21263=CARTESIAN_POINT('Ctrl Pts',(-0.0064612414746064,0.155952229438248,
2.0585966452661));
#21264=CARTESIAN_POINT('Ctrl Pts',(-0.0193909164158658,0.154876907379754,
2.05942540401926));
#21265=CARTESIAN_POINT('Ctrl Pts',(-0.0365441258256776,0.151266403135661,
2.06061245465308));
#21266=CARTESIAN_POINT('Ctrl Pts',(-0.0410045087006287,0.150118690166007,
2.06092896682679));
#21267=CARTESIAN_POINT('Ctrl Pts',(-0.0462744250105808,0.148510277117373,
2.06131555053908));
#21268=CARTESIAN_POINT('Ctrl Pts',(-0.0471393986116943,0.148237990596818,
2.06137941314836));
#21269=CARTESIAN_POINT('Ctrl Pts',(-0.0485536802457966,0.147779156548596,
2.06148453169087));
#21270=CARTESIAN_POINT('Ctrl Pts',(-0.0491044220376613,0.147597068722404,
2.06152564140436));
#21271=CARTESIAN_POINT('Ctrl Pts',(-0.0500913224121013,0.147264641876094,
2.06159962874611));
#21272=CARTESIAN_POINT('Ctrl Pts',(-0.0505278573796326,0.147115434092107,
2.06163246878474));
#21273=CARTESIAN_POINT('Ctrl Pts',(-0.0514546152084873,0.146794056530645,
2.06170243226568));
#21274=CARTESIAN_POINT('Ctrl Pts',(-0.0519446509788728,0.146621368434372,
2.06173957251182));
#21275=CARTESIAN_POINT('Ctrl Pts',(-0.0532121363793322,0.146167556242658,
2.06183602088373));
#21276=CARTESIAN_POINT('Ctrl Pts',(-0.0539882175663857,0.145882686673219,
2.06189545267534));
#21277=CARTESIAN_POINT('Ctrl Pts',(-0.0576593850086255,0.144501835577831,
2.06217841341757));
#21278=CARTESIAN_POINT('Ctrl Pts',(-0.0605234069515121,0.143325851918236,
2.06240459257798));
#21279=CARTESIAN_POINT('Ctrl Pts',(-0.0634631113378447,0.142014968460715,
2.06264267791307));
#21280=CARTESIAN_POINT('Ctrl Pts',(-0.0635758997156846,0.141964512262164,
2.06265182176443));
#21281=CARTESIAN_POINT('Ctrl Pts',(-0.0636886258537358,0.141913922632217,
2.0626609697501));
#21282=CARTESIAN_POINT('Origin',(0.,0.,-0.129405622560373));
#21283=CARTESIAN_POINT('',(-0.0637081998868885,0.141956949220952,2.1466152095062));
#21284=CARTESIAN_POINT('',(-0.0636886258331689,0.141913922641447,2.13289020897179));
#21285=CARTESIAN_POINT('',(-0.0636886258329924,0.141913922641526,-0.129405622560373));
#21286=CARTESIAN_POINT('',(-0.155776797124186,5.07126225089676E-5,2.08940161016563));
#21287=CARTESIAN_POINT('Ctrl Pts',(-0.155783920579557,5.0990988608356E-5,
2.08940569613714));
#21288=CARTESIAN_POINT('Ctrl Pts',(-0.15557194890439,-0.0485975948926043,
2.09290471482211));
#21289=CARTESIAN_POINT('Ctrl Pts',(-0.104875675767394,-0.14913732793219,
2.100108637801));
#21290=CARTESIAN_POINT('Ctrl Pts',(0.0663275338242693,-0.17147627599867,
2.11101746507382));
#21291=CARTESIAN_POINT('Ctrl Pts',(0.180042327710072,-0.0372587603217594,
2.1221321779556));
#21292=CARTESIAN_POINT('Ctrl Pts',(0.128937250118005,0.131067312760423,
2.13324689083737));
#21293=CARTESIAN_POINT('Ctrl Pts',(0.00474514346942996,0.16656140244008,
2.14140790135424));
#21294=CARTESIAN_POINT('Ctrl Pts',(-0.054193003884981,0.146343230460563,
2.14586400757718));
#21295=CARTESIAN_POINT('Ctrl Pts',(-0.0637081998868965,0.141956949220948,
2.1466152095062));
#21296=CARTESIAN_POINT('Ctrl Pts',(-0.155549994370291,4.18497610693008E-5,
2.08927151745862));
#21297=CARTESIAN_POINT('Ctrl Pts',(-0.155549667422381,0.00125707164660975,
2.08918069722845));
#21298=CARTESIAN_POINT('Ctrl Pts',(-0.155535099726752,0.00247229902528903,
2.08909044289044));
#21299=CARTESIAN_POINT('Ctrl Pts',(-0.155487197254807,0.0044925239884509,
2.08894147324318));
#21300=CARTESIAN_POINT('Ctrl Pts',(-0.155461848926162,0.00529762994950571,
2.0888823885966));
#21301=CARTESIAN_POINT('Ctrl Pts',(-0.155416323820299,0.00645714646472965,
2.08879773638013));
#21302=CARTESIAN_POINT('Ctrl Pts',(-0.155401186846902,0.00681172397177014,
2.08877190946493));
#21303=CARTESIAN_POINT('Ctrl Pts',(-0.155372759727773,0.0074281052750826,
2.08872712019409));
#21304=CARTESIAN_POINT('Ctrl Pts',(-0.155360021166545,0.00768993103216972,
2.08870812825469));
#21305=CARTESIAN_POINT('Ctrl Pts',(-0.155334173705052,0.00819489257441228,
2.08867156647934));
#21306=CARTESIAN_POINT('Ctrl Pts',(-0.155321155649488,0.0084380326972423,
2.08865399161486));
#21307=CARTESIAN_POINT('Ctrl Pts',(-0.155294049603464,0.00892296575729506,
2.08861899979675));
#21308=CARTESIAN_POINT('Ctrl Pts',(-0.15527996775943,0.00916475722462516,
2.08860158251635));
#21309=CARTESIAN_POINT('Ctrl Pts',(-0.15524139928141,0.00980137405827636,
2.08855580070547));
#21310=CARTESIAN_POINT('Ctrl Pts',(-0.155215970947152,0.0101961441979767,
2.08852748855982));
#21311=CARTESIAN_POINT('Ctrl Pts',(-0.155121717123465,0.0115772612053776,
2.08842869499331));
#21312=CARTESIAN_POINT('Ctrl Pts',(-0.155044991624251,0.0125630731462905,
2.08835863795071));
#21313=CARTESIAN_POINT('Ctrl Pts',(-0.154797284725753,0.015396261847019,
2.08815844470379));
#21314=CARTESIAN_POINT('Ctrl Pts',(-0.154602641749619,0.0172414659348747,
2.08802946853944));
#21315=CARTESIAN_POINT('Ctrl Pts',(-0.152703259559245,0.0326069517581584,
2.08696386984621));
#21316=CARTESIAN_POINT('Ctrl Pts',(-0.149261473173037,0.0458541611473487,
2.08609517361747));
#21317=CARTESIAN_POINT('Ctrl Pts',(-0.14178908789031,0.064270062858469,
2.08476817861712));
#21318=CARTESIAN_POINT('Ctrl Pts',(-0.139095611857409,0.0699083838310649,
2.0843446765939));
#21319=CARTESIAN_POINT('Ctrl Pts',(-0.135359427929713,0.0766536622101196,
2.08380689327797));
#21320=CARTESIAN_POINT('Ctrl Pts',(-0.134629814998468,0.0779279880041747,
2.08370387195097));
#21321=CARTESIAN_POINT('Ctrl Pts',(-0.13355740004296,0.0797410223268643,
2.08355514833553));
#21322=CARTESIAN_POINT('Ctrl Pts',(-0.133229135137427,0.0802882760841422,
2.08350997155228));
#21323=CARTESIAN_POINT('Ctrl Pts',(-0.132653468078079,0.0812347244586077,
2.0834313352329));
#21324=CARTESIAN_POINT('Ctrl Pts',(-0.132407606395193,0.0816348504675293,
2.08339793225569));
#21325=CARTESIAN_POINT('Ctrl Pts',(-0.131930864100402,0.0824029020741967,
2.08333350578081));
#21326=CARTESIAN_POINT('Ctrl Pts',(-0.131700246588257,0.0827709865476328,
2.08330249219319));
#21327=CARTESIAN_POINT('Ctrl Pts',(-0.131090891279738,0.0837345734365021,
2.08322093832683));
#21328=CARTESIAN_POINT('Ctrl Pts',(-0.130709640908966,0.0843284667720374,
2.08317030541721));
#21329=CARTESIAN_POINT('Ctrl Pts',(-0.129366936103868,0.086389084987543,
2.08299332010484));
#21330=CARTESIAN_POINT('Ctrl Pts',(-0.128384761404647,0.0878420783737397,
2.0828661979083));
#21331=CARTESIAN_POINT('Ctrl Pts',(-0.120968342248256,0.0984235154968745,
2.081922713478));
#21332=CARTESIAN_POINT('Ctrl Pts',(-0.113593465199103,0.106850154702385,
2.08106913137985));
#21333=CARTESIAN_POINT('Ctrl Pts',(-0.0997225357481578,0.119626178768407,
2.07960761393809));
#21334=CARTESIAN_POINT('Ctrl Pts',(-0.093683674696811,0.124412175682198,
2.0790087202848));
#21335=CARTESIAN_POINT('Ctrl Pts',(-0.0856198574553641,0.129881632577302,
2.078272334449));
#21336=CARTESIAN_POINT('Ctrl Pts',(-0.0839019677366231,0.130997935995013,
2.07811885972282));
#21337=CARTESIAN_POINT('Ctrl Pts',(-0.0814287803910966,0.132536420486931,
2.07790319989135));
#21338=CARTESIAN_POINT('Ctrl Pts',(-0.0806913152668629,0.132986693914689,
2.07783954779368));
#21339=CARTESIAN_POINT('Ctrl Pts',(-0.079549918183988,0.133670605129244,
2.07774207794944));
#21340=CARTESIAN_POINT('Ctrl Pts',(-0.0791486373653939,0.13390860083106,
2.07770800760455));
#21341=CARTESIAN_POINT('Ctrl Pts',(-0.0784815167610447,0.134300217000108,
2.07765169995903));
#21342=CARTESIAN_POINT('Ctrl Pts',(-0.0782162857530849,0.134454860108218,
2.07762940028624));
#21343=CARTESIAN_POINT('Ctrl Pts',(-0.0777015914167277,0.13475291457641,
2.07758629720714));
#21344=CARTESIAN_POINT('Ctrl Pts',(-0.0774521848476985,0.134896420862542,
2.07756548786014));
#21345=CARTESIAN_POINT('Ctrl Pts',(-0.0769845126051193,0.135163790633825,
2.07752661377717));
#21346=CARTESIAN_POINT('Ctrl Pts',(-0.0767663479963998,0.135287816510729,
2.0775085390124));
#21347=CARTESIAN_POINT('Ctrl Pts',(-0.0762599613568219,0.135574076361242,
2.07746672205635));
#21348=CARTESIAN_POINT('Ctrl Pts',(-0.0759715215812175,0.135735919348897,
2.07744300507754));
#21349=CARTESIAN_POINT('Ctrl Pts',(-0.0750848941308739,0.136229692694543,
2.0773704078891));
#21350=CARTESIAN_POINT('Ctrl Pts',(-0.0744850200810121,0.136558604005474,
2.07732171573094));
#21351=CARTESIAN_POINT('Ctrl Pts',(-0.0705471595416633,0.138684066591484,
2.07700471927045));
#21352=CARTESIAN_POINT('Ctrl Pts',(-0.0671467602577074,0.140361969007692,
2.07674333761002));
#21353=CARTESIAN_POINT('Ctrl Pts',(-0.0636886254669799,0.141913922805787,
2.07648623881325));
#21354=CARTESIAN_POINT('',(-0.155549927754303,-0.000143266912413758,2.07557283338354));
#21355=CARTESIAN_POINT('Ctrl Pts',(-0.0636886258537358,0.141913922632217,
2.0626609697501));
#21356=CARTESIAN_POINT('Ctrl Pts',(-0.0685588818197047,0.139728232149738,
2.06305620223627));
#21357=CARTESIAN_POINT('Ctrl Pts',(-0.0733129487900478,0.137293486104077,
2.06345934329278));
#21358=CARTESIAN_POINT('Ctrl Pts',(-0.0840535706708943,0.131075666014453,
2.06440954394235));
#21359=CARTESIAN_POINT('Ctrl Pts',(-0.0899259662053769,0.127118625302212,
2.06495990848433));
#21360=CARTESIAN_POINT('Ctrl Pts',(-0.101448404136603,0.118155233102281,
2.06608987339327));
#21361=CARTESIAN_POINT('Ctrl Pts',(-0.107046118013571,0.113108788840649,
2.06666762379429));
#21362=CARTESIAN_POINT('Ctrl Pts',(-0.112744221473667,0.107168271130109,
2.06727110957734));
#21363=CARTESIAN_POINT('Ctrl Pts',(-0.11322796123183,0.106657051611768,
2.0673224704545));
#21364=CARTESIAN_POINT('Ctrl Pts',(-0.113936490514527,0.105898019483298,
2.06739786533489));
#21365=CARTESIAN_POINT('Ctrl Pts',(-0.114163967794944,0.105652746600751,
2.06742209704434));
#21366=CARTESIAN_POINT('Ctrl Pts',(-0.114565835517278,0.105216627311411,
2.0674649482667));
#21367=CARTESIAN_POINT('Ctrl Pts',(-0.114740542899674,0.105026078426222,
2.06748359167589));
#21368=CARTESIAN_POINT('Ctrl Pts',(-0.115113387008802,0.104617386087745,
2.06752340878616));
#21369=CARTESIAN_POINT('Ctrl Pts',(-0.115311378661106,0.104399115397032,
2.06754457157719));
#21370=CARTESIAN_POINT('Ctrl Pts',(-0.115716231343181,0.10395023939792,
2.06758788693527));
#21371=CARTESIAN_POINT('Ctrl Pts',(-0.115923026338546,0.103719575954074,
2.06761003458226));
#21372=CARTESIAN_POINT('Ctrl Pts',(-0.116865634850867,0.102661830138502,
2.06771109961662));
#21373=CARTESIAN_POINT('Ctrl Pts',(-0.117593320919101,0.101827496474286,
2.06778943505141));
#21374=CARTESIAN_POINT('Ctrl Pts',(-0.122812129741725,0.0957132676506731,
2.06835416885508));
#21375=CARTESIAN_POINT('Ctrl Pts',(-0.126955419458914,0.0901454231054279,
2.06881868869512));
#21376=CARTESIAN_POINT('Ctrl Pts',(-0.133764039990031,0.0795904912136084,
2.06965031120051));
#21377=CARTESIAN_POINT('Ctrl Pts',(-0.13655542240652,0.0746999502341629,
2.07001864757813));
#21378=CARTESIAN_POINT('Ctrl Pts',(-0.14332004812707,0.0611961442370621,
2.07101607980847));
#21379=CARTESIAN_POINT('Ctrl Pts',(-0.146780621986319,0.0523546662277312,
2.07165020659328));
#21380=CARTESIAN_POINT('Ctrl Pts',(-0.14973357521524,0.0421541275072256,
2.07239371170773));
#21381=CARTESIAN_POINT('Ctrl Pts',(-0.150039861562512,0.0410506252184793,
2.07247427047709));
#21382=CARTESIAN_POINT('Ctrl Pts',(-0.150484115587405,0.0393786175391289,
2.07259656625316));
#21383=CARTESIAN_POINT('Ctrl Pts',(-0.150631111899754,0.0388125324389542,
2.07263801175104));
#21384=CARTESIAN_POINT('Ctrl Pts',(-0.150888460275398,0.0377979937996901,
2.07271236869379));
#21385=CARTESIAN_POINT('Ctrl Pts',(-0.151000014855141,0.0373498498642456,
2.0727452410034));
#21386=CARTESIAN_POINT('Ctrl Pts',(-0.151232133818903,0.0363993285303847,
2.07281502470274));
#21387=CARTESIAN_POINT('Ctrl Pts',(-0.151352194035988,0.0358968350344211,
2.07285195184643));
#21388=CARTESIAN_POINT('Ctrl Pts',(-0.151591387263,0.0348731930303727,2.07292725423219));
#21389=CARTESIAN_POINT('Ctrl Pts',(-0.151710341314558,0.0343520102677563,
2.07296563467547));
#21390=CARTESIAN_POINT('Ctrl Pts',(-0.15199981373053,0.0330528877576283,
2.07306140929058));
#21391=CARTESIAN_POINT('Ctrl Pts',(-0.1521670469016,0.0322742398297517,
2.07311890752159));
#21392=CARTESIAN_POINT('Ctrl Pts',(-0.154480728380849,0.0210836902572564,
2.07394669144845));
#21393=CARTESIAN_POINT('Ctrl Pts',(-0.155559724762432,0.0104824683348447,
2.07475164736192));
#21394=CARTESIAN_POINT('Ctrl Pts',(-0.155549933968261,-0.000143326444609621,
2.07557282710847));
#21395=CARTESIAN_POINT('Ctrl Pts',(-0.155549934022329,-0.000143267753619253,
2.07557282257272));
#21396=CARTESIAN_POINT('Ctrl Pts',(-0.155539275057488,-0.0117160134402106,
2.0764671842731));
#21397=CARTESIAN_POINT('Ctrl Pts',(-0.154237185185774,-0.023252640275882,
2.07737557437259));
#21398=CARTESIAN_POINT('Ctrl Pts',(-0.151510568590532,-0.0352256410899354,
2.07828126275613));
#21399=CARTESIAN_POINT('Ctrl Pts',(-0.151349575070947,-0.0359110617876846,
2.07833296763677));
#21400=CARTESIAN_POINT('Ctrl Pts',(-0.151088863884984,-0.0369881195800717,
2.07841396545394));
#21401=CARTESIAN_POINT('Ctrl Pts',(-0.150992266990084,-0.037380490887096,
2.07844342042423));
#21402=CARTESIAN_POINT('Ctrl Pts',(-0.150806355107479,-0.0381231746751705,
2.07849906788549));
#21403=CARTESIAN_POINT('Ctrl Pts',(-0.150717345967773,-0.038473560008412,
2.078525276927));
#21404=CARTESIAN_POINT('Ctrl Pts',(-0.150561628668209,-0.0390777086561489,
2.0785703871));
#21405=CARTESIAN_POINT('Ctrl Pts',(-0.150495498861823,-0.0393316179150293,
2.07858932118145));
#21406=CARTESIAN_POINT('Ctrl Pts',(-0.150365886775339,-0.039824158068148,
2.07862600085319));
#21407=CARTESIAN_POINT('Ctrl Pts',(-0.150302478798175,-0.0400628049570566,
2.07864375074015));
#21408=CARTESIAN_POINT('Ctrl Pts',(-0.150129596860551,-0.0407072884352145,
2.0786916280179));
#21409=CARTESIAN_POINT('Ctrl Pts',(-0.150019044614443,-0.0411128380111044,
2.07872169361249));
#21410=CARTESIAN_POINT('Ctrl Pts',(-0.149601090166072,-0.0426219261966321,
2.07883335744952));
#21411=CARTESIAN_POINT('Ctrl Pts',(-0.149283134209527,-0.0437225435885582,
2.07891437154914));
#21412=CARTESIAN_POINT('Ctrl Pts',(-0.146088489028586,-0.0543395994523739,
2.07969265742224));
#21413=CARTESIAN_POINT('Ctrl Pts',(-0.142317370091986,-0.0635646861446651,
2.08034470014211));
#21414=CARTESIAN_POINT('Ctrl Pts',(-0.135336273678805,-0.076847281847116,
2.08133224390421));
#21415=CARTESIAN_POINT('Ctrl Pts',(-0.132764773239527,-0.0812091379441312,
2.0816651354955));
#21416=CARTESIAN_POINT('Ctrl Pts',(-0.126501829414894,-0.090737603622008,
2.0824254833909));
#21417=CARTESIAN_POINT('Ctrl Pts',(-0.122697859816682,-0.0958188150260091,
2.08285494143391));
#21418=CARTESIAN_POINT('Ctrl Pts',(-0.117582891959365,-0.101845526724964,
2.08340551780044));
#21419=CARTESIAN_POINT('Ctrl Pts',(-0.116553137326716,-0.103022393990375,
2.08351512443418));
#21420=CARTESIAN_POINT('Ctrl Pts',(-0.11516323704072,-0.104563344426577,
2.08366155945504));
#21421=CARTESIAN_POINT('Ctrl Pts',(-0.114818758889329,-0.104941492076381,
2.08369773297364));
#21422=CARTESIAN_POINT('Ctrl Pts',(-0.114133435236436,-0.105686385761821,
2.08376946820248));
#21423=CARTESIAN_POINT('Ctrl Pts',(-0.113792671706578,-0.106053199053403,
2.08380502618964));
#21424=CARTESIAN_POINT('Ctrl Pts',(-0.113131290684871,-0.106758282050102,
2.08387383096205));
#21425=CARTESIAN_POINT('Ctrl Pts',(-0.112810911656775,-0.107096768955875,
2.08390706730585));
#21426=CARTESIAN_POINT('Ctrl Pts',(-0.112070095386993,-0.107872443742654,
2.08398370995093));
#21427=CARTESIAN_POINT('Ctrl Pts',(-0.111648614895726,-0.108308620024616,
2.08402716114621));
#21428=CARTESIAN_POINT('Ctrl Pts',(-0.110513822882038,-0.109469316190258,
2.08414374780094));
#21429=CARTESIAN_POINT('Ctrl Pts',(-0.109795951459124,-0.110189315212772,
2.08421708223764));
#21430=CARTESIAN_POINT('Ctrl Pts',(-0.103796682457949,-0.116089529518788,
2.08482661157651));
#21431=CARTESIAN_POINT('Ctrl Pts',(-0.0981598405173183,-0.120893107614842,
2.08537893165665));
#21432=CARTESIAN_POINT('Ctrl Pts',(-0.0838711187023698,-0.131409576367771,
2.08673283586956));
#21433=CARTESIAN_POINT('Ctrl Pts',(-0.0749483327620099,-0.136695163080771,
2.08754373776629));
#21434=CARTESIAN_POINT('Ctrl Pts',(-0.0624525077612218,-0.142503632708605,
2.08860014208909));
#21435=CARTESIAN_POINT('Ctrl Pts',(-0.0592903211807623,-0.14384805334556,
2.08886100106461));
#21436=CARTESIAN_POINT('Ctrl Pts',(-0.0543550133917548,-0.145755888490614,
2.08925580564902));
#21437=CARTESIAN_POINT('Ctrl Pts',(-0.0526120985105431,-0.146394038251702,
2.08939292288103));
#21438=CARTESIAN_POINT('Ctrl Pts',(-0.0504005275819003,-0.147159178205275,
2.08956366271858));
#21439=CARTESIAN_POINT('Ctrl Pts',(-0.0499422327641749,-0.147315343104484,
2.08959887022755));
#21440=CARTESIAN_POINT('Ctrl Pts',(-0.0492076949578372,-0.147561816575549,
2.08965501292125));
#21441=CARTESIAN_POINT('Ctrl Pts',(-0.0489319202078071,-0.14765349349984,
2.08967602670699));
#21442=CARTESIAN_POINT('Ctrl Pts',(-0.0484095487962619,-0.147825523334772,
2.089715707014));
#21443=CARTESIAN_POINT('Ctrl Pts',(-0.0481630112734116,-0.147906031351704,
2.08973438208562));
#21444=CARTESIAN_POINT('Ctrl Pts',(-0.047596787497356,-0.148089368586787,
2.08977715474778));
#21445=CARTESIAN_POINT('Ctrl Pts',(-0.0472769688221497,-0.148191779438817,
2.08980122763603));
#21446=CARTESIAN_POINT('Ctrl Pts',(-0.0464226934864937,-0.148462284510505,
2.08986530566505));
#21447=CARTESIAN_POINT('Ctrl Pts',(-0.0458876493650725,-0.148628530416703,
2.08990520555735));
#21448=CARTESIAN_POINT('Ctrl Pts',(-0.0420192689448587,-0.149807611241837,
2.09019208323064));
#21449=CARTESIAN_POINT('Ctrl Pts',(-0.0386533127484973,-0.150711199165969,
2.09043315313171));
#21450=CARTESIAN_POINT('Ctrl Pts',(-0.0351738451268169,-0.151520991477027,
2.09067637808321));
#21451=CARTESIAN_POINT('Ctrl Pts',(-0.0350881453331679,-0.151540860154363,
2.09068236506112));
#21452=CARTESIAN_POINT('Ctrl Pts',(-0.0330029247003192,-0.152022434911937,
2.09082794965413));
#21453=CARTESIAN_POINT('Ctrl Pts',(-0.0309944023124441,-0.15244461751603,
2.09096619755381));
#21454=CARTESIAN_POINT('Ctrl Pts',(-0.0178296593580188,-0.154940829624849,
2.09186285370095));
#21455=CARTESIAN_POINT('Ctrl Pts',(-0.00648343222484846,-0.155828551932417,
2.09259400605833));
#21456=CARTESIAN_POINT('Ctrl Pts',(0.00883310285273221,-0.155349895274327,
2.09362243048698));
#21457=CARTESIAN_POINT('Ctrl Pts',(0.0128009852858482,-0.155073351939004,
2.09389232126612));
#21458=CARTESIAN_POINT('Ctrl Pts',(0.0192096306625509,-0.154379062869907,
2.09433708239329));
#21459=CARTESIAN_POINT('Ctrl Pts',(0.0216587621687042,-0.154054541628188,
2.09450915592145));
#21460=CARTESIAN_POINT('Ctrl Pts',(0.024853337552565,-0.15355356430304,
2.09473681807388));
#21461=CARTESIAN_POINT('Ctrl Pts',(0.025606767685335,-0.153429719771189,
2.09479074619171));
#21462=CARTESIAN_POINT('Ctrl Pts',(0.0267863769709881,-0.153226891718253,
2.09487556019163));
#21463=CARTESIAN_POINT('Ctrl Pts',(0.0272131975532774,-0.153151664074773,
2.0949063270881));
#21464=CARTESIAN_POINT('Ctrl Pts',(0.0280927244976935,-0.152992853617563,
2.09496989158027));
#21465=CARTESIAN_POINT('Ctrl Pts',(0.028545384832841,-0.152909042976954,
2.09500269610817));
#21466=CARTESIAN_POINT('Ctrl Pts',(0.0295562198156295,-0.15271724064329,
2.09507615701763));
#21467=CARTESIAN_POINT('Ctrl Pts',(0.0301141854047978,-0.152608196179066,
2.0951168464701));
#21468=CARTESIAN_POINT('Ctrl Pts',(0.0315238279156536,-0.152324674836719,
2.09522000556244));
#21469=CARTESIAN_POINT('Ctrl Pts',(0.0323746534130341,-0.152146114146601,
2.09528260442757));
#21470=CARTESIAN_POINT('Ctrl Pts',(0.0371649183859182,-0.151098792922337,
2.09563697986784));
#21471=CARTESIAN_POINT('Ctrl Pts',(0.0410705340794318,-0.150084249816918,
2.09593337227538));
#21472=CARTESIAN_POINT('Ctrl Pts',(0.046742365216269,-0.148372940897499,
2.0963753493966));
#21473=CARTESIAN_POINT('Ctrl Pts',(0.0485425551349078,-0.147793768902848,
2.09651736623511));
#21474=CARTESIAN_POINT('Ctrl Pts',(0.0642483240589407,-0.142422881267746,
2.09777152746878));
#21475=CARTESIAN_POINT('Ctrl Pts',(0.0774175463040418,-0.135715032924409,
2.0989378469886));
#21476=CARTESIAN_POINT('Ctrl Pts',(0.0915746681914158,-0.125764217306641,
2.10023969192907));
#21477=CARTESIAN_POINT('Ctrl Pts',(0.093663488237941,-0.124216389181719,
2.1004328880198));
#21478=CARTESIAN_POINT('Ctrl Pts',(0.0961380302185033,-0.122284801965177,
2.10066221003611));
#21479=CARTESIAN_POINT('Ctrl Pts',(0.0965616474906106,-0.121950571556939,
2.10070148388226));
#21480=CARTESIAN_POINT('Ctrl Pts',(0.097218574685019,-0.121426692369834,
2.10076240225947));
#21481=CARTESIAN_POINT('Ctrl Pts',(0.097453082825586,-0.121238564556163,
2.10078415158408));
#21482=CARTESIAN_POINT('Ctrl Pts',(0.0978876018901263,-0.120887908052338,
2.10082445379575));
#21483=CARTESIAN_POINT('Ctrl Pts',(0.0980877523498004,-0.120725563812675,
2.10084301892751));
#21484=CARTESIAN_POINT('Ctrl Pts',(0.0985399596028237,-0.120356906550316,
2.10088496687752));
#21485=CARTESIAN_POINT('Ctrl Pts',(0.0987917719262479,-0.120150299199908,
2.10090832810862));
#21486=CARTESIAN_POINT('Ctrl Pts',(0.0995512130847963,-0.119523190112429,
2.10097879728187));
#21487=CARTESIAN_POINT('Ctrl Pts',(0.100056828717749,-0.119100243784874,
2.10102573278743));
#21488=CARTESIAN_POINT('Ctrl Pts',(0.103915013534657,-0.115830969734336,
2.10138416708048));
#21489=CARTESIAN_POINT('Ctrl Pts',(0.107148590900619,-0.112846497817881,
2.10168625142364));
#21490=CARTESIAN_POINT('Ctrl Pts',(0.120645024503983,-0.0992857331299244,
2.10297766192179));
#21491=CARTESIAN_POINT('Ctrl Pts',(0.129502144886547,-0.0874192325556558,
2.10391456027543));
#21492=CARTESIAN_POINT('Ctrl Pts',(0.138467021982286,-0.0709829732157343,
2.10518925654987));
#21493=CARTESIAN_POINT('Ctrl Pts',(0.140240711343387,-0.0674109549754019,
2.10546450603147));
#21494=CARTESIAN_POINT('Ctrl Pts',(0.142251038715252,-0.0629387410611146,
2.10580899008777));
#21495=CARTESIAN_POINT('Ctrl Pts',(0.142619542019864,-0.0620991892997372,
2.1058736503358));
#21496=CARTESIAN_POINT('Ctrl Pts',(0.143188794075535,-0.0607704801661151,
2.10597599418996));
#21497=CARTESIAN_POINT('Ctrl Pts',(0.143394512078053,-0.0602834629211887,
2.10601350874638));
#21498=CARTESIAN_POINT('Ctrl Pts',(0.143774662092217,-0.0593705386413041,
2.10608383910188));
#21499=CARTESIAN_POINT('Ctrl Pts',(0.143949694876233,-0.0589448865888338,
2.10611663415434));
#21500=CARTESIAN_POINT('Ctrl Pts',(0.144336065167541,-0.0579933103904562,
2.10618996094575));
#21501=CARTESIAN_POINT('Ctrl Pts',(0.144546421373407,-0.0574669975769691,
2.10623052519959));
#21502=CARTESIAN_POINT('Ctrl Pts',(0.145070086163024,-0.0561357170685721,
2.10633315577793));
#21503=CARTESIAN_POINT('Ctrl Pts',(0.145379571249598,-0.0553292764951944,
2.10639534902532));
#21504=CARTESIAN_POINT('Ctrl Pts',(0.147067941684211,-0.0508178257031439,
2.10674344913227));
#21505=CARTESIAN_POINT('Ctrl Pts',(0.148311788598635,-0.0470642007978736,
2.1070337827555));
#21506=CARTESIAN_POINT('Ctrl Pts',(0.149957472320738,-0.0413813395434992,
2.10747486944115));
#21507=CARTESIAN_POINT('Ctrl Pts',(0.15046791368721,-0.0394849989686747,
2.10762229655842));
#21508=CARTESIAN_POINT('Ctrl Pts',(0.1544841234355,-0.0233534706240894,
2.10887821628386));
#21509=CARTESIAN_POINT('Ctrl Pts',(0.155996648345524,-0.00870038777706942,
2.11004050690006));
#21510=CARTESIAN_POINT('Ctrl Pts',(0.15533463394952,0.00860376758607486,
2.11134407375037));
#21511=CARTESIAN_POINT('Ctrl Pts',(0.155164850128709,0.0112581041147174,
2.11154181553789));
#21512=CARTESIAN_POINT('Ctrl Pts',(0.154878510889393,0.0144479896801079,
2.1117757994496));
#21513=CARTESIAN_POINT('Ctrl Pts',(0.154827113627625,0.0149887441273677,
2.11181533768871));
#21514=CARTESIAN_POINT('Ctrl Pts',(0.154742791440628,0.0158291456724525,
2.11187657616866));
#21515=CARTESIAN_POINT('Ctrl Pts',(0.154711827075869,0.0161289777301707,
2.11189838295658));
#21516=CARTESIAN_POINT('Ctrl Pts',(0.154652779836225,0.0166849203565997,
2.11193873751695));
#21517=CARTESIAN_POINT('Ctrl Pts',(0.154624932493924,0.0169410487141398,
2.11195729781535));
#21518=CARTESIAN_POINT('Ctrl Pts',(0.154560553731085,0.0175197928359585,
2.11199916624363));
#21519=CARTESIAN_POINT('Ctrl Pts',(0.154523648616741,0.0178423634662825,
2.11202245313307));
#21520=CARTESIAN_POINT('Ctrl Pts',(0.154411805251766,0.0187935539596294,
2.11209098276562));
#21521=CARTESIAN_POINT('Ctrl Pts',(0.15433403787289,0.0194218449727524,
2.11213607038085));
#21522=CARTESIAN_POINT('Ctrl Pts',(0.153746969808654,0.0239384645705222,
2.11245902428026));
#21523=CARTESIAN_POINT('Ctrl Pts',(0.153094570344407,0.0278071926000845,
2.11272941991567));
#21524=CARTESIAN_POINT('Ctrl Pts',(0.152025546843706,0.0329516274772899,
2.11308561441976));
#21525=CARTESIAN_POINT('Ctrl Pts',(0.151737803875257,0.0342522363124642,
2.11317537428777));
#21526=CARTESIAN_POINT('Ctrl Pts',(0.15050603824148,0.0394993694956073,
2.11353688721891));
#21527=CARTESIAN_POINT('Ctrl Pts',(0.149424433351358,0.0434120849051451,
2.11380508662157));
#21528=CARTESIAN_POINT('Ctrl Pts',(0.145327975164245,0.0562522256601415,
2.1146931901613));
#21529=CARTESIAN_POINT('Ctrl Pts',(0.141655936298709,0.0649469992922441,
2.11530892160966));
#21530=CARTESIAN_POINT('Ctrl Pts',(0.135168842958949,0.0770983696808988,
2.11624404231416));
#21531=CARTESIAN_POINT('Ctrl Pts',(0.132957227833877,0.0808526082722024,
2.11654412421923));
#21532=CARTESIAN_POINT('Ctrl Pts',(0.130079807788597,0.085299074325434,
2.11691608163433));
#21533=CARTESIAN_POINT('Ctrl Pts',(0.129561276838548,0.0860846324820536,
2.11698244436873));
#21534=CARTESIAN_POINT('Ctrl Pts',(0.128737432506259,0.0873084254999529,
2.11708687656539));
#21535=CARTESIAN_POINT('Ctrl Pts',(0.128436930695856,0.0877498861086389,
2.11712476507561));
#21536=CARTESIAN_POINT('Ctrl Pts',(0.127899658760918,0.0885305081531673,
2.11719215241497));
#21537=CARTESIAN_POINT('Ctrl Pts',(0.127663796604884,0.0888702909603656,
2.1172216165997));
#21538=CARTESIAN_POINT('Ctrl Pts',(0.127116674566962,0.0896518017262265,
2.11728969382767));
#21539=CARTESIAN_POINT('Ctrl Pts',(0.126804464031219,0.0900928542885824,
2.11732834291841));
#21540=CARTESIAN_POINT('Ctrl Pts',(0.125940396610847,0.0913001129030285,
2.11743477199929));
#21541=CARTESIAN_POINT('Ctrl Pts',(0.125383859158127,0.0920629236128803,
2.11750273140506));
#21542=CARTESIAN_POINT('Ctrl Pts',(0.122490277179034,0.0959540653074933,
2.11785312865737));
#21543=CARTESIAN_POINT('Ctrl Pts',(0.120043179152849,0.0989983875217004,
2.11813983605939));
#21544=CARTESIAN_POINT('Ctrl Pts',(0.116168371410419,0.103463731106798,
2.11858043259816));
#21545=CARTESIAN_POINT('Ctrl Pts',(0.114823207912509,0.104954582940407,
2.11873114189461));
#21546=CARTESIAN_POINT('Ctrl Pts',(0.103437996811253,0.117091971235299,
2.11998829786051));
#21547=CARTESIAN_POINT('Ctrl Pts',(0.0919720869577657,0.126297292122009,
2.12114832932706));
#21548=CARTESIAN_POINT('Ctrl Pts',(0.0770740535487226,0.135139359868302,
2.12245291008323));
#21549=CARTESIAN_POINT('Ctrl Pts',(0.0747224595322871,0.136453701831866,
2.12265324684281));
#21550=CARTESIAN_POINT('Ctrl Pts',(0.0718550858329579,0.13795994479323,
2.12288988734704));
#21551=CARTESIAN_POINT('Ctrl Pts',(0.0713711006441542,0.138210946542513,
2.12292957323021));
#21552=CARTESIAN_POINT('Ctrl Pts',(0.0706171024967069,0.138596964087064,
2.12299099040557));
#21553=CARTESIAN_POINT('Ctrl Pts',(0.0703480058979274,0.138733743875096,
2.12301282922946));
#21554=CARTESIAN_POINT('Ctrl Pts',(0.0698485323621824,0.138985795623522,
2.1230532131736));
#21555=CARTESIAN_POINT('Ctrl Pts',(0.0696182694072932,0.139101277581931,
2.12307177097624));
#21556=CARTESIAN_POINT('Ctrl Pts',(0.0690976519170733,0.139360762186724,
2.12311359597568));
#21557=CARTESIAN_POINT('Ctrl Pts',(0.0688071341872435,0.139504429420173,
2.12313684212222));
#21558=CARTESIAN_POINT('Ctrl Pts',(0.0679502213662177,0.13992486309541,
2.12320514115709));
#21559=CARTESIAN_POINT('Ctrl Pts',(0.0673825811031899,0.14019910019741,
2.12325004047087));
#21560=CARTESIAN_POINT('Ctrl Pts',(0.0633337264451739,0.142124902623486,
2.12356797265133));
#21561=CARTESIAN_POINT('Ctrl Pts',(0.0597935064867675,0.143650241009157,
2.12383379668596));
#21562=CARTESIAN_POINT('Ctrl Pts',(0.04460299243111,0.149536135184221,2.12493888899866));
#21563=CARTESIAN_POINT('Ctrl Pts',(0.0325084024869392,0.15262284961798,
2.12573589926957));
#21564=CARTESIAN_POINT('Ctrl Pts',(0.015809608591236,0.154807096117142,
2.12686198254668));
#21565=CARTESIAN_POINT('Ctrl Pts',(0.0114227787029252,0.155192447419367,
2.127159727511));
#21566=CARTESIAN_POINT('Ctrl Pts',(0.00436006533228581,0.155511777362201,
2.12764664434128));
#21567=CARTESIAN_POINT('Ctrl Pts',(0.00169183895864124,0.155563682337055,
2.12783230286204));
#21568=CARTESIAN_POINT('Ctrl Pts',(-0.00177884502506953,0.155541899061895,
2.1280765912983));
#21569=CARTESIAN_POINT('Ctrl Pts',(-0.00258135610695362,0.155530650389993,
2.12813327044301));
#21570=CARTESIAN_POINT('Ctrl Pts',(-0.00388701311032124,0.155502241276432,
2.12822581573446));
#21571=CARTESIAN_POINT('Ctrl Pts',(-0.00439023374664659,0.155488847669876,
2.12826156399668));
#21572=CARTESIAN_POINT('Ctrl Pts',(-0.00535825764755493,0.155458379976122,
2.12833048916073));
#21573=CARTESIAN_POINT('Ctrl Pts',(-0.00582306747507281,0.155441663354329,
2.12836365452934));
#21574=CARTESIAN_POINT('Ctrl Pts',(-0.00688768696392738,0.155398593084937,
2.12843978180993));
#21575=CARTESIAN_POINT('Ctrl Pts',(-0.00748742974726766,0.155370851003539,
2.12848278665164));
#21576=CARTESIAN_POINT('Ctrl Pts',(-0.00908132583029788,0.155287872695047,
2.12859740292566));
#21577=CARTESIAN_POINT('Ctrl Pts',(-0.0100751204578383,0.155226562633507,
2.12866920290423));
#21578=CARTESIAN_POINT('Ctrl Pts',(-0.0175925317763295,0.154690298224357,
2.12921495981637));
#21579=CARTESIAN_POINT('Ctrl Pts',(-0.0240799891881967,0.15381390346561,
2.12970141250499));
#21580=CARTESIAN_POINT('Ctrl Pts',(-0.0419292207722073,0.150245713766086,
2.13108376194071));
#21581=CARTESIAN_POINT('Ctrl Pts',(-0.0530638077777302,0.146682165595228,
2.13199949648016));
#21582=CARTESIAN_POINT('Ctrl Pts',(-0.0636886258331765,0.141913922641444,
2.1328902089718));
#21583=CARTESIAN_POINT('Origin',(0.,0.,-0.129405622560373));
#21584=CARTESIAN_POINT('',(-0.0636886258329906,0.141913922641527,2.21660530308003));
#21585=CARTESIAN_POINT('',(-0.0636886613526595,0.141913906700881,2.20284414165342));
#21586=CARTESIAN_POINT('',(-0.0636886258329924,0.141913922641526,-0.129405622560373));
#21587=CARTESIAN_POINT('',(-0.15554996116255,0.000109919649464305,2.15940562256037));
#21588=CARTESIAN_POINT('Ctrl Pts',(-0.15554996116255,0.000109919649464305,
2.15940562256037));
#21589=CARTESIAN_POINT('Ctrl Pts',(-0.155557267423461,-0.0102293473203203,
2.16014353394896));
#21590=CARTESIAN_POINT('Ctrl Pts',(-0.154529367184467,-0.0205766677469432,
2.16088144533755));
#21591=CARTESIAN_POINT('Ctrl Pts',(-0.152487668180623,-0.0307134099838537,
2.16161935672614));
#21592=CARTESIAN_POINT('Ctrl Pts',(-0.150445829414615,-0.0408508461198288,
2.16235731862761));
#21593=CARTESIAN_POINT('Ctrl Pts',(-0.147390270093583,-0.050776782287812,
2.16309528052908));
#21594=CARTESIAN_POINT('Ctrl Pts',(-0.143393161912447,-0.060284356318624,
2.16383324243055));
#21595=CARTESIAN_POINT('Ctrl Pts',(-0.139385782328791,-0.0698163620424093,
2.16457310067893));
#21596=CARTESIAN_POINT('Ctrl Pts',(-0.134432451496566,-0.0789270447473818,
2.1653129589273));
#21597=CARTESIAN_POINT('Ctrl Pts',(-0.128651965870623,-0.0874326836922218,
2.16605281717568));
#21598=CARTESIAN_POINT('Ctrl Pts',(-0.12725028813426,-0.0894951686656319,
2.16623222127802));
#21599=CARTESIAN_POINT('Ctrl Pts',(-0.125800167594638,-0.091522222466176,
2.16641162538036));
#21600=CARTESIAN_POINT('Ctrl Pts',(-0.124303651570102,-0.0935115217838889,
2.1665910294827));
#21601=CARTESIAN_POINT('Ctrl Pts',(-0.118153313802634,-0.101687085910121,
2.16732833921288));
#21602=CARTESIAN_POINT('Ctrl Pts',(-0.111169892400885,-0.109283920973333,
2.16806564894306));
#21603=CARTESIAN_POINT('Ctrl Pts',(-0.103486335854972,-0.116130877854737,
2.16880295867324));
#21604=CARTESIAN_POINT('Ctrl Pts',(-0.0957549579473897,-0.123020449220645,
2.16954485731418));
#21605=CARTESIAN_POINT('Ctrl Pts',(-0.0873152795860456,-0.129150017855905,
2.17028675595512));
#21606=CARTESIAN_POINT('Ctrl Pts',(-0.0783421409037998,-0.134381216911476,
2.17102865459605));
#21607=CARTESIAN_POINT('Ctrl Pts',(-0.0694450195957192,-0.139568099030686,
2.17176426812443));
#21608=CARTESIAN_POINT('Ctrl Pts',(-0.0600242657486143,-0.143871321381819,
2.17249988165282));
#21609=CARTESIAN_POINT('Ctrl Pts',(-0.0502782126981477,-0.147200216806497,
2.1732354951812));
#21610=CARTESIAN_POINT('Ctrl Pts',(-0.0404072536243069,-0.150571775562431,
2.17398053637841));
#21611=CARTESIAN_POINT('Ctrl Pts',(-0.0302035006824242,-0.152943492630249,
2.17472557757562));
#21612=CARTESIAN_POINT('Ctrl Pts',(-0.0198888207273883,-0.154273255329865,
2.17547061877284));
#21613=CARTESIAN_POINT('Ctrl Pts',(-0.00957414077235236,-0.155603018029482,
2.17621565997005));
#21614=CARTESIAN_POINT('Ctrl Pts',(0.000850485147299905,-0.155890834447186,
2.17696070116726));
#21615=CARTESIAN_POINT('Ctrl Pts',(0.011161779685702,-0.155149016027327,
2.17770574236447));
#21616=CARTESIAN_POINT('Ctrl Pts',(0.0213660702183622,-0.154414895723565,
2.17844305200167));
#21617=CARTESIAN_POINT('Ctrl Pts',(0.0315358720632552,-0.152666987619122,
2.17918036163887));
#21618=CARTESIAN_POINT('Ctrl Pts',(0.0414552909564462,-0.149924185346182,
2.17991767127607));
#21619=CARTESIAN_POINT('Ctrl Pts',(0.0514364484715978,-0.147164311827995,
2.18065956994025));
#21620=CARTESIAN_POINT('Ctrl Pts',(0.0611631441371558,-0.143397193035534,
2.18140146860444));
#21621=CARTESIAN_POINT('Ctrl Pts',(0.0704243105148482,-0.138694697045375,
2.18214336726862));
#21622=CARTESIAN_POINT('Ctrl Pts',(0.0796070180183042,-0.134032039724173,
2.18287898070569));
#21623=CARTESIAN_POINT('Ctrl Pts',(0.0883312262223324,-0.128450239567257,
2.18361459414276));
#21624=CARTESIAN_POINT('Ctrl Pts',(0.0964132053605308,-0.122066769974912,
2.18435020757983));
#21625=CARTESIAN_POINT('Ctrl Pts',(0.104598765547872,-0.115601487937096,
2.18509524885757));
#21626=CARTESIAN_POINT('Ctrl Pts',(0.112124722996507,-0.108314403050016,
2.18584029013531));
#21627=CARTESIAN_POINT('Ctrl Pts',(0.118835381745117,-0.100369091584473,
2.18658533141304));
#21628=CARTESIAN_POINT('Ctrl Pts',(0.125546040493727,-0.0924237801189298,
2.18733037269078));
#21629=CARTESIAN_POINT('Ctrl Pts',(0.131440875338134,-0.0838210707394638,
2.18807541396852));
#21630=CARTESIAN_POINT('Ctrl Pts',(0.136409152710375,-0.0747552376548803,
2.18882045524625));
#21631=CARTESIAN_POINT('Ctrl Pts',(0.141325872363875,-0.0657834841953472,
2.18955776494506));
#21632=CARTESIAN_POINT('Ctrl Pts',(0.145372103737932,-0.0562909566865397,
2.19029507464387));
#21633=CARTESIAN_POINT('Ctrl Pts',(0.148446647289986,-0.0464692953288783,
2.19103238434268));
#21634=CARTESIAN_POINT('Ctrl Pts',(0.151540326527584,-0.0365865048247006,
2.19177428299146));
#21635=CARTESIAN_POINT('Ctrl Pts',(0.153649728849893,-0.0263713099442799,
2.19251618164024));
#21636=CARTESIAN_POINT('Ctrl Pts',(0.154720781389452,-0.0160400220148674,
2.19325808028901));
#21637=CARTESIAN_POINT('Ctrl Pts',(0.155782760276811,-0.00579625781560798,
2.19399369378365));
#21638=CARTESIAN_POINT('Ctrl Pts',(0.155823841493419,0.004560702577827,
2.19472930727828));
#21639=CARTESIAN_POINT('Ctrl Pts',(0.154843094330516,0.0148127863061284,
2.19546492077292));
#21640=CARTESIAN_POINT('Ctrl Pts',(0.153849777767092,0.0251962622539743,
2.19620996199877));
#21641=CARTESIAN_POINT('Ctrl Pts',(0.15180829570891,0.0354711820272215,
2.19695500322462));
#21642=CARTESIAN_POINT('Ctrl Pts',(0.148771655133367,0.0454180264749404,
2.19770004445047));
#21643=CARTESIAN_POINT('Ctrl Pts',(0.145735014557825,0.0553648709226579,
2.19844508567632));
#21644=CARTESIAN_POINT('Ctrl Pts',(0.141703626904404,0.0649827494045178,
2.19919012690217));
#21645=CARTESIAN_POINT('Ctrl Pts',(0.136780673539898,0.074073273493021,
2.19993516812803));
#21646=CARTESIAN_POINT('Ctrl Pts',(0.131908805826588,0.083069464909977,
2.20067247803624));
#21647=CARTESIAN_POINT('Ctrl Pts',(0.126127338894467,0.0916166731077121,
2.20140978794444));
#21648=CARTESIAN_POINT('Ctrl Pts',(0.119542411262813,0.0995259484228733,
2.20214709785265));
#21649=CARTESIAN_POINT('Ctrl Pts',(0.112916501976755,0.107484447542105,
2.20288899644908));
#21650=CARTESIAN_POINT('Ctrl Pts',(0.105477557918341,0.11479621038619,2.20363089504551));
#21651=CARTESIAN_POINT('Ctrl Pts',(0.0973780017415188,0.121298504841687,
2.20437279364194));
#21652=CARTESIAN_POINT('Ctrl Pts',(0.0893470598209456,0.127745716019997,
2.20510840734827));
#21653=CARTESIAN_POINT('Ctrl Pts',(0.0806674030898069,0.133396550631897,
2.20584402105461));
#21654=CARTESIAN_POINT('Ctrl Pts',(0.0715217520374606,0.138131971264773,
2.20657963476094));
#21655=CARTESIAN_POINT('Ctrl Pts',(0.0622588939281335,0.142928079180902,
2.20732467580242));
#21656=CARTESIAN_POINT('Ctrl Pts',(0.0525188515825804,0.146784650332905,
2.20806971684389));
#21657=CARTESIAN_POINT('Ctrl Pts',(0.0425148093650004,0.149627181637087,
2.20881475788537));
#21658=CARTESIAN_POINT('Ctrl Pts',(0.0325107671474189,0.152469712941268,
2.20955979892685));
#21659=CARTESIAN_POINT('Ctrl Pts',(0.0222436964848991,0.154298067118003,
2.21030483996833));
#21660=CARTESIAN_POINT('Ctrl Pts',(0.0119362359789071,0.155091356208706,
2.21104988100981));
#21661=CARTESIAN_POINT('Ctrl Pts',(0.00173574192027406,0.155876412882151,
2.21178719033179));
#21662=CARTESIAN_POINT('Ctrl Pts',(-0.00858076872269995,0.155653752489481,
2.21252449965377));
#21663=CARTESIAN_POINT('Ctrl Pts',(-0.0187969842381853,0.154410089966781,
2.21326180897575));
#21664=CARTESIAN_POINT('Ctrl Pts',(-0.0289936767261386,0.153168804063645,
2.21399770931119));
#21665=CARTESIAN_POINT('Ctrl Pts',(-0.0390895324633264,0.150910415862194,
2.21473360964663));
#21666=CARTESIAN_POINT('Ctrl Pts',(-0.0488704089261867,0.147673577973134,
2.21546950998207));
#21667=CARTESIAN_POINT('Ctrl Pts',(-0.0539023638633416,0.146008326146422,
2.21584810768139));
#21668=CARTESIAN_POINT('Ctrl Pts',(-0.0588510526583658,0.144084945625908,
2.21622670538071));
#21669=CARTESIAN_POINT('Ctrl Pts',(-0.0636886258329906,0.141913922641527,
2.21660530308003));
#21670=CARTESIAN_POINT('Ctrl Pts',(-0.0637081998868965,0.141956949220948,
2.1466152095062));
#21671=CARTESIAN_POINT('Ctrl Pts',(-0.101121651380785,0.124710229304317,
2.14956891187111));
#21672=CARTESIAN_POINT('Ctrl Pts',(-0.145741622366923,0.0779923160122845,
2.15383235576962));
#21673=CARTESIAN_POINT('Ctrl Pts',(-0.15550054095579,0.0184426036431841,
2.15809579966814));
#21674=CARTESIAN_POINT('Ctrl Pts',(-0.155381214903208,0.000110939127196429,
2.15940554120174));
#21675=CARTESIAN_POINT('Ctrl Pts',(-0.0636886258331769,0.141913922641443,
2.1328902089718));
#21676=CARTESIAN_POINT('Ctrl Pts',(-0.0660169911472436,0.14086899072405,
2.13308540328567));
#21677=CARTESIAN_POINT('Ctrl Pts',(-0.0683208869914562,0.139766198311673,
2.13327922358076));
#21678=CARTESIAN_POINT('Ctrl Pts',(-0.0726221572309729,0.137575376390049,
2.13364111494803));
#21679=CARTESIAN_POINT('Ctrl Pts',(-0.074623493377058,0.136500174458298,
2.13380951295736));
#21680=CARTESIAN_POINT('Ctrl Pts',(-0.0770515419109373,0.135126350957108,
2.13401320397298));
#21681=CARTESIAN_POINT('Ctrl Pts',(-0.0775011181018852,0.134869001432455,
2.134050892937));
#21682=CARTESIAN_POINT('Ctrl Pts',(-0.0782054811963862,0.134461119929222,
2.13410988981991));
#21683=CARTESIAN_POINT('Ctrl Pts',(-0.0784611328148135,0.134312101849352,
2.13413129228043));
#21684=CARTESIAN_POINT('Ctrl Pts',(-0.0789391602791836,0.134031631350248,
2.13417128912932));
#21685=CARTESIAN_POINT('Ctrl Pts',(-0.0791616313086886,0.133900356079015,
2.13418989404401));
#21686=CARTESIAN_POINT('Ctrl Pts',(-0.0796697893692687,0.13359879405042,
2.13423237036266));
#21687=CARTESIAN_POINT('Ctrl Pts',(-0.079955257667684,0.133428145032307,
2.13425621791842));
#21688=CARTESIAN_POINT('Ctrl Pts',(-0.0808345705958355,0.13289866852993,
2.1343296369212));
#21689=CARTESIAN_POINT('Ctrl Pts',(-0.0814265746190951,0.132536775629558,
2.13437901402411));
#21690=CARTESIAN_POINT('Ctrl Pts',(-0.0870306301950694,0.129059285588559,
2.13484612591801));
#21691=CARTESIAN_POINT('Ctrl Pts',(-0.0918646957790118,0.125664342741429,
2.1352467978858));
#21692=CARTESIAN_POINT('Ctrl Pts',(-0.104292549765392,0.115834846101169,
2.13630449511134));
#21693=CARTESIAN_POINT('Ctrl Pts',(-0.111481215559507,0.108933905415754,
2.13694806206204));
#21694=CARTESIAN_POINT('Ctrl Pts',(-0.122076923861692,0.0966068036517986,
2.13803296018742));
#21695=CARTESIAN_POINT('Ctrl Pts',(-0.125895963225234,0.0915742366820963,
2.13846094260296));
#21696=CARTESIAN_POINT('Ctrl Pts',(-0.130218059858009,0.0850954789193387,
2.13900405786398));
#21697=CARTESIAN_POINT('Ctrl Pts',(-0.131020099688287,0.0838553329261292,
2.13910766737493));
#21698=CARTESIAN_POINT('Ctrl Pts',(-0.132143950138925,0.0820620979977112,
2.13925708130983));
#21699=CARTESIAN_POINT('Ctrl Pts',(-0.132480214152427,0.0815181226608786,
2.13930235324905));
#21700=CARTESIAN_POINT('Ctrl Pts',(-0.133057638284181,0.0805710125096015,
2.13938109302485));
#21701=CARTESIAN_POINT('Ctrl Pts',(-0.133300346321974,0.0801688270100914,
2.13941450381366));
#21702=CARTESIAN_POINT('Ctrl Pts',(-0.13376370459128,0.0793930857309455,
2.13947890105814));
#21703=CARTESIAN_POINT('Ctrl Pts',(-0.133984621346033,0.0790196935174879,
2.13950987743686));
#21704=CARTESIAN_POINT('Ctrl Pts',(-0.134559661831712,0.0780384189484672,
2.1395912333798));
#21705=CARTESIAN_POINT('Ctrl Pts',(-0.134911225284298,0.077429055827792,
2.13964170476628));
#21706=CARTESIAN_POINT('Ctrl Pts',(-0.136118623782933,0.0753030894724131,
2.13981763426765));
#21707=CARTESIAN_POINT('Ctrl Pts',(-0.136953086795314,0.0737745659677436,
2.13994385026327));
#21708=CARTESIAN_POINT('Ctrl Pts',(-0.143208624521256,0.0618440021030586,
2.14092731086853));
#21709=CARTESIAN_POINT('Ctrl Pts',(-0.147461917323854,0.0508749674725732,
2.14182601688876));
#21710=CARTESIAN_POINT('Ctrl Pts',(-0.151793605044927,0.0343916342501916,
2.14314750614871));
#21711=CARTESIAN_POINT('Ctrl Pts',(-0.152880620568386,0.0291822299549133,
2.14356043826949));
#21712=CARTESIAN_POINT('Ctrl Pts',(-0.15420048097391,0.0207039916653352,
2.14421732374455));
#21713=CARTESIAN_POINT('Ctrl Pts',(-0.154600784969782,0.0174655102016115,
2.14446469468069));
#21714=CARTESIAN_POINT('Ctrl Pts',(-0.15500816346531,0.013026863815089,
2.14479700796752));
#21715=CARTESIAN_POINT('Ctrl Pts',(-0.155103651586189,0.0118358524301557,
2.14488551622584));
#21716=CARTESIAN_POINT('Ctrl Pts',(-0.155243882151083,0.00979130937018618,
2.14503619349355));
#21717=CARTESIAN_POINT('Ctrl Pts',(-0.155295329555652,0.00893831033988605,
2.14509868175035));
#21718=CARTESIAN_POINT('Ctrl Pts',(-0.155358562299612,0.00772338469619673,
2.14518710950521));
#21719=CARTESIAN_POINT('Ctrl Pts',(-0.155376116359966,0.0073617948263221,
2.14521335528877));
#21720=CARTESIAN_POINT('Ctrl Pts',(-0.15540421959229,0.00673794620559497,
2.14525850844299));
#21721=CARTESIAN_POINT('Ctrl Pts',(-0.15541536756059,0.00647571745886528,
2.14527744893267));
#21722=CARTESIAN_POINT('Ctrl Pts',(-0.155435709740474,0.0059668701674449,
2.14531412503386));
#21723=CARTESIAN_POINT('Ctrl Pts',(-0.155444980785915,0.00572025811611256,
2.14533186500484));
#21724=CARTESIAN_POINT('Ctrl Pts',(-0.155465950470758,0.00512470841408515,
2.14537462337654));
#21725=CARTESIAN_POINT('Ctrl Pts',(-0.155477061388796,0.00477574919723898,
2.14539960918499));
#21726=CARTESIAN_POINT('Ctrl Pts',(-0.155513813946436,0.00348483744748929,
2.14549179721318));
#21727=CARTESIAN_POINT('Ctrl Pts',(-0.155532071846496,0.00254266870293689,
2.14555860299013));
#21728=CARTESIAN_POINT('Ctrl Pts',(-0.155547088414487,0.0010831836899177,
2.14566143200919));
#21729=CARTESIAN_POINT('Ctrl Pts',(-0.155549830254567,0.00056597405139784,
2.14569774445918));
#21730=CARTESIAN_POINT('Ctrl Pts',(-0.155553009013036,-0.00957632917392199,
2.14640748139099));
#21731=CARTESIAN_POINT('Ctrl Pts',(-0.154662648232899,-0.0191824693484842,
2.14703920233448));
#21732=CARTESIAN_POINT('Ctrl Pts',(-0.150827262360558,-0.0396528162620391,
2.14840986053697));
#21733=CARTESIAN_POINT('Ctrl Pts',(-0.147582757689397,-0.0504032958235261,
2.14914702796375));
#21734=CARTESIAN_POINT('Ctrl Pts',(-0.142528464659535,-0.0623258617002273,
2.15004688918939));
#21735=CARTESIAN_POINT('Ctrl Pts',(-0.141816961770028,-0.0639282816438271,
2.15016957519926));
#21736=CARTESIAN_POINT('Ctrl Pts',(-0.140781385131717,-0.066158157878763,
2.15034292533514));
#21737=CARTESIAN_POINT('Ctrl Pts',(-0.140479873336042,-0.0667959984688954,
2.1503928160626));
#21738=CARTESIAN_POINT('Ctrl Pts',(-0.13998579833137,-0.0678230588884798,
2.15047365561208));
#21739=CARTESIAN_POINT('Ctrl Pts',(-0.139795923496471,-0.0682135676991828,
2.1505045111557));
#21740=CARTESIAN_POINT('Ctrl Pts',(-0.139397362288651,-0.0690246209204112,
2.15056884589346));
#21741=CARTESIAN_POINT('Ctrl Pts',(-0.139188402425506,-0.0694450252184121,
2.15060233435117));
#21742=CARTESIAN_POINT('Ctrl Pts',(-0.138691015863459,-0.0704344488879261,
2.15068148655744));
#21743=CARTESIAN_POINT('Ctrl Pts',(-0.138400987391194,-0.0710026488102514,
2.15072720596713));
#21744=CARTESIAN_POINT('Ctrl Pts',(-0.137432114314633,-0.0728722926324531,
2.15087853137526));
#21745=CARTESIAN_POINT('Ctrl Pts',(-0.136738361755392,-0.0741658764413903,
2.15098465991372));
#21746=CARTESIAN_POINT('Ctrl Pts',(-0.132999201335909,-0.0809071438232189,
2.15154546334311));
#21747=CARTESIAN_POINT('Ctrl Pts',(-0.129646684549319,-0.086176975962864,
2.15201103484421));
#21748=CARTESIAN_POINT('Ctrl Pts',(-0.120134372237566,-0.0993132358241871,
2.15324450473581));
#21749=CARTESIAN_POINT('Ctrl Pts',(-0.113517547093068,-0.106813508048795,
2.15402485757897));
#21750=CARTESIAN_POINT('Ctrl Pts',(-0.104281169918516,-0.115448470096155,
2.15499880432721));
#21751=CARTESIAN_POINT('Ctrl Pts',(-0.102286881648717,-0.117219054610476,
2.15520305482506));
#21752=CARTESIAN_POINT('Ctrl Pts',(-0.0976450176969882,-0.12113150613975,
2.15566341145255));
#21753=CARTESIAN_POINT('Ctrl Pts',(-0.0949704747078093,-0.123239623089311,
2.15591812252595));
#21754=CARTESIAN_POINT('Ctrl Pts',(-0.0917805866619302,-0.125588359384388,
2.15620801789963));
#21755=CARTESIAN_POINT('Ctrl Pts',(-0.0913307485896006,-0.125915870675793,
2.1562485874287));
#21756=CARTESIAN_POINT('Ctrl Pts',(-0.090607532982875,-0.126436503743735,
2.15631330260624));
#21757=CARTESIAN_POINT('Ctrl Pts',(-0.0903352783986377,-0.126631165178803,
2.15633755000596));
#21758=CARTESIAN_POINT('Ctrl Pts',(-0.0898510596985914,-0.12697502414216,
2.15638046925827));
#21759=CARTESIAN_POINT('Ctrl Pts',(-0.0896393487143254,-0.127124572176622,
2.15639916491298));
#21760=CARTESIAN_POINT('Ctrl Pts',(-0.0891889537829955,-0.12744103675876,
2.15643878976897));
#21761=CARTESIAN_POINT('Ctrl Pts',(-0.0889501750260208,-0.127607812040246,
2.1564597093528));
#21762=CARTESIAN_POINT('Ctrl Pts',(-0.0883027004698815,-0.12805734093405,
2.15651620240084));
#21763=CARTESIAN_POINT('Ctrl Pts',(-0.0878931109526026,-0.128338811520761,
2.15655168982881));
#21764=CARTESIAN_POINT('Ctrl Pts',(-0.0858318452554503,-0.129740820200941,
2.15672907057403));
#21765=CARTESIAN_POINT('Ctrl Pts',(-0.0841599610416281,-0.130831525481305,
2.15686906486807));
#21766=CARTESIAN_POINT('Ctrl Pts',(-0.0792410325040952,-0.133907209883295,
2.15727127005465));
#21767=CARTESIAN_POINT('Ctrl Pts',(-0.0759414119874704,-0.135805702253897,
2.15752912808194));
#21768=CARTESIAN_POINT('Ctrl Pts',(-0.0634724587087657,-0.142383169019051,
2.15847274967042));
#21769=CARTESIAN_POINT('Ctrl Pts',(-0.0539154935395429,-0.146269797743455,
2.15913800836375));
#21770=CARTESIAN_POINT('Ctrl Pts',(-0.0373841405397244,-0.151150435148778,
2.16028795169779));
#21771=CARTESIAN_POINT('Ctrl Pts',(-0.0306005687088528,-0.15266830854688,
2.16075925850456));
#21772=CARTESIAN_POINT('Ctrl Pts',(-0.0227449809000074,-0.15388138239273,
2.16131609694688));
#21773=CARTESIAN_POINT('Ctrl Pts',(-0.0217495828496704,-0.15402522379476,
2.16138684483133));
#21774=CARTESIAN_POINT('Ctrl Pts',(-0.0201549390142474,-0.154239894146944,
2.16150051948653));
#21775=CARTESIAN_POINT('Ctrl Pts',(-0.019556542243215,-0.154316908179411,
2.1615432516709));
#21776=CARTESIAN_POINT('Ctrl Pts',(-0.01849562723894,-0.154447178745311,
2.16161915294675));
#21777=CARTESIAN_POINT('Ctrl Pts',(-0.0180332865962473,-0.154501844051324,
2.1616522773486));
#21778=CARTESIAN_POINT('Ctrl Pts',(-0.0170718529500173,-0.154611145826206,
2.16172126041987));
#21779=CARTESIAN_POINT('Ctrl Pts',(-0.0165727276296994,-0.154665443020899,
2.16175712933995));
#21780=CARTESIAN_POINT('Ctrl Pts',(-0.015281044667889,-0.154799634051358,
2.16185010534437));
#21781=CARTESIAN_POINT('Ctrl Pts',(-0.0144881291743909,-0.154875857052642,
2.1619073268212));
#21782=CARTESIAN_POINT('Ctrl Pts',(-0.0110918737770631,-0.155176030171966,
2.16215307741864));
#21783=CARTESIAN_POINT('Ctrl Pts',(-0.0084838442530061,-0.155340441775755,
2.16234345242823));
#21784=CARTESIAN_POINT('Ctrl Pts',(-0.00160101816005513,-0.155600499910772,
2.1628506149305));
#21785=CARTESIAN_POINT('Ctrl Pts',(0.00267546407588023,-0.155585714704597,
2.1631705929119));
#21786=CARTESIAN_POINT('Ctrl Pts',(0.0190840290486806,-0.154852313143182,
2.16441645935159));
#21787=CARTESIAN_POINT('Ctrl Pts',(0.0311156172426077,-0.152889543478955,
2.16537225069882));
#21788=CARTESIAN_POINT('Ctrl Pts',(0.0469359789972818,-0.148362271959415,
2.16662861378158));
#21789=CARTESIAN_POINT('Ctrl Pts',(0.0510259411921149,-0.147005821667162,
2.16695286356551));
#21790=CARTESIAN_POINT('Ctrl Pts',(0.0556607734020622,-0.14525185254536,
2.16731582243976));
#21791=CARTESIAN_POINT('Ctrl Pts',(0.0562653743922906,-0.145018723093558,
2.16736307886673));
#21792=CARTESIAN_POINT('Ctrl Pts',(0.0571736753913093,-0.144661953644649,
2.16743391769736));
#21793=CARTESIAN_POINT('Ctrl Pts',(0.0574784598625501,-0.144541124415357,
2.16745766153654));
#21794=CARTESIAN_POINT('Ctrl Pts',(0.058022291051215,-0.144323534960282,
2.16749997781683));
#21795=CARTESIAN_POINT('Ctrl Pts',(0.0582614803767429,-0.14422714345853,
2.16751857191401));
#21796=CARTESIAN_POINT('Ctrl Pts',(0.0587775700087398,-0.14401766982145,
2.16755865329977));
#21797=CARTESIAN_POINT('Ctrl Pts',(0.0590543834770298,-0.143904384065221,
2.16758012807128));
#21798=CARTESIAN_POINT('Ctrl Pts',(0.0598231212537174,-0.143587186851067,
2.16763970467767));
#21799=CARTESIAN_POINT('Ctrl Pts',(0.0603143342386319,-0.143381544041978,
2.16767770379636));
#21800=CARTESIAN_POINT('Ctrl Pts',(0.0630926906561102,-0.142201600190267,
2.16789229008545));
#21801=CARTESIAN_POINT('Ctrl Pts',(0.0653574414135578,-0.141175031265913,
2.16806589480209));
#21802=CARTESIAN_POINT('Ctrl Pts',(0.080923847741506,-0.133664110767473,
2.16925661359228));
#21803=CARTESIAN_POINT('Ctrl Pts',(0.0932665513474686,-0.125364381436631,
2.17019422091939));
#21804=CARTESIAN_POINT('Ctrl Pts',(0.105566661086969,-0.114256827072005,
2.17130745036735));
#21805=CARTESIAN_POINT('Ctrl Pts',(0.106861355862433,-0.113046860913555,
2.17142709209935));
#21806=CARTESIAN_POINT('Ctrl Pts',(0.111131628690177,-0.108917129366686,
2.17183073280626));
#21807=CARTESIAN_POINT('Ctrl Pts',(0.114010232381242,-0.105900149115265,
2.17211803421125));
#21808=CARTESIAN_POINT('Ctrl Pts',(0.117344395061399,-0.102112032106714,
2.17247226249401));
#21809=CARTESIAN_POINT('Ctrl Pts',(0.117919169473969,-0.101447738109457,
2.17253414778933));
#21810=CARTESIAN_POINT('Ctrl Pts',(0.118858433709445,-0.100343418598042,
2.17263666550434));
#21811=CARTESIAN_POINT('Ctrl Pts',(0.119226186195294,-0.099906183138633,
2.17267716387004));
#21812=CARTESIAN_POINT('Ctrl Pts',(0.119886027097854,-0.0991128403745894,
2.17275048725313));
#21813=CARTESIAN_POINT('Ctrl Pts',(0.120178960001454,-0.0987574411628452,
2.17278327749431));
#21814=CARTESIAN_POINT('Ctrl Pts',(0.120802671555645,-0.0979938420759882,
2.17285361142018));
#21815=CARTESIAN_POINT('Ctrl Pts',(0.121132968214345,-0.0975852577947737,
2.17289117394836));
#21816=CARTESIAN_POINT('Ctrl Pts',(0.122024630948541,-0.0964707489380403,
2.17299344669418));
#21817=CARTESIAN_POINT('Ctrl Pts',(0.122581929843276,-0.0957616121994802,
2.17305831772651));
#21818=CARTESIAN_POINT('Ctrl Pts',(0.125442527249752,-0.0920557459832751,
2.1733963285068));
#21819=CARTESIAN_POINT('Ctrl Pts',(0.127642016235695,-0.0889808917727768,
2.17367347781928));
#21820=CARTESIAN_POINT('Ctrl Pts',(0.137939983336804,-0.0734159577205989,
2.17506207928698));
#21821=CARTESIAN_POINT('Ctrl Pts',(0.144327768023264,-0.0598889390220219,
2.17623513251602));
#21822=CARTESIAN_POINT('Ctrl Pts',(0.150011388456629,-0.0413819418323274,
2.17771495930309));
#21823=CARTESIAN_POINT('Ctrl Pts',(0.151141339699327,-0.0370430362492653,
2.17805272408048));
#21824=CARTESIAN_POINT('Ctrl Pts',(0.152221410351436,-0.0320137911054857,
2.17842952082074));
#21825=CARTESIAN_POINT('Ctrl Pts',(0.152356258021773,-0.031365765958149,
2.17847779380394));
#21826=CARTESIAN_POINT('Ctrl Pts',(0.152551396518006,-0.0303970453885356,
2.17854952242973));
#21827=CARTESIAN_POINT('Ctrl Pts',(0.152614819048364,-0.0300770005169151,
2.17857314955833));
#21828=CARTESIAN_POINT('Ctrl Pts',(0.152726543271103,-0.0295037610728202,
2.17861533967494));
#21829=CARTESIAN_POINT('Ctrl Pts',(0.152775222829793,-0.029250644947397,
2.17863392378123));
#21830=CARTESIAN_POINT('Ctrl Pts',(0.152879244208359,-0.0287024273093525,
2.17867407666903));
#21831=CARTESIAN_POINT('Ctrl Pts',(0.152934360729109,-0.028407287017642,
2.17869563252361));
#21832=CARTESIAN_POINT('Ctrl Pts',(0.153085807742378,-0.0275830951462181,
2.17875566278421));
#21833=CARTESIAN_POINT('Ctrl Pts',(0.153180251145834,-0.0270536938641554,
2.17879403191009));
#21834=CARTESIAN_POINT('Ctrl Pts',(0.153710047501832,-0.0239921826632196,
2.17901487929414));
#21835=CARTESIAN_POINT('Ctrl Pts',(0.154085390504345,-0.0214498960006938,
2.17919416718502));
#21836=CARTESIAN_POINT('Ctrl Pts',(0.156187133044349,-0.00427971991433805,
2.18038468284168));
#21837=CARTESIAN_POINT('Ctrl Pts',(0.155891464619304,0.0105213047301718,
2.18131828246991));
#21838=CARTESIAN_POINT('Ctrl Pts',(0.153218677638573,0.0268940111399787,
2.18243276336411));
#21839=CARTESIAN_POINT('Ctrl Pts',(0.152886698950583,0.0287212102522075,
2.18255819625035));
#21840=CARTESIAN_POINT('Ctrl Pts',(0.151722591172594,0.0345345911704988,
2.18296134794165));
#21841=CARTESIAN_POINT('Ctrl Pts',(0.150766689182046,0.0384939363462242,
2.18324213517661));
#21842=CARTESIAN_POINT('Ctrl Pts',(0.149418884779932,0.0432499693966803,
2.18358916198354));
#21843=CARTESIAN_POINT('Ctrl Pts',(0.149174070315314,0.0440869558046919,
2.18365060252135));
#21844=CARTESIAN_POINT('Ctrl Pts',(0.148757808466609,0.0454669230190861,
2.18375253466676));
#21845=CARTESIAN_POINT('Ctrl Pts',(0.148590391998414,0.0460111079928682,
2.18379289489307));
#21846=CARTESIAN_POINT('Ctrl Pts',(0.14828219631769,0.0469936670019351,
2.1838660700102));
#21847=CARTESIAN_POINT('Ctrl Pts',(0.148142450514052,0.0474323605824498,
2.18389885076099));
#21848=CARTESIAN_POINT('Ctrl Pts',(0.147838637253949,0.0483716586027706,
2.18396927685111));
#21849=CARTESIAN_POINT('Ctrl Pts',(0.147673970629489,0.0488720616201343,
2.18400694152024));
#21850=CARTESIAN_POINT('Ctrl Pts',(0.147218469819651,0.0502329540024445,
2.18410977760331));
#21851=CARTESIAN_POINT('Ctrl Pts',(0.146922639400423,0.051091736028941,
2.18417511285159));
#21852=CARTESIAN_POINT('Ctrl Pts',(0.1453279802132,0.0555925532874534,2.18451990580471));
#21853=CARTESIAN_POINT('Ctrl Pts',(0.143901316198438,0.0591874994254227,
2.18480356770326));
#21854=CARTESIAN_POINT('Ctrl Pts',(0.136365909383786,0.076287577932957,
2.18619492745192));
#21855=CARTESIAN_POINT('Ctrl Pts',(0.128482064653812,0.0889250636299577,
2.1873631202283));
#21856=CARTESIAN_POINT('Ctrl Pts',(0.116067083713127,0.103653319518036,
2.1888351851711));
#21857=CARTESIAN_POINT('Ctrl Pts',(0.113056099038681,0.106929444877068,
2.1891703150065));
#21858=CARTESIAN_POINT('Ctrl Pts',(0.109440909998381,0.110539252576792,
2.18954453433145));
#21859=CARTESIAN_POINT('Ctrl Pts',(0.108970332334835,0.11100317947858,2.18959272662328));
#21860=CARTESIAN_POINT('Ctrl Pts',(0.108263164400714,0.111691521785521,
2.18966435914577));
#21861=CARTESIAN_POINT('Ctrl Pts',(0.10802881009828,0.111918206735427,2.18968797020011));
#21862=CARTESIAN_POINT('Ctrl Pts',(0.107607925604363,0.112322763835223,
2.18973014300443));
#21863=CARTESIAN_POINT('Ctrl Pts',(0.107421665344474,0.112500909981275,
2.18974872579851));
#21864=CARTESIAN_POINT('Ctrl Pts',(0.107017352793025,0.112885689708462,
2.18978888882276));
#21865=CARTESIAN_POINT('Ctrl Pts',(0.106799145048987,0.113092154284681,
2.18981045606867));
#21866=CARTESIAN_POINT('Ctrl Pts',(0.106188123902481,0.113666946843727,
2.18987055011425));
#21867=CARTESIAN_POINT('Ctrl Pts',(0.10579398876875,0.11403387402876,2.18990897127112));
#21868=CARTESIAN_POINT('Ctrl Pts',(0.103499602418438,0.116147739827136,
2.19013071754495));
#21869=CARTESIAN_POINT('Ctrl Pts',(0.10155786521983,0.11784934145035,2.19031082183706));
#21870=CARTESIAN_POINT('Ctrl Pts',(0.0882665781434985,0.12892425317794,
2.19150132377397));
#21871=CARTESIAN_POINT('Ctrl Pts',(0.0756774914708116,0.136694837702149,
2.19243435912003));
#21872=CARTESIAN_POINT('Ctrl Pts',(0.0604678209613985,0.143328098318324,
2.19354911717698));
#21873=CARTESIAN_POINT('Ctrl Pts',(0.058740016146079,0.144044823772724,
2.19367546635138));
#21874=CARTESIAN_POINT('Ctrl Pts',(0.0532249452615636,0.146216849267518,
2.19407857004239));
#21875=CARTESIAN_POINT('Ctrl Pts',(0.0493937358494896,0.147555127867977,
2.19435835639163));
#21876=CARTESIAN_POINT('Ctrl Pts',(0.0446820724337822,0.148996890554439,
2.19470426613834));
#21877=CARTESIAN_POINT('Ctrl Pts',(0.0438471651956738,0.149244721987937,
2.19476562711256));
#21878=CARTESIAN_POINT('Ctrl Pts',(0.0424634148965213,0.149642857035555,
2.19486745449038));
#21879=CARTESIAN_POINT('Ctrl Pts',(0.0419157416018176,0.149797185743918,
2.19490778998844));
#21880=CARTESIAN_POINT('Ctrl Pts',(0.0409234288375339,0.150070941330244,
2.19498093864806));
#21881=CARTESIAN_POINT('Ctrl Pts',(0.040479080290673,0.15019140624561,2.19501371778359));
#21882=CARTESIAN_POINT('Ctrl Pts',(0.0400330342233529,0.150310208144181,
2.19504664756934));
#21883=CARTESIAN_POINT('Ctrl Pts',(0.0400318606011181,0.150310520717236,
2.19504673421333));
#21884=CARTESIAN_POINT('Ctrl Pts',(0.0400295202429271,0.150311143999967,
2.19504690699325));
#21885=CARTESIAN_POINT('Ctrl Pts',(0.0400283532855143,0.150311454768783,
2.19504699314555));
#21886=CARTESIAN_POINT('Ctrl Pts',(0.0400260259182125,0.150312074533738,
2.1950471649671));
#21887=CARTESIAN_POINT('Ctrl Pts',(0.0400248655008104,0.150312383532041,
2.19504725063691));
#21888=CARTESIAN_POINT('Ctrl Pts',(0.040022551155019,0.15031299977204,2.19504742149782));
#21889=CARTESIAN_POINT('Ctrl Pts',(0.0400213972215343,0.150313307015252,
2.19504750668929));
#21890=CARTESIAN_POINT('Ctrl Pts',(0.0400190957973346,0.150313919757863,
2.19504767659692));
#21891=CARTESIAN_POINT('Ctrl Pts',(0.0400179482970169,0.150314225259976,
2.19504776131378));
#21892=CARTESIAN_POINT('Ctrl Pts',(0.0400156596820435,0.150314834536065,
2.19504793027641));
#21893=CARTESIAN_POINT('Ctrl Pts',(0.0400145185607507,0.150315138311965,
2.19504801452267));
#21894=CARTESIAN_POINT('Ctrl Pts',(0.0400122426538242,0.150315744149407,
2.19504818254776));
#21895=CARTESIAN_POINT('Ctrl Pts',(0.0400111078601173,0.150316046213252,
2.19504826632719));
#21896=CARTESIAN_POINT('Ctrl Pts',(0.0400088445550172,0.150316648641245,
2.19504843342258));
#21897=CARTESIAN_POINT('Ctrl Pts',(0.0400077160362043,0.15031694900752,
2.19504851673907));
#21898=CARTESIAN_POINT('Ctrl Pts',(0.0400054652336443,0.150317548053405,
2.19504868291207));
#21899=CARTESIAN_POINT('Ctrl Pts',(0.0400043429398311,0.150317846735843,
2.19504876576931));
#21900=CARTESIAN_POINT('Ctrl Pts',(0.0400021045351428,0.150318442428375,
2.19504893102764));
#21901=CARTESIAN_POINT('Ctrl Pts',(0.0400009884150471,0.150318739441071,
2.19504901342941));
#21902=CARTESIAN_POINT('Ctrl Pts',(0.0394966174363725,0.150452952480337,
2.19508625058655));
#21903=CARTESIAN_POINT('Ctrl Pts',(0.038992698963713,0.150584338874641,
2.19512348679596));
#21904=CARTESIAN_POINT('Ctrl Pts',(0.037626282433313,0.15093328527227,2.19522454917707));
#21905=CARTESIAN_POINT('Ctrl Pts',(0.0367625739951586,0.151145978527453,
2.19528853096926));
#21906=CARTESIAN_POINT('Ctrl Pts',(0.0348421117614178,0.151601468890245,
2.1954310370156));
#21907=CARTESIAN_POINT('Ctrl Pts',(0.0337845563873765,0.151840645944173,
2.19550967375551));
#21908=CARTESIAN_POINT('Ctrl Pts',(0.0305611906194461,0.152534301925005,
2.19574988237738));
#21909=CARTESIAN_POINT('Ctrl Pts',(0.0283881884900447,0.152953618688722,
2.19591254353701));
#21910=CARTESIAN_POINT('Ctrl Pts',(0.011358084511525,0.15586446272202,2.1971934091327));
#21911=CARTESIAN_POINT('Ctrl Pts',(-0.0037795157964463,0.15623150014638,
2.19837911666908));
#21912=CARTESIAN_POINT('Ctrl Pts',(-0.01976205936095,0.154293056099371,
2.19961193071215));
#21913=CARTESIAN_POINT('Ctrl Pts',(-0.0207942078137085,0.154157345448689,
2.19969140692819));
#21914=CARTESIAN_POINT('Ctrl Pts',(-0.0255731063562977,0.153480127833509,
2.20005854210484));
#21915=CARTESIAN_POINT('Ctrl Pts',(-0.0293010451904266,0.152812264396642,
2.20034255277593));
#21916=CARTESIAN_POINT('Ctrl Pts',(-0.0336146562908762,0.151875776124736,
2.20066570901339));
#21917=CARTESIAN_POINT('Ctrl Pts',(-0.0342272566340571,0.151738892280126,
2.20071147160936));
#21918=CARTESIAN_POINT('Ctrl Pts',(-0.0351543185566328,0.151525842834467,
2.20078050998261));
#21919=CARTESIAN_POINT('Ctrl Pts',(-0.0354693887289193,0.151452400536461,
2.20080393550929));
#21920=CARTESIAN_POINT('Ctrl Pts',(-0.036034884310486,0.15131872306628,
2.20084590953956));
#21921=CARTESIAN_POINT('Ctrl Pts',(-0.0362853899089312,0.151258848733661,
2.20086447823018));
#21922=CARTESIAN_POINT('Ctrl Pts',(-0.0368296030020982,0.15112734442563,
2.20090476303684));
#21923=CARTESIAN_POINT('Ctrl Pts',(-0.0371232499457968,0.151055480563059,
2.20092646549189));
#21924=CARTESIAN_POINT('Ctrl Pts',(-0.0379478727344393,0.150851121771983,
2.20098731857148));
#21925=CARTESIAN_POINT('Ctrl Pts',(-0.0384783688082745,0.150716678382996,
2.20102635919234));
#21926=CARTESIAN_POINT('Ctrl Pts',(-0.0416499751499815,0.149895062130021,
2.2012591843144));
#21927=CARTESIAN_POINT('Ctrl Pts',(-0.0442735475237671,0.14914122678078,
2.20144935995401));
#21928=CARTESIAN_POINT('Ctrl Pts',(-0.0526057991022602,0.146507817854672,
2.20204962024977));
#21929=CARTESIAN_POINT('Ctrl Pts',(-0.0582190549626605,0.144368577403726,
2.20244845233402));
#21930=CARTESIAN_POINT('Ctrl Pts',(-0.0636886613526676,0.141913906700877,
2.20284414165342));
#21931=CARTESIAN_POINT('Origin',(0.,0.,-0.129405622560373));
#21932=CARTESIAN_POINT('',(-0.0636886081915498,0.141913930558713,2.28656840831392));
#21933=CARTESIAN_POINT('',(-0.0636886258329926,0.141913922641526,2.27279455889198));
#21934=CARTESIAN_POINT('',(-0.0636886258329924,0.141913922641526,-0.129405622560373));
#21935=CARTESIAN_POINT('',(-0.155549959235335,-0.000112613879107687,2.22940562256037));
#21936=CARTESIAN_POINT('Ctrl Pts',(-0.0636886081915498,0.141913930558713,
2.28656840831392));
#21937=CARTESIAN_POINT('Ctrl Pts',(-0.0573573513556864,0.144755293167668,
2.28611116580639));
#21938=CARTESIAN_POINT('Ctrl Pts',(-0.0508393810386415,0.147171438272272,
2.28565645924617));
#21939=CARTESIAN_POINT('Ctrl Pts',(-0.0379348625092741,0.150993842402475,
2.28475646093028));
#21940=CARTESIAN_POINT('Ctrl Pts',(-0.0315829264545988,0.152448992633366,
2.28431354593895));
#21941=CARTESIAN_POINT('Ctrl Pts',(-0.0241771909634659,0.153662799599024,
2.28378773977956));
#21942=CARTESIAN_POINT('Ctrl Pts',(-0.0231937821712976,0.153814306651298,
2.28371773837351));
#21943=CARTESIAN_POINT('Ctrl Pts',(-0.0216149122255629,0.154042066862606,
2.28360503193009));
#21944=CARTESIAN_POINT('Ctrl Pts',(-0.0210203335993272,0.154124327576502,
2.28356251619436));
#21945=CARTESIAN_POINT('Ctrl Pts',(-0.019964169240911,0.154264224044377,
2.28348685968897));
#21946=CARTESIAN_POINT('Ctrl Pts',(-0.0195027702404401,0.15432323486059,
2.28345376260884));
#21947=CARTESIAN_POINT('Ctrl Pts',(-0.0185412962912334,0.154441822231064,
2.2833846959364));
#21948=CARTESIAN_POINT('Ctrl Pts',(-0.0180411835922698,0.154501041439202,
2.28334871551462));
#21949=CARTESIAN_POINT('Ctrl Pts',(-0.0167426573252954,0.154648411431805,
2.28325514536027));
#21950=CARTESIAN_POINT('Ctrl Pts',(-0.0159438416586882,0.154732807125449,
2.2831974384754));
#21951=CARTESIAN_POINT('Ctrl Pts',(-0.0124832655330437,0.155071338762232,
2.28294678745214));
#21952=CARTESIAN_POINT('Ctrl Pts',(-0.00981600324762601,0.155262991260491,
2.28275190462622));
#21953=CARTESIAN_POINT('Ctrl Pts',(-0.00273555764848378,0.155588579095533,
2.2822296970878));
#21954=CARTESIAN_POINT('Ctrl Pts',(0.00168037847960483,0.155603531053496,
2.28189894091815));
#21955=CARTESIAN_POINT('Ctrl Pts',(0.0184849974486085,0.154945035350905,
2.28062171486504));
#21956=CARTESIAN_POINT('Ctrl Pts',(0.0307753701326118,0.152978736820492,
2.27964472851734));
#21957=CARTESIAN_POINT('Ctrl Pts',(0.0464213459760401,0.148512050827812,
2.27840629214938));
#21958=CARTESIAN_POINT('Ctrl Pts',(0.0501010675833204,0.147311438723959,
2.27811586792665));
#21959=CARTESIAN_POINT('Ctrl Pts',(0.0543247881584176,0.145756708838042,
2.27778634090322));
#21960=CARTESIAN_POINT('Ctrl Pts',(0.0549157150812203,0.145535099043165,
2.27774032736285));
#21961=CARTESIAN_POINT('Ctrl Pts',(0.0558082223386521,0.145194180244331,
2.27767098375387));
#21962=CARTESIAN_POINT('Ctrl Pts',(0.0561107955107271,0.145077518209393,
2.27764750199097));
#21963=CARTESIAN_POINT('Ctrl Pts',(0.0566531351358926,0.144866459797971,
2.27760546355121));
#21964=CARTESIAN_POINT('Ctrl Pts',(0.0568930325451477,0.144772413623429,
2.27758688644834));
#21965=CARTESIAN_POINT('Ctrl Pts',(0.0574134757671532,0.144566892573746,
2.27754662409336));
#21966=CARTESIAN_POINT('Ctrl Pts',(0.057693930331708,0.144455197328433,
2.27752495232895));
#21967=CARTESIAN_POINT('Ctrl Pts',(0.0584797527270391,0.144139578177909,
2.27746429334337));
#21968=CARTESIAN_POINT('Ctrl Pts',(0.0589843835067336,0.14393381118546,
2.27742541495191));
#21969=CARTESIAN_POINT('Ctrl Pts',(0.0619707373189326,0.142697759495357,
2.27719572147635));
#21970=CARTESIAN_POINT('Ctrl Pts',(0.0644267013975265,0.141605880339322,
2.2770084026159));
#21971=CARTESIAN_POINT('Ctrl Pts',(0.0800739870305123,0.13415791258341,
2.27581742889312));
#21972=CARTESIAN_POINT('Ctrl Pts',(0.0923411546455998,0.12602938048,2.27488888769079));
#21973=CARTESIAN_POINT('Ctrl Pts',(0.104808348480506,0.114957069883973,
2.273768420861));
#21974=CARTESIAN_POINT('Ctrl Pts',(0.106298599288021,0.113580478595294,
2.273631288463));
#21975=CARTESIAN_POINT('Ctrl Pts',(0.110561457056521,0.109485350054613,
2.27322871837826));
#21976=CARTESIAN_POINT('Ctrl Pts',(0.113259539574259,0.106691846093292,
2.27296068672493));
#21977=CARTESIAN_POINT('Ctrl Pts',(0.116479193483515,0.103098441522035,
2.27262190544415));
#21978=CARTESIAN_POINT('Ctrl Pts',(0.117101852740555,0.102390659602416,
2.27255545459439));
#21979=CARTESIAN_POINT('Ctrl Pts',(0.118071101348591,0.101268500944805,
2.27245050778179));
#21980=CARTESIAN_POINT('Ctrl Pts',(0.11842203883526,0.100857894891781,2.27241219155885));
#21981=CARTESIAN_POINT('Ctrl Pts',(0.119038035523508,0.100129515275094,
2.27234436583517));
#21982=CARTESIAN_POINT('Ctrl Pts',(0.119303980194252,0.0998124943795168,
2.27231489290808));
#21983=CARTESIAN_POINT('Ctrl Pts',(0.119910650235786,0.0990834211175232,
2.27224721836863));
#21984=CARTESIAN_POINT('Ctrl Pts',(0.120250520706898,0.0986706675606195,
2.27220898259578));
#21985=CARTESIAN_POINT('Ctrl Pts',(0.121184306229015,0.0975246473260161,
2.27210302625334));
#21986=CARTESIAN_POINT('Ctrl Pts',(0.121773678588445,0.0967877267137006,
2.27203512478758));
#21987=CARTESIAN_POINT('Ctrl Pts',(0.125066621541656,0.0925927119457553,
2.27164982537739));
#21988=CARTESIAN_POINT('Ctrl Pts',(0.127629301959572,0.0890270984659791,
2.27132695774074));
#21989=CARTESIAN_POINT('Ctrl Pts',(0.135280764356334,0.0773706034538519,
2.27028440093614));
#21990=CARTESIAN_POINT('Ctrl Pts',(0.139776167646088,0.0689178634916385,
2.2695456545424));
#21991=CARTESIAN_POINT('Ctrl Pts',(0.146972611835888,0.0517410732806681,
2.26810146465739));
#21992=CARTESIAN_POINT('Ctrl Pts',(0.149739778504839,0.0430828345014801,
2.26739934261687));
#21993=CARTESIAN_POINT('Ctrl Pts',(0.151887410841179,0.0335631738011914,
2.26668414797492));
#21994=CARTESIAN_POINT('Ctrl Pts',(0.152033819262679,0.0328936172347227,
2.26663414585285));
#21995=CARTESIAN_POINT('Ctrl Pts',(0.152244370562465,0.0318992742220397,
2.26656035531206));
#21996=CARTESIAN_POINT('Ctrl Pts',(0.152311907121558,0.0315752279229992,
2.26653638098573));
#21997=CARTESIAN_POINT('Ctrl Pts',(0.152430293916657,0.0309979788080861,
2.26649380692038));
#21998=CARTESIAN_POINT('Ctrl Pts',(0.152481548328445,0.0307448632597523,
2.26647518449148));
#21999=CARTESIAN_POINT('Ctrl Pts',(0.152590420698477,0.0302002368390077,
2.26643521354255));
#22000=CARTESIAN_POINT('Ctrl Pts',(0.152647833676518,0.0299086889042221,
2.26641387679954));
#22001=CARTESIAN_POINT('Ctrl Pts',(0.152804054693212,0.0291032170932399,
2.26635509099754));
#22002=CARTESIAN_POINT('Ctrl Pts',(0.152901106425012,0.028588949804786,
2.26631774020638));
#22003=CARTESIAN_POINT('Ctrl Pts',(0.153418950685478,0.0257668606691734,
2.26611372178914));
#22004=CARTESIAN_POINT('Ctrl Pts',(0.153790120119515,0.0234500766939515,
2.26594970206205));
#22005=CARTESIAN_POINT('Ctrl Pts',(0.156078857414954,0.00675402169688695,
2.264786684186));
#22006=CARTESIAN_POINT('Ctrl Pts',(0.156029241330102,-0.0078240706720093,
2.26386612154625));
#22007=CARTESIAN_POINT('Ctrl Pts',(0.153529204700032,-0.025173349535694,
2.26269175450212));
#22008=CARTESIAN_POINT('Ctrl Pts',(0.153011820533273,-0.0281477418916587,
2.26248783645466));
#22009=CARTESIAN_POINT('Ctrl Pts',(0.152317642101105,-0.0315490688947975,
2.26225060191487));
#22010=CARTESIAN_POINT('Ctrl Pts',(0.152225087780352,-0.0319926630206638,
2.26221958289814));
#22011=CARTESIAN_POINT('Ctrl Pts',(0.151486894407884,-0.0354549377299227,
2.26197683609599));
#22012=CARTESIAN_POINT('Ctrl Pts',(0.15075350359295,-0.0384540073966083,
2.2617627292832));
#22013=CARTESIAN_POINT('Ctrl Pts',(0.149696803417965,-0.0422781922462996,
2.26148383369467));
#22014=CARTESIAN_POINT('Ctrl Pts',(0.149454979594136,-0.0431252537452708,
2.26142168374751));
#22015=CARTESIAN_POINT('Ctrl Pts',(0.149058744623597,-0.0444698149755887,
2.26132241417873));
#22016=CARTESIAN_POINT('Ctrl Pts',(0.148909003978465,-0.0449686814889762,
2.26128544666474));
#22017=CARTESIAN_POINT('Ctrl Pts',(0.14863540628562,-0.0458638296830602,
2.26121886446981));
#22018=CARTESIAN_POINT('Ctrl Pts',(0.148512462229922,-0.0462603872785091,
2.26118927986567));
#22019=CARTESIAN_POINT('Ctrl Pts',(0.148220924980014,-0.0471876034538367,
2.26111989695573));
#22020=CARTESIAN_POINT('Ctrl Pts',(0.148051068133613,-0.047717855476158,
2.26108005757885));
#22021=CARTESIAN_POINT('Ctrl Pts',(0.147553727050576,-0.0492422138340347,
2.26096505658488));
#22022=CARTESIAN_POINT('Ctrl Pts',(0.14721905687228,-0.0502339246315254,
2.26088965990593));
#22023=CARTESIAN_POINT('Ctrl Pts',(0.144699197162619,-0.0574593698189089,
2.26033597846919));
#22024=CARTESIAN_POINT('Ctrl Pts',(0.142129228447879,-0.0635507337839902,
2.25984495752987));
#22025=CARTESIAN_POINT('Ctrl Pts',(0.133612089324095,-0.0806170288581316,
2.25839672987307));
#22026=CARTESIAN_POINT('Ctrl Pts',(0.126723149867643,-0.091063143806636,
2.25741442235511));
#22027=CARTESIAN_POINT('Ctrl Pts',(0.116176032218369,-0.103507058960591,
2.25617307767612));
#22028=CARTESIAN_POINT('Ctrl Pts',(0.113582224672677,-0.106346914373026,
2.25588454096309));
#22029=CARTESIAN_POINT('Ctrl Pts',(0.110443628544838,-0.109537229009839,
2.25555688116506));
#22030=CARTESIAN_POINT('Ctrl Pts',(0.109998944927597,-0.10998377960677,
2.25551093502715));
#22031=CARTESIAN_POINT('Ctrl Pts',(0.109321461395658,-0.110655888333206,
2.255441671038));
#22032=CARTESIAN_POINT('Ctrl Pts',(0.10909065747102,-0.110883434300372,
2.25541820203834));
#22033=CARTESIAN_POINT('Ctrl Pts',(0.108675084841261,-0.111290587335218,
2.25537617645301));
#22034=CARTESIAN_POINT('Ctrl Pts',(0.108490580532803,-0.111470457224127,
2.25535759949977));
#22035=CARTESIAN_POINT('Ctrl Pts',(0.108088841023171,-0.111860163437116,
2.25531732670021));
#22036=CARTESIAN_POINT('Ctrl Pts',(0.107871441981383,-0.112069825229613,
2.25529564439006));
#22037=CARTESIAN_POINT('Ctrl Pts',(0.107259547250416,-0.112656512432037,
2.25523492308035));
#22038=CARTESIAN_POINT('Ctrl Pts',(0.106863670928656,-0.11303210220632,
2.25519599328371));
#22039=CARTESIAN_POINT('Ctrl Pts',(0.104497439687509,-0.115253533307624,
2.2549653419878));
#22040=CARTESIAN_POINT('Ctrl Pts',(0.102481120515078,-0.11705004981435,
2.2547771510607));
#22041=CARTESIAN_POINT('Ctrl Pts',(0.0892450389667769,-0.128238833966699,
2.25358621462346));
#22042=CARTESIAN_POINT('Ctrl Pts',(0.0767934630560027,-0.136061543583205,
2.25265830472956));
#22043=CARTESIAN_POINT('Ctrl Pts',(0.0615688317115607,-0.142860910162098,
2.25153783002241));
#22044=CARTESIAN_POINT('Ctrl Pts',(0.0596908032700508,-0.14365572800412,
2.25139997822199));
#22045=CARTESIAN_POINT('Ctrl Pts',(0.0542046407851404,-0.14585142381349,
2.2509975008022));
#22046=CARTESIAN_POINT('Ctrl Pts',(0.0505594023373035,-0.147154760200364,
2.25073031212824));
#22047=CARTESIAN_POINT('Ctrl Pts',(0.0459717518387923,-0.148604465522027,
2.25039247750613));
#22048=CARTESIAN_POINT('Ctrl Pts',(0.0450713584129952,-0.148880024588584,
2.25032610153214));
#22049=CARTESIAN_POINT('Ctrl Pts',(0.0436508872736459,-0.14930068318768,
2.25022124944924));
#22050=CARTESIAN_POINT('Ctrl Pts',(0.0431324499660888,-0.149451282050877,
2.2501829525775));
#22051=CARTESIAN_POINT('Ctrl Pts',(0.0422153069090767,-0.149712529756639,
2.25011514850273));
#22052=CARTESIAN_POINT('Ctrl Pts',(0.0418169216190779,-0.149824292969449,
2.25008567779496));
#22053=CARTESIAN_POINT('Ctrl Pts',(0.0409128456458104,-0.150074036135658,
2.25001875463655));
#22054=CARTESIAN_POINT('Ctrl Pts',(0.0404068961543966,-0.150211051496321,
2.24998127134972));
#22055=CARTESIAN_POINT('Ctrl Pts',(0.0390259360379312,-0.150577545197679,
2.24987887289088));
#22056=CARTESIAN_POINT('Ctrl Pts',(0.0381496126816666,-0.150801948891273,
2.24981379505647));
#22057=CARTESIAN_POINT('Ctrl Pts',(0.0361971291219298,-0.151283821648048,
2.24966856057029));
#22058=CARTESIAN_POINT('Ctrl Pts',(0.0351200875582728,-0.15153747451188,
2.24958828511914));
#22059=CARTESIAN_POINT('Ctrl Pts',(0.0266612197224183,-0.153434591836196,
2.24895646394655));
#22060=CARTESIAN_POINT('Ctrl Pts',(0.019172334738909,-0.154548965718495,
2.24838827975225));
#22061=CARTESIAN_POINT('Ctrl Pts',(0.00701306501031108,-0.15546087879246,
2.24745370584204));
#22062=CARTESIAN_POINT('Ctrl Pts',(0.00237996351554062,-0.155600772695253,
2.24709500198779));
#22063=CARTESIAN_POINT('Ctrl Pts',(-0.0113164306047466,-0.155402435418559,
2.24603275093491));
#22064=CARTESIAN_POINT('Ctrl Pts',(-0.0203527782042444,-0.154479058725245,
2.24532871700704));
#22065=CARTESIAN_POINT('Ctrl Pts',(-0.0303976650125656,-0.152555336832543,
2.24457263715985));
#22066=CARTESIAN_POINT('Ctrl Pts',(-0.0315348394857559,-0.152324334722878,
2.2444874501976));
#22067=CARTESIAN_POINT('Ctrl Pts',(-0.0330826262982139,-0.151991845179949,
2.24437215725131));
#22068=CARTESIAN_POINT('Ctrl Pts',(-0.0334955283689098,-0.151901384966118,
2.24434146434602));
#22069=CARTESIAN_POINT('Ctrl Pts',(-0.0341495492331672,-0.151755303077253,
2.24429295452869));
#22070=CARTESIAN_POINT('Ctrl Pts',(-0.0343909086614062,-0.151700788161075,
2.24427507554927));
#22071=CARTESIAN_POINT('Ctrl Pts',(-0.0348877643931869,-0.151587318558925,
2.24423831931851));
#22072=CARTESIAN_POINT('Ctrl Pts',(-0.0351432417345333,-0.15152829377319,
2.24421944662984));
#22073=CARTESIAN_POINT('Ctrl Pts',(-0.0357492293967447,-0.151386673042685,
2.24417474261723));
#22074=CARTESIAN_POINT('Ctrl Pts',(-0.0360996073778895,-0.151303504690462,
2.24414894399397));
#22075=CARTESIAN_POINT('Ctrl Pts',(-0.0372692919054918,-0.151021565156767,
2.2440629729643));
#22076=CARTESIAN_POINT('Ctrl Pts',(-0.0380872904848871,-0.150817345321459,
2.24400310314584));
#22077=CARTESIAN_POINT('Ctrl Pts',(-0.0478919991860359,-0.148284661529589,
2.24328807669048));
#22078=CARTESIAN_POINT('Ctrl Pts',(-0.056656109061988,-0.145162421860327,
2.24267451143852));
#22079=CARTESIAN_POINT('Ctrl Pts',(-0.0763483297742828,-0.136089587162927,
2.24124642652981));
#22080=CARTESIAN_POINT('Ctrl Pts',(-0.0869441918015212,-0.12957661911029,
2.24043556295722));
#22081=CARTESIAN_POINT('Ctrl Pts',(-0.0979321353685671,-0.120862561180529,
2.23945970866766));
#22082=CARTESIAN_POINT('Ctrl Pts',(-0.0991937926249771,-0.119829265982124,
2.23934548715271));
#22083=CARTESIAN_POINT('Ctrl Pts',(-0.100909884418619,-0.118378115049075,
2.23918696625747));
#22084=CARTESIAN_POINT('Ctrl Pts',(-0.10137845885781,-0.117977078094951,
2.23914335057556));
#22085=CARTESIAN_POINT('Ctrl Pts',(-0.102177897647449,-0.117284586106956,
2.23906835806864));
#22086=CARTESIAN_POINT('Ctrl Pts',(-0.102509933327922,-0.116994489048573,
2.2390370374169));
#22087=CARTESIAN_POINT('Ctrl Pts',(-0.103173756093037,-0.116409516733341,
2.23897406711934));
#22088=CARTESIAN_POINT('Ctrl Pts',(-0.103505523224592,-0.116114625206865,
2.23894241697771));
#22089=CARTESIAN_POINT('Ctrl Pts',(-0.104275045865188,-0.115424715628329,
2.23886858482094));
#22090=CARTESIAN_POINT('Ctrl Pts',(-0.104711824018052,-0.115028622790872,
2.23882635787885));
#22091=CARTESIAN_POINT('Ctrl Pts',(-0.106040249937883,-0.113810101975912,
2.23869693568919));
#22092=CARTESIAN_POINT('Ctrl Pts',(-0.106924519525045,-0.112979736625554,
2.23860940422635));
#22093=CARTESIAN_POINT('Ctrl Pts',(-0.108944428928519,-0.111038004683485,
2.23840618681019));
#22094=CARTESIAN_POINT('Ctrl Pts',(-0.110072913868205,-0.109919426697514,
2.2382901945484));
#22095=CARTESIAN_POINT('Ctrl Pts',(-0.113826445543424,-0.106083076171633,
2.23789585560581));
#22096=CARTESIAN_POINT('Ctrl Pts',(-0.116369365902476,-0.103287197261522,
2.23761415878912));
#22097=CARTESIAN_POINT('Ctrl Pts',(-0.122020273007504,-0.0966003413014661,
2.23695319887407));
#22098=CARTESIAN_POINT('Ctrl Pts',(-0.125048203122969,-0.0926472501124097,
2.23657166515618));
#22099=CARTESIAN_POINT('Ctrl Pts',(-0.134497342267141,-0.0790020291946222,
2.23528941105982));
#22100=CARTESIAN_POINT('Ctrl Pts',(-0.140022341167246,-0.068736020863521,
2.23437688134712));
#22101=CARTESIAN_POINT('Ctrl Pts',(-0.144753114888704,-0.0569516885847873,
2.23343939579434));
#22102=CARTESIAN_POINT('Ctrl Pts',(-0.14514342647292,-0.055949486392273,
2.23336051379335));
#22103=CARTESIAN_POINT('Ctrl Pts',(-0.145668050126691,-0.0545599628760283,
2.23325238773368));
#22104=CARTESIAN_POINT('Ctrl Pts',(-0.145811261042839,-0.0541760698112806,
2.23322264498015));
#22105=CARTESIAN_POINT('Ctrl Pts',(-0.14603764843099,-0.0535618121466522,
2.23317526669559));
#22106=CARTESIAN_POINT('Ctrl Pts',(-0.146121799234582,-0.0533318129301595,
2.23315757404831));
#22107=CARTESIAN_POINT('Ctrl Pts',(-0.146295489809564,-0.0528535882687254,
2.23312088651856));
#22108=CARTESIAN_POINT('Ctrl Pts',(-0.146384941334058,-0.0526053332229557,
2.2331018972893));
#22109=CARTESIAN_POINT('Ctrl Pts',(-0.146598167357355,-0.0520088111325375,
2.23305640043931));
#22110=CARTESIAN_POINT('Ctrl Pts',(-0.146721334270555,-0.0516603250613235,
2.23302992873309));
#22111=CARTESIAN_POINT('Ctrl Pts',(-0.147139857263208,-0.0504625935176851,
2.23293930390087));
#22112=CARTESIAN_POINT('Ctrl Pts',(-0.147429099150707,-0.0496112060505376,
2.23287549989638));
#22113=CARTESIAN_POINT('Ctrl Pts',(-0.148110824645266,-0.0475459100635357,
2.23272209701623));
#22114=CARTESIAN_POINT('Ctrl Pts',(-0.148495795895353,-0.0463295672201016,
2.23263289047902));
#22115=CARTESIAN_POINT('Ctrl Pts',(-0.153287006421845,-0.0305177795719035,
2.23148626158064));
#22116=CARTESIAN_POINT('Ctrl Pts',(-0.155539540945981,-0.0153552451317254,
2.23052254341945));
#22117=CARTESIAN_POINT('Ctrl Pts',(-0.155549963665145,-0.000106319198765817,
2.22949944336375));
#22118=CARTESIAN_POINT('Ctrl Pts',(-0.0636886258329906,0.141913922641527,
2.21660530308003));
#22119=CARTESIAN_POINT('Ctrl Pts',(-0.073087183706925,0.137696005014694,
2.21734085213728));
#22120=CARTESIAN_POINT('Ctrl Pts',(-0.0820645472936867,0.132540662282221,
2.21807640119453));
#22121=CARTESIAN_POINT('Ctrl Pts',(-0.0904340546464224,0.126560200142888,
2.21881195025179));
#22122=CARTESIAN_POINT('Ctrl Pts',(-0.0988235076356814,0.12056548577591,
2.21954925221916));
#22123=CARTESIAN_POINT('Ctrl Pts',(-0.106601484691876,0.113742306694471,
2.22028655418654));
#22124=CARTESIAN_POINT('Ctrl Pts',(-0.113613251576689,0.106244207212309,
2.22102385615391));
#22125=CARTESIAN_POINT('Ctrl Pts',(-0.117229403188563,0.102377241157413,
2.22140410206647));
#22126=CARTESIAN_POINT('Ctrl Pts',(-0.120642374163594,0.0983313682361586,
2.22178434797902));
#22127=CARTESIAN_POINT('Ctrl Pts',(-0.123835241219437,0.0941309488538381,
2.22216459389158));
#22128=CARTESIAN_POINT('Ctrl Pts',(-0.130041164091348,0.0859666631944461,
2.22290367158083));
#22129=CARTESIAN_POINT('Ctrl Pts',(-0.135459995160728,0.077154802997613,
2.22364274927007));
#22130=CARTESIAN_POINT('Ctrl Pts',(-0.139962212458014,0.0678703291863065,
2.22438182695931));
#22131=CARTESIAN_POINT('Ctrl Pts',(-0.144454014774706,0.058607333150994,
2.22511919493992));
#22132=CARTESIAN_POINT('Ctrl Pts',(-0.148032938209205,0.0488746759435811,
2.22585656292052));
#22133=CARTESIAN_POINT('Ctrl Pts',(-0.150614199915162,0.038873709418006,
2.22659393090113));
#22134=CARTESIAN_POINT('Ctrl Pts',(-0.153193498779847,0.0288803478205996,
2.22733073817288));
#22135=CARTESIAN_POINT('Ctrl Pts',(-0.154776376478075,0.0186199611818154,
2.22806754544463));
#22136=CARTESIAN_POINT('Ctrl Pts',(-0.155327939155893,0.00830865919285778,
2.22880435271638));
#22137=CARTESIAN_POINT('Ctrl Pts',(-0.155477972965258,0.00550382126757846,
2.22900477599771));
#22138=CARTESIAN_POINT('Ctrl Pts',(-0.155551992058767,0.00269526028780381,
2.22920519927904));
#22139=CARTESIAN_POINT('Ctrl Pts',(-0.155549959235335,-0.000112613879107687,
2.22940562256037));
#22140=CARTESIAN_POINT('',(-0.155549955602241,0.000117525064441449,2.21559437743963));
#22141=CARTESIAN_POINT('Ctrl Pts',(-0.0636886613526676,0.141913906700877,
2.20284414165342));
#22142=CARTESIAN_POINT('Ctrl Pts',(-0.0715111988820138,0.138403278636249,
2.2034100497518));
#22143=CARTESIAN_POINT('Ctrl Pts',(-0.0790398862705312,0.134247499711388,
2.20397012429285));
#22144=CARTESIAN_POINT('Ctrl Pts',(-0.0879068540018532,0.128344903044612,
2.2046859425461));
#22145=CARTESIAN_POINT('Ctrl Pts',(-0.0895954112005581,0.127171895045403,
2.20482493449157));
#22146=CARTESIAN_POINT('Ctrl Pts',(-0.0943799932002816,0.123705543211883,
2.20522740700976));
#22147=CARTESIAN_POINT('Ctrl Pts',(-0.0974145178887555,0.121330342456775,
2.20549340476745));
#22148=CARTESIAN_POINT('Ctrl Pts',(-0.101075740896878,0.118238659868456,
2.20582989426555));
#22149=CARTESIAN_POINT('Ctrl Pts',(-0.101788398222784,0.117625711489505,
2.20589615703369));
#22150=CARTESIAN_POINT('Ctrl Pts',(-0.102901184799252,0.116650930639211,
2.20600086212419));
#22151=CARTESIAN_POINT('Ctrl Pts',(-0.103305070783896,0.116293403893325,
2.20603912597705));
#22152=CARTESIAN_POINT('Ctrl Pts',(-0.104015383203998,0.115658003018652,
2.2061068886626));
#22153=CARTESIAN_POINT('Ctrl Pts',(-0.104322577905872,0.115380992101588,
2.2061363511242));
#22154=CARTESIAN_POINT('Ctrl Pts',(-0.104631399187023,0.115100272883497,
2.2061661292456));
#22155=CARTESIAN_POINT('Ctrl Pts',(-0.104634136955246,0.115097784067811,
2.20616639324787));
#22156=CARTESIAN_POINT('Ctrl Pts',(-0.104640889228299,0.115091645356859,
2.20616704439912));
#22157=CARTESIAN_POINT('Ctrl Pts',(-0.104644903632025,0.115087995348214,
2.20616743155299));
#22158=CARTESIAN_POINT('Ctrl Pts',(-0.104652854202276,0.115080765706631,
2.20616819836953));
#22159=CARTESIAN_POINT('Ctrl Pts',(-0.104656790775052,0.115077185718859,
2.20616857807037));
#22160=CARTESIAN_POINT('Ctrl Pts',(-0.104664588509522,0.115070093592429,
2.20616933025036));
#22161=CARTESIAN_POINT('Ctrl Pts',(-0.104668449726155,0.115066581417779,
2.20616970273381));
#22162=CARTESIAN_POINT('Ctrl Pts',(-0.104676100009156,0.115059621992719,
2.2061704407907));
#22163=CARTESIAN_POINT('Ctrl Pts',(-0.104679888618601,0.115056175171225,
2.20617080631911));
#22164=CARTESIAN_POINT('Ctrl Pts',(-0.104687395399258,0.115049344934214,
2.20617153062825));
#22165=CARTESIAN_POINT('Ctrl Pts',(-0.104691113576459,0.115045961525789,
2.20617188940868));
#22166=CARTESIAN_POINT('Ctrl Pts',(-0.104698481727184,0.11503925611886,
2.20617260043486));
#22167=CARTESIAN_POINT('Ctrl Pts',(-0.104702131707279,0.115035934126296,
2.20617295268038));
#22168=CARTESIAN_POINT('Ctrl Pts',(-0.104709365611245,0.115029349632079,
2.20617365084146));
#22169=CARTESIAN_POINT('Ctrl Pts',(-0.104712949541064,0.11502608713635,
2.20617399675678));
#22170=CARTESIAN_POINT('Ctrl Pts',(-0.104720053409928,0.115019619789333,
2.2061746824544));
#22171=CARTESIAN_POINT('Ctrl Pts',(-0.104723573353455,0.115016414944757,
2.20617502223637));
#22172=CARTESIAN_POINT('Ctrl Pts',(-0.105127831347595,0.114648311449253,
2.20621404788843));
#22173=CARTESIAN_POINT('Ctrl Pts',(-0.105526654944334,0.114281325353414,
2.20625282199629));
#22174=CARTESIAN_POINT('Ctrl Pts',(-0.106642123400429,0.113244085205233,
2.20636204668078));
#22175=CARTESIAN_POINT('Ctrl Pts',(-0.107354344670884,0.112569133938219,
2.20643269749459));
#22176=CARTESIAN_POINT('Ctrl Pts',(-0.108941506549535,0.111036264817846,
2.20659223388689));
#22177=CARTESIAN_POINT('Ctrl Pts',(-0.109812782152078,0.110174664376795,
2.20668127690867));
#22178=CARTESIAN_POINT('Ctrl Pts',(-0.112517216916863,0.107436310457396,
2.20696237307633));
#22179=CARTESIAN_POINT('Ctrl Pts',(-0.114313044825189,0.105523510066375,
2.20715599037422));
#22180=CARTESIAN_POINT('Ctrl Pts',(-0.120117794830169,0.0990185313458685,
2.20780578091117));
#22181=CARTESIAN_POINT('Ctrl Pts',(-0.123904778622434,0.0942366441679901,
2.20826997121257));
#22182=CARTESIAN_POINT('Ctrl Pts',(-0.130445481279453,0.0848995500202114,
2.20914861857641));
#22183=CARTESIAN_POINT('Ctrl Pts',(-0.13326539983101,0.0804007980511664,
2.20956112426964));
#22184=CARTESIAN_POINT('Ctrl Pts',(-0.139571765628049,0.0690934973332764,
2.21056351081752));
#22185=CARTESIAN_POINT('Ctrl Pts',(-0.142797435609249,0.0621539555417956,
2.2111505004814));
#22186=CARTESIAN_POINT('Ctrl Pts',(-0.145748979178899,0.0543464126688515,
2.21176243539643));
#22187=CARTESIAN_POINT('Ctrl Pts',(-0.145993306996063,0.0536866078690325,
2.21181377997955));
#22188=CARTESIAN_POINT('Ctrl Pts',(-0.146347173762537,0.0527107114756539,
2.2118891555663));
#22189=CARTESIAN_POINT('Ctrl Pts',(-0.146460178799727,0.0523959006432511,
2.21191338413341));
#22190=CARTESIAN_POINT('Ctrl Pts',(-0.146658722849685,0.0518371328317279,
2.21195623186529));
#22191=CARTESIAN_POINT('Ctrl Pts',(-0.146744669875165,0.0515933251039739,
2.21197487491199));
#22192=CARTESIAN_POINT('Ctrl Pts',(-0.146927299827461,0.0510711065216392,
2.21201469352663));
#22193=CARTESIAN_POINT('Ctrl Pts',(-0.1470237992305,0.050792635486859,2.21203585817473));
#22194=CARTESIAN_POINT('Ctrl Pts',(-0.147285969705562,0.0500290753610769,
2.21209370809432));
#22195=CARTESIAN_POINT('Ctrl Pts',(-0.147450037373086,0.0495434329866201,
2.21213030014871));
#22196=CARTESIAN_POINT('Ctrl Pts',(-0.148304511300897,0.04697233393671,
2.21232300623104));
#22197=CARTESIAN_POINT('Ctrl Pts',(-0.148953128010119,0.0448731012644384,
2.212476806311));
#22198=CARTESIAN_POINT('Ctrl Pts',(-0.153522341647447,0.0288921072323438,
2.21362608980931));
#22199=CARTESIAN_POINT('Ctrl Pts',(-0.15553960122566,0.0145385171943701,
2.214541897821));
#22200=CARTESIAN_POINT('Ctrl Pts',(-0.155549959903481,0.00011168717713736,
2.21550711968674));
#22201=CARTESIAN_POINT('Ctrl Pts',(-0.155549955602241,0.000117525064441449,
2.21559437743963));
#22202=CARTESIAN_POINT('Ctrl Pts',(-0.15555774324584,-0.0101897878636815,
2.21633029329905));
#22203=CARTESIAN_POINT('Ctrl Pts',(-0.1545366858615,-0.0205079000756088,
2.21706620915846));
#22204=CARTESIAN_POINT('Ctrl Pts',(-0.152506621271349,-0.0306191601517313,
2.21780212501788));
#22205=CARTESIAN_POINT('Ctrl Pts',(-0.150476759822646,-0.040729408429497,
2.21853796723677));
#22206=CARTESIAN_POINT('Ctrl Pts',(-0.147438301032368,-0.050631944170681,
2.21927380945567));
#22207=CARTESIAN_POINT('Ctrl Pts',(-0.143461944089335,-0.0601204881725731,
2.22000965167456));
#22208=CARTESIAN_POINT('Ctrl Pts',(-0.139475569793138,-0.0696329359883434,
2.22074734764841));
#22209=CARTESIAN_POINT('Ctrl Pts',(-0.134547003388513,-0.0787284847889013,
2.22148504362226));
#22210=CARTESIAN_POINT('Ctrl Pts',(-0.128793764580693,-0.0872236705552636,
2.22222273959611));
#22211=CARTESIAN_POINT('Ctrl Pts',(-0.126922445896272,-0.0899868445487726,
2.22246268518248));
#22212=CARTESIAN_POINT('Ctrl Pts',(-0.124964213903837,-0.092686744913992,
2.22270263076886));
#22213=CARTESIAN_POINT('Ctrl Pts',(-0.122924023262475,-0.0953178210250663,
2.22294257635523));
#22214=CARTESIAN_POINT('Ctrl Pts',(-0.116654882005318,-0.103402647738927,
2.22367988626368));
#22215=CARTESIAN_POINT('Ctrl Pts',(-0.109561201917683,-0.110896634044241,
2.22441719617213));
#22216=CARTESIAN_POINT('Ctrl Pts',(-0.101778418172752,-0.117630591659876,
2.22515450608058));
#22217=CARTESIAN_POINT('Ctrl Pts',(-0.093947197854086,-0.124406458423351,
2.22589640467695));
#22218=CARTESIAN_POINT('Ctrl Pts',(-0.0854188577963193,-0.130412054182867,
2.22663830327332));
#22219=CARTESIAN_POINT('Ctrl Pts',(-0.0763702411659673,-0.135511581660949,
2.22738020186969));
#22220=CARTESIAN_POINT('Ctrl Pts',(-0.0673982786209784,-0.140567909207971,
2.22811581557626));
#22221=CARTESIAN_POINT('Ctrl Pts',(-0.0579156509877826,-0.144733019772496,
2.22885142928283));
#22222=CARTESIAN_POINT('Ctrl Pts',(-0.0481219953059009,-0.147919153823225,
2.22958704298941));
#22223=CARTESIAN_POINT('Ctrl Pts',(-0.0382028280013022,-0.151146120109422,
2.23033208403067));
#22224=CARTESIAN_POINT('Ctrl Pts',(-0.0279655118809678,-0.153368489234519,
2.23107712507194));
#22225=CARTESIAN_POINT('Ctrl Pts',(-0.017632505234266,-0.154547394863723,
2.23182216611321));
#22226=CARTESIAN_POINT('Ctrl Pts',(-0.00729949858756426,-0.155726300492927,
2.23256720715448));
#22227=CARTESIAN_POINT('Ctrl Pts',(0.00312821776256832,-0.155861765045953,
2.23331224819575));
#22228=CARTESIAN_POINT('Ctrl Pts',(0.0134275703953657,-0.154969361014613,
2.23405728923701));
#22229=CARTESIAN_POINT('Ctrl Pts',(0.0236200397669874,-0.15408621805594,
2.23479459848979));
#22230=CARTESIAN_POINT('Ctrl Pts',(0.0337632113016459,-0.152189900448648,
2.23553190774256));
#22231=CARTESIAN_POINT('Ctrl Pts',(0.0436414900225305,-0.149302454261855,
2.23626921699533));
#22232=CARTESIAN_POINT('Ctrl Pts',(0.053581257778395,-0.146397034672549,
2.23701111575562));
#22233=CARTESIAN_POINT('Ctrl Pts',(0.0632518734402264,-0.142488195014809,
2.23775301451591));
#22234=CARTESIAN_POINT('Ctrl Pts',(0.0724433419641342,-0.137650879783122,
2.23849491327619));
#22235=CARTESIAN_POINT('Ctrl Pts',(0.0815569362388782,-0.132854548458485,
2.239230526337));
#22236=CARTESIAN_POINT('Ctrl Pts',(0.0901986504315224,-0.127145872651856,
2.23996613939781));
#22237=CARTESIAN_POINT('Ctrl Pts',(0.0981864910299422,-0.120644997738104,
2.24070175245862));
#22238=CARTESIAN_POINT('Ctrl Pts',(0.106276713916341,-0.114060799372996,
2.24144679406865));
#22239=CARTESIAN_POINT('Ctrl Pts',(0.113695395930814,-0.106664522953298,
2.24219183567868));
#22240=CARTESIAN_POINT('Ctrl Pts',(0.120289247614429,-0.0986220026584063,
2.2429368772887));
#22241=CARTESIAN_POINT('Ctrl Pts',(0.126883099298044,-0.0905794823635131,
2.24368191889873));
#22242=CARTESIAN_POINT('Ctrl Pts',(0.132651607608807,-0.0818915544490725,
2.24442696050876));
#22243=CARTESIAN_POINT('Ctrl Pts',(0.1374868894278,-0.0727540908503969,
2.24517200211879));
#22244=CARTESIAN_POINT('Ctrl Pts',(0.142271992500362,-0.0637114524317446,
2.24590931196561));
#22245=CARTESIAN_POINT('Ctrl Pts',(0.146179090611282,-0.0541608146967772,
2.24664662181244));
#22246=CARTESIAN_POINT('Ctrl Pts',(0.149109795162426,-0.0442952761208154,
2.24738393165927));
#22247=CARTESIAN_POINT('Ctrl Pts',(0.152058739418865,-0.0343683377984613,
2.24812583027104));
#22248=CARTESIAN_POINT('Ctrl Pts',(0.154018655072632,-0.0241234125626051,
2.24886772888282));
#22249=CARTESIAN_POINT('Ctrl Pts',(0.154938635682156,-0.013777578631686,
2.24960962749459));
#22250=CARTESIAN_POINT('Ctrl Pts',(0.155850822686378,-0.00351938931558706,
2.25034524112069));
#22251=CARTESIAN_POINT('Ctrl Pts',(0.155740566749862,0.00683706719978448,
2.25108085474679));
#22252=CARTESIAN_POINT('Ctrl Pts',(0.154610123611401,0.0170737276793156,
2.25181646837289));
#22253=CARTESIAN_POINT('Ctrl Pts',(0.153465192937607,0.0274415791717708,
2.2525615094775));
#22254=CARTESIAN_POINT('Ctrl Pts',(0.151273795230323,0.0376855707696601,
2.25330655058211));
#22255=CARTESIAN_POINT('Ctrl Pts',(0.14809213922491,0.0475869814107803,
2.25405159168673));
#22256=CARTESIAN_POINT('Ctrl Pts',(0.144910483219496,0.0574883920519004,
2.25479663279134));
#22257=CARTESIAN_POINT('Ctrl Pts',(0.140738993323588,0.0670463372042073,
2.25554167389595));
#22258=CARTESIAN_POINT('Ctrl Pts',(0.135683738501421,0.076063957340373,
2.25628671500057));
#22259=CARTESIAN_POINT('Ctrl Pts',(0.130680934045985,0.0849880159252763,
2.25702402599452));
#22260=CARTESIAN_POINT('Ctrl Pts',(0.12477518554404,0.0934498463198428,
2.25776133698848));
#22261=CARTESIAN_POINT('Ctrl Pts',(0.118075381672266,0.101262069616163,
2.25849864798244));
#22262=CARTESIAN_POINT('Ctrl Pts',(0.111333893601457,0.109122898256315,
2.25924054630743));
#22263=CARTESIAN_POINT('Ctrl Pts',(0.103788908687305,0.116325179858639,
2.25998244463242));
#22264=CARTESIAN_POINT('Ctrl Pts',(0.0955952107805158,0.122708427484948,
2.26072434295741));
#22265=CARTESIAN_POINT('Ctrl Pts',(0.0874709096238068,0.129037612019688,
2.26145995775411));
#22266=CARTESIAN_POINT('Ctrl Pts',(0.0787095978315592,0.134561023847159,
2.2621955725508));
#22267=CARTESIAN_POINT('Ctrl Pts',(0.069495716187678,0.139162307869486,
2.2629311873475));
#22268=CARTESIAN_POINT('Ctrl Pts',(0.0601637788311818,0.143822547268624,
2.26367622743664));
#22269=CARTESIAN_POINT('Ctrl Pts',(0.0503684379128092,0.147536380332777,
2.26442126752578));
#22270=CARTESIAN_POINT('Ctrl Pts',(0.0403239423585863,0.150232427167577,
2.26516630761492));
#22271=CARTESIAN_POINT('Ctrl Pts',(0.0302794468043635,0.152928474002378,
2.26591134770406));
#22272=CARTESIAN_POINT('Ctrl Pts',(0.0199867699267357,0.154606611536914,
2.2666563877932));
#22273=CARTESIAN_POINT('Ctrl Pts',(0.00966883048430999,0.155249206816221,
2.26740142788234));
#22274=CARTESIAN_POINT('Ctrl Pts',(-0.000542097669002817,0.155885137494557,
2.26813874087627));
#22275=CARTESIAN_POINT('Ctrl Pts',(-0.0108543084255259,0.155511753195141,
2.26887605387021));
#22276=CARTESIAN_POINT('Ctrl Pts',(-0.021051314719076,0.154118930208454,
2.26961336686414));
#22277=CARTESIAN_POINT('Ctrl Pts',(-0.0312281172117351,0.152728866886466,
2.27034921898569));
#22278=CARTESIAN_POINT('Ctrl Pts',(-0.0412892470449968,0.150323416029473,
2.27108507110724));
#22279=CARTESIAN_POINT('Ctrl Pts',(-0.0510211898583786,0.14694434553747,
2.27182092322879));
#22280=CARTESIAN_POINT('Ctrl Pts',(-0.0553134320620295,0.145454017321099,
2.27214546844985));
#22281=CARTESIAN_POINT('Ctrl Pts',(-0.0595417459102688,0.143774973896094,
2.27247001367092));
#22282=CARTESIAN_POINT('Ctrl Pts',(-0.0636886258329926,0.141913922641526,
2.27279455889198));
#22283=CARTESIAN_POINT('Origin',(0.,0.,-0.129405622560373));
#22284=CARTESIAN_POINT('',(-0.0636886247653984,0.141913923120645,2.35649769913034));
#22285=CARTESIAN_POINT('',(-0.063688625846537,0.141913922635448,2.34279739246514));
#22286=CARTESIAN_POINT('',(-0.0636886258329924,0.141913922641526,-0.129405622560373));
#22287=CARTESIAN_POINT('Ctrl Pts',(-0.0636886247653984,0.141913923120645,
2.35649769913034));
#22288=CARTESIAN_POINT('Ctrl Pts',(-0.0622878305980981,0.142542576406615,
2.35638086051576));
#22289=CARTESIAN_POINT('Ctrl Pts',(-0.0608775885458281,0.143150552227936,
2.35626465169388));
#22290=CARTESIAN_POINT('Ctrl Pts',(-0.0571970067334463,0.144673057726781,
2.35596539343815));
#22291=CARTESIAN_POINT('Ctrl Pts',(-0.0549137229840253,0.145555061980462,
2.35578366821747));
#22292=CARTESIAN_POINT('Ctrl Pts',(-0.0521132765585264,0.146561550106255,
2.3555662784368));
#22293=CARTESIAN_POINT('Ctrl Pts',(-0.0516152280238154,0.146737690526577,
2.35552782542491));
#22294=CARTESIAN_POINT('Ctrl Pts',(-0.0508322066157277,0.147010134817518,
2.35546770811077));
#22295=CARTESIAN_POINT('Ctrl Pts',(-0.050547841690524,0.147108152979743,
2.35544594531707));
#22296=CARTESIAN_POINT('Ctrl Pts',(-0.0500199124173099,0.147288414162136,
2.35540567355351));
#22297=CARTESIAN_POINT('Ctrl Pts',(-0.0497764290221712,0.147370878064146,
2.35538715190662));
#22298=CARTESIAN_POINT('Ctrl Pts',(-0.0492255612363254,0.147555927108912,
2.35534536475117));
#22299=CARTESIAN_POINT('Ctrl Pts',(-0.0489180608026368,0.147658155333656,
2.35532212051625));
#22300=CARTESIAN_POINT('Ctrl Pts',(-0.0479866671592225,0.147964567384768,
2.35525195641379));
#22301=CARTESIAN_POINT('Ctrl Pts',(-0.0473617877156281,0.148165767071775,
2.35520520897835));
#22302=CARTESIAN_POINT('Ctrl Pts',(-0.0425441923930382,0.149683351498874,
2.35484717023235));
#22303=CARTESIAN_POINT('Ctrl Pts',(-0.0382981722067958,0.150825638060988,
2.35454535351134));
#22304=CARTESIAN_POINT('Ctrl Pts',(-0.0335722986047436,0.151884507259909,
2.35421854400406));
#22305=CARTESIAN_POINT('Ctrl Pts',(-0.0331351765354773,0.151980468684479,
2.35418840070296));
#22306=CARTESIAN_POINT('Ctrl Pts',(-0.0180190020082514,0.155230606857872,
2.35314876149821));
#22307=CARTESIAN_POINT('Ctrl Pts',(-0.00296108203843076,0.156244986067882,
2.35219422806468));
#22308=CARTESIAN_POINT('Ctrl Pts',(0.0153514257203747,0.154826909522471,
2.35093757278502));
#22309=CARTESIAN_POINT('Ctrl Pts',(0.0186839142513779,0.154460178197442,
2.35070539853519));
#22310=CARTESIAN_POINT('Ctrl Pts',(0.022839970997147,0.15386635491245,2.3504102954226));
#22311=CARTESIAN_POINT('Ctrl Pts',(0.0236771794885812,0.153739749478231,
2.35035056660114));
#22312=CARTESIAN_POINT('Ctrl Pts',(0.0250279552116814,0.153524185637536,
2.35025372312775));
#22313=CARTESIAN_POINT('Ctrl Pts',(0.025542190667988,0.153439468851789,
2.35021674357695));
#22314=CARTESIAN_POINT('Ctrl Pts',(0.0265068587123853,0.153275562621882,
2.35014715843685));
#22315=CARTESIAN_POINT('Ctrl Pts',(0.0269573878814876,0.153196967614252,
2.3501145721393));
#22316=CARTESIAN_POINT('Ctrl Pts',(0.0279665901151058,0.153016322219819,
2.35004137697733));
#22317=CARTESIAN_POINT('Ctrl Pts',(0.0285250615359366,0.152913197196287,
2.35000073417393));
#22318=CARTESIAN_POINT('Ctrl Pts',(0.0299417563619243,0.152643565186706,
2.34989727636714));
#22319=CARTESIAN_POINT('Ctrl Pts',(0.0307991538417424,0.152472879001992,
2.34983432844281));
#22320=CARTESIAN_POINT('Ctrl Pts',(0.0357306460359825,0.151447850872865,
2.34947029509453));
#22321=CARTESIAN_POINT('Ctrl Pts',(0.0397701946310805,0.150437548705449,
2.34916424549396));
#22322=CARTESIAN_POINT('Ctrl Pts',(0.0457275555419092,0.148690887389623,
2.34870053983961));
#22323=CARTESIAN_POINT('Ctrl Pts',(0.047679444898215,0.148076531622052,
2.34854659782376));
#22324=CARTESIAN_POINT('Ctrl Pts',(0.06328079759921,0.142825571584371,2.3473001368566));
#22325=CARTESIAN_POINT('Ctrl Pts',(0.0762355623586698,0.136351288318933,
2.3461567201094));
#22326=CARTESIAN_POINT('Ctrl Pts',(0.0903257021524403,0.126666013171159,
2.34486886168383));
#22327=CARTESIAN_POINT('Ctrl Pts',(0.0924987625491884,0.125087939784361,
2.34466911782051));
#22328=CARTESIAN_POINT('Ctrl Pts',(0.0950599237290633,0.123124760996137,
2.34443334106692));
#22329=CARTESIAN_POINT('Ctrl Pts',(0.0954880850004677,0.122793002717387,
2.34439391298474));
#22330=CARTESIAN_POINT('Ctrl Pts',(0.0961503586843689,0.122274284993161,
2.34433291844597));
#22331=CARTESIAN_POINT('Ctrl Pts',(0.0963856728034501,0.122088878806069,
2.34431124479288));
#22332=CARTESIAN_POINT('Ctrl Pts',(0.0968218667143772,0.121743150439679,
2.34427106851226));
#22333=CARTESIAN_POINT('Ctrl Pts',(0.0970228824131831,0.12158301214552,
2.3442525536978));
#22334=CARTESIAN_POINT('Ctrl Pts',(0.097476345921773,0.121219921634605,
2.34421078506096));
#22335=CARTESIAN_POINT('Ctrl Pts',(0.097728557500299,0.121016678476366,
2.34418755241403));
#22336=CARTESIAN_POINT('Ctrl Pts',(0.0984685943473138,0.120416501982828,
2.34411937305476));
#22337=CARTESIAN_POINT('Ctrl Pts',(0.0989546573390958,0.120017389779382,
2.34407457893583));
#22338=CARTESIAN_POINT('Ctrl Pts',(0.102366453987248,0.11718110411787,2.34375995322933));
#22339=CARTESIAN_POINT('Ctrl Pts',(0.105204553397637,0.114639915018339,
2.34349715605987));
#22340=CARTESIAN_POINT('Ctrl Pts',(0.108627801617633,0.111340459121465,
2.34317449610659));
#22341=CARTESIAN_POINT('Ctrl Pts',(0.109302826118583,0.110677863138308,
2.34311058143381));
#22342=CARTESIAN_POINT('Ctrl Pts',(0.110760795350055,0.109220389080328,
2.34297178443598));
#22343=CARTESIAN_POINT('Ctrl Pts',(0.111541319238087,0.108423158814631,
2.34289699681766));
#22344=CARTESIAN_POINT('Ctrl Pts',(0.122286387272624,0.0972092565142343,
2.34185949304597));
#22345=CARTESIAN_POINT('Ctrl Pts',(0.13076393203542,0.0854657964949122,
2.34093726750333));
#22346=CARTESIAN_POINT('Ctrl Pts',(0.138925231320378,0.0700344977818755,
2.33973905824407));
#22347=CARTESIAN_POINT('Ctrl Pts',(0.140267774344386,0.0673052753624433,
2.33952794273069));
#22348=CARTESIAN_POINT('Ctrl Pts',(0.141878635797227,0.063772750588508,
2.33925483803145));
#22349=CARTESIAN_POINT('Ctrl Pts',(0.142221646981817,0.0630040799734087,
2.33919542118767));
#22350=CARTESIAN_POINT('Ctrl Pts',(0.14276366953388,0.0617624514560131,
2.33909944405467));
#22351=CARTESIAN_POINT('Ctrl Pts',(0.142966612332954,0.0612912187447158,
2.33906301773306));
#22352=CARTESIAN_POINT('Ctrl Pts',(0.143348760632995,0.0603916460324446,
2.33899347578859));
#22353=CARTESIAN_POINT('Ctrl Pts',(0.143528387257957,0.0599634899591847,
2.3389603748524));
#22354=CARTESIAN_POINT('Ctrl Pts',(0.143934156468139,0.0589840332043454,
2.33888464430861));
#22355=CARTESIAN_POINT('Ctrl Pts',(0.144159052303033,0.058432227341634,
2.33884197327949));
#22356=CARTESIAN_POINT('Ctrl Pts',(0.144736393405761,0.0569920376945332,
2.33873058051624));
#22357=CARTESIAN_POINT('Ctrl Pts',(0.14508382658787,0.0561016855687722,
2.33866169243442));
#22358=CARTESIAN_POINT('Ctrl Pts',(0.147375110664908,0.0500662519809027,
2.33819449695654));
#22359=CARTESIAN_POINT('Ctrl Pts',(0.149052859461297,0.0448250397748916,
2.33778747731663));
#22360=CARTESIAN_POINT('Ctrl Pts',(0.15422980213956,0.0251101363304353,
2.33625021870314));
#22361=CARTESIAN_POINT('Ctrl Pts',(0.155923832282781,0.0102480922114691,
2.33507032285342));
#22362=CARTESIAN_POINT('Ctrl Pts',(0.155404149723066,-0.00721505828116631,
2.33375641176293));
#22363=CARTESIAN_POINT('Ctrl Pts',(0.155262513318454,-0.00980106623130346,
2.33356399780182));
#22364=CARTESIAN_POINT('Ctrl Pts',(0.155013314022462,-0.0129215871342742,
2.33333533037815));
#22365=CARTESIAN_POINT('Ctrl Pts',(0.154967454023022,-0.0134604292336566,
2.33329597209172));
#22366=CARTESIAN_POINT('Ctrl Pts',(0.154891621803753,-0.0142996183530743,
2.3332348853593));
#22367=CARTESIAN_POINT('Ctrl Pts',(0.154863584605737,-0.0146001286745855,
2.33321305236033));
#22368=CARTESIAN_POINT('Ctrl Pts',(0.154809902503556,-0.0151579500788135,
2.33317260510611));
#22369=CARTESIAN_POINT('Ctrl Pts',(0.154784490825486,-0.0154152770317063,
2.33315397846414));
#22370=CARTESIAN_POINT('Ctrl Pts',(0.154725501208146,-0.0159977695661447,
2.33311188642505));
#22371=CARTESIAN_POINT('Ctrl Pts',(0.154691539962111,-0.0163228926562672,
2.33308844272013));
#22372=CARTESIAN_POINT('Ctrl Pts',(0.154585569263784,-0.0173073443193214,
2.33301760251964));
#22373=CARTESIAN_POINT('Ctrl Pts',(0.154510366320208,-0.017966333338465,
2.33297038054363));
#22374=CARTESIAN_POINT('Ctrl Pts',(0.153892301836982,-0.0230911183375703,
2.33260454883558));
#22375=CARTESIAN_POINT('Ctrl Pts',(0.153160089114337,-0.0275324712237907,
2.33229577604474));
#22376=CARTESIAN_POINT('Ctrl Pts',(0.149143960590367,-0.0466768288702718,
2.33097646186338));
#22377=CARTESIAN_POINT('Ctrl Pts',(0.1439274079896,-0.060890029549738,2.33001919513146));
#22378=CARTESIAN_POINT('Ctrl Pts',(0.135037290984816,-0.0772892468845399,
2.32874492216824));
#22379=CARTESIAN_POINT('Ctrl Pts',(0.133217216620147,-0.0803857409580274,
2.32849644056927));
#22380=CARTESIAN_POINT('Ctrl Pts',(0.130815578221392,-0.0841657616905167,
2.3281816507435));
#22381=CARTESIAN_POINT('Ctrl Pts',(0.130333003175463,-0.0849111251320017,
2.32811900702467));
#22382=CARTESIAN_POINT('Ctrl Pts',(0.129556330041332,-0.0860885179992524,
2.32801911913909));
#22383=CARTESIAN_POINT('Ctrl Pts',(0.129266385106025,-0.0865232757966593,
2.32798203019436));
#22384=CARTESIAN_POINT('Ctrl Pts',(0.128716357150386,-0.0873390790886988,
2.32791204288386));
#22385=CARTESIAN_POINT('Ctrl Pts',(0.128456758294247,-0.0877204455884917,
2.32787916301725));
#22386=CARTESIAN_POINT('Ctrl Pts',(0.127868917245048,-0.0885758145443564,
2.32780504613579));
#22387=CARTESIAN_POINT('Ctrl Pts',(0.127539729985038,-0.0890491559668797,
2.32776377357674));
#22388=CARTESIAN_POINT('Ctrl Pts',(0.126693074955339,-0.0902522440487524,
2.32765820373673));
#22389=CARTESIAN_POINT('Ctrl Pts',(0.126171935609659,-0.0909793679898886,
2.32759376672507));
#22390=CARTESIAN_POINT('Ctrl Pts',(0.123043202073309,-0.0952661731389925,
2.32721004747348));
#22391=CARTESIAN_POINT('Ctrl Pts',(0.120291626198591,-0.0987177326470451,
2.32688521268492));
#22392=CARTESIAN_POINT('Ctrl Pts',(0.116402704292327,-0.103191625078317,
2.32644162287713));
#22393=CARTESIAN_POINT('Ctrl Pts',(0.115391433353489,-0.104321224599612,
2.32632757795555));
#22394=CARTESIAN_POINT('Ctrl Pts',(0.104395121950214,-0.116248672770863,
2.32510136923459));
#22395=CARTESIAN_POINT('Ctrl Pts',(0.0929450050055603,-0.125591580949708,
2.32393492748763));
#22396=CARTESIAN_POINT('Ctrl Pts',(0.0781478439210853,-0.134518993348186,
2.32263501971058));
#22397=CARTESIAN_POINT('Ctrl Pts',(0.0759081183462432,-0.135795451921587,
2.32244347278898));
#22398=CARTESIAN_POINT('Ctrl Pts',(0.0731633907447485,-0.137270574046965,
2.32221584288785));
#22399=CARTESIAN_POINT('Ctrl Pts',(0.0726879201603291,-0.137522938196781,
2.32217666349231));
#22400=CARTESIAN_POINT('Ctrl Pts',(0.0719450993619771,-0.13791227428643,
2.32211585827971));
#22401=CARTESIAN_POINT('Ctrl Pts',(0.071678652575637,-0.138050945270857,
2.32209412825292));
#22402=CARTESIAN_POINT('Ctrl Pts',(0.0711829088526831,-0.138307130586625,
2.32205384968041));
#22403=CARTESIAN_POINT('Ctrl Pts',(0.0709537238005797,-0.138424845907807,
2.3220352889418));
#22404=CARTESIAN_POINT('Ctrl Pts',(0.0704339850649211,-0.138690167106335,
2.32199333287592));
#22405=CARTESIAN_POINT('Ctrl Pts',(0.0701432599400468,-0.138837429371094,
2.32196995923314));
#22406=CARTESIAN_POINT('Ctrl Pts',(0.0692617996533039,-0.139280443848806,
2.32189937304643));
#22407=CARTESIAN_POINT('Ctrl Pts',(0.0686696307340983,-0.139573352709093,
2.32185233407845));
#22408=CARTESIAN_POINT('Ctrl Pts',(0.0640737093931769,-0.141810336390388,
2.32149005601268));
#22409=CARTESIAN_POINT('Ctrl Pts',(0.059989579155983,-0.143585763411402,
2.32118447340646));
#22410=CARTESIAN_POINT('Ctrl Pts',(0.0420295968950637,-0.15049277568158,
2.31988629511711));
#22411=CARTESIAN_POINT('Ctrl Pts',(0.0275381540075679,-0.153805918183178,
2.31894590935921));
#22412=CARTESIAN_POINT('Ctrl Pts',(0.00892024207663318,-0.155342707186809,
2.3176730678394));
#22413=CARTESIAN_POINT('Ctrl Pts',(0.00503402763356657,-0.15551714240138,
2.31740444208039));
#22414=CARTESIAN_POINT('Ctrl Pts',(0.000236148989807116,-0.155552479634794,
2.31706732785458));
#22415=CARTESIAN_POINT('Ctrl Pts',(-0.000673348055767362,-0.15555120130186,
2.3170031839142));
#22416=CARTESIAN_POINT('Ctrl Pts',(-0.00210956804403887,-0.15553658660679,
2.31690149064174));
#22417=CARTESIAN_POINT('Ctrl Pts',(-0.00263633488942848,-0.155528549715288,
2.31686410706024));
#22418=CARTESIAN_POINT('Ctrl Pts',(-0.00362299322545797,-0.155508482276909,
2.31679392159595));
#22419=CARTESIAN_POINT('Ctrl Pts',(-0.0040828931970336,-0.155497087158457,
2.31676113994206));
#22420=CARTESIAN_POINT('Ctrl Pts',(-0.00511087117510107,-0.15546705295409,
2.31668771276117));
#22421=CARTESIAN_POINT('Ctrl Pts',(-0.00567890867194311,-0.155447340082818,
2.31664703409218));
#22422=CARTESIAN_POINT('Ctrl Pts',(-0.00711571039481541,-0.155389592181557,
2.3165438700161));
#22423=CARTESIAN_POINT('Ctrl Pts',(-0.007984277411045,-0.155347384753823,
2.31648125508628));
#22424=CARTESIAN_POINT('Ctrl Pts',(-0.01288900493283,-0.15506780111924,
2.31612621134544));
#22425=CARTESIAN_POINT('Ctrl Pts',(-0.016914694462103,-0.15468043474138,
2.31582914032079));
#22426=CARTESIAN_POINT('Ctrl Pts',(-0.0334724592352452,-0.15243311160776,
2.31458243592057));
#22427=CARTESIAN_POINT('Ctrl Pts',(-0.045768055606153,-0.149202703142092,
2.31359213945788));
#22428=CARTESIAN_POINT('Ctrl Pts',(-0.0616041272279759,-0.142898327077771,
2.31227748502557));
#22429=CARTESIAN_POINT('Ctrl Pts',(-0.0656049953992499,-0.141106311662637,
2.31194231365037));
#22430=CARTESIAN_POINT('Ctrl Pts',(-0.0714850425700971,-0.138168344186125,
2.31144993863582));
#22431=CARTESIAN_POINT('Ctrl Pts',(-0.0734241700131549,-0.137147713228804,
2.3112876122622));
#22432=CARTESIAN_POINT('Ctrl Pts',(-0.0757890541065996,-0.135838447462043,
2.31109027544619));
#22433=CARTESIAN_POINT('Ctrl Pts',(-0.0762356743359717,-0.135588297834739,
2.31105303571891));
#22434=CARTESIAN_POINT('Ctrl Pts',(-0.0769372110193267,-0.13519080862986,
2.31099459507163));
#22435=CARTESIAN_POINT('Ctrl Pts',(-0.0771929524300621,-0.135044945394115,
2.31097330228848));
#22436=CARTESIAN_POINT('Ctrl Pts',(-0.0776724937269196,-0.13476962959015,
2.31093339985487));
#22437=CARTESIAN_POINT('Ctrl Pts',(-0.0778963821967603,-0.134640346789623,
2.3109147802163));
#22438=CARTESIAN_POINT('Ctrl Pts',(-0.0784093972709849,-0.134342401928793,
2.31087213694262));
#22439=CARTESIAN_POINT('Ctrl Pts',(-0.0786983024056535,-0.134173364497457,
2.31084813786164));
#22440=CARTESIAN_POINT('Ctrl Pts',(-0.0795934567921234,-0.133645726680182,
2.3107738192145));
#22441=CARTESIAN_POINT('Ctrl Pts',(-0.0801978292286563,-0.133283933244755,
2.31072370082422));
#22442=CARTESIAN_POINT('Ctrl Pts',(-0.0870062445747519,-0.129145155782385,
2.31015952041146));
#22443=CARTESIAN_POINT('Ctrl Pts',(-0.0929418963855798,-0.124941566437214,
2.30967142059025));
#22444=CARTESIAN_POINT('Ctrl Pts',(-0.105657439832881,-0.114526892973744,
2.30858204222566));
#22445=CARTESIAN_POINT('Ctrl Pts',(-0.112224199928664,-0.108100100314215,
2.30798608777209));
#22446=CARTESIAN_POINT('Ctrl Pts',(-0.120941984603689,-0.0979122061325489,
2.30708826970452));
#22447=CARTESIAN_POINT('Ctrl Pts',(-0.123564454556539,-0.0945811009747796,
2.30680123264976));
#22448=CARTESIAN_POINT('Ctrl Pts',(-0.127569356035594,-0.0890427263891966,
2.30633019370055));
#22449=CARTESIAN_POINT('Ctrl Pts',(-0.129038175931453,-0.0869004919454911,
2.30614941239417));
#22450=CARTESIAN_POINT('Ctrl Pts',(-0.130885742992438,-0.08405567896223,
2.30591062617438));
#22451=CARTESIAN_POINT('Ctrl Pts',(-0.131313746553809,-0.0833854592141237,
2.3058544612963));
#22452=CARTESIAN_POINT('Ctrl Pts',(-0.13200353461866,-0.0822868238743171,
2.30576252840975));
#22453=CARTESIAN_POINT('Ctrl Pts',(-0.132268421278512,-0.0818603643826864,
2.30572687512221));
#22454=CARTESIAN_POINT('Ctrl Pts',(-0.132775237377736,-0.0810355235260071,
2.30565797433472));
#22455=CARTESIAN_POINT('Ctrl Pts',(-0.133017450188594,-0.0806373218211241,
2.30562473767779));
#22456=CARTESIAN_POINT('Ctrl Pts',(-0.13356984545034,-0.0797199139045481,
2.30554822052624));
#22457=CARTESIAN_POINT('Ctrl Pts',(-0.133878794969277,-0.079199978062087,
2.30550489579634));
#22458=CARTESIAN_POINT('Ctrl Pts',(-0.134695533067784,-0.0778070423704681,
2.30538892728303));
#22459=CARTESIAN_POINT('Ctrl Pts',(-0.135197857267318,-0.07693088958118,
2.30531608809641));
#22460=CARTESIAN_POINT('Ctrl Pts',(-0.139159029865383,-0.0698631922559838,
2.3047292527764));
#22461=CARTESIAN_POINT('Ctrl Pts',(-0.142198727525374,-0.063447572256919,
2.30420049045902));
#22462=CARTESIAN_POINT('Ctrl Pts',(-0.147965869834655,-0.0487588297400476,
2.30299830421891));
#22463=CARTESIAN_POINT('Ctrl Pts',(-0.150458203950497,-0.0404182165755456,
2.30232084932417));
#22464=CARTESIAN_POINT('Ctrl Pts',(-0.153666102340847,-0.0251153907349569,
2.30111260790511));
#22465=CARTESIAN_POINT('Ctrl Pts',(-0.154634474418508,-0.0182280067856629,
2.30058131794673));
#22466=CARTESIAN_POINT('Ctrl Pts',(-0.15518748566797,-0.010634362502773,
2.30002357022452));
#22467=CARTESIAN_POINT('Ctrl Pts',(-0.155231563393175,-0.00997031309190796,
2.29997503237368));
#22468=CARTESIAN_POINT('Ctrl Pts',(-0.155290953329751,-0.00897938553177951,
2.29990297366899));
#22469=CARTESIAN_POINT('Ctrl Pts',(-0.155309497394042,-0.00865272067933687,
2.29987927934808));
#22470=CARTESIAN_POINT('Ctrl Pts',(-0.155339510580998,-0.00809280462923168,
2.29983877232926));
#22471=CARTESIAN_POINT('Ctrl Pts',(-0.155351485262566,-0.00785958421389333,
2.29982193162328));
#22472=CARTESIAN_POINT('Ctrl Pts',(-0.155377199402237,-0.00733573818004885,
2.29978417653917));
#22473=CARTESIAN_POINT('Ctrl Pts',(-0.155390648711314,-0.00704510082247598,
2.29976327857965));
#22474=CARTESIAN_POINT('Ctrl Pts',(-0.155424784455485,-0.0062597183010564,
2.29970693499892));
#22475=CARTESIAN_POINT('Ctrl Pts',(-0.155443924299087,-0.00576490352588302,
2.29967157455729));
#22476=CARTESIAN_POINT('Ctrl Pts',(-0.155519581091093,-0.00353308850723159,
2.29951267115722));
#22477=CARTESIAN_POINT('Ctrl Pts',(-0.155549351313571,-0.00179521709333132,
2.29939053766916));
#22478=CARTESIAN_POINT('Ctrl Pts',(-0.155551162562828,0.00313761411625181,
2.29904747749142));
#22479=CARTESIAN_POINT('Ctrl Pts',(-0.155453913840257,0.00633186507260315,
2.29882961760291));
#22480=CARTESIAN_POINT('Ctrl Pts',(-0.154565299748118,0.0208223160512951,
2.29785168407958));
#22481=CARTESIAN_POINT('Ctrl Pts',(-0.15264043241771,0.0320144805920024,
2.29712269225997));
#22482=CARTESIAN_POINT('Ctrl Pts',(-0.147644349853505,0.049427503961895,
2.2959131258933));
#22483=CARTESIAN_POINT('Ctrl Pts',(-0.145345904140758,0.0558254485291349,
2.29545178914122));
#22484=CARTESIAN_POINT('Ctrl Pts',(-0.142237316937904,0.062971043102483,
2.29490586140212));
#22485=CARTESIAN_POINT('Ctrl Pts',(-0.141828717961668,0.0638860022015219,
2.29483536976228));
#22486=CARTESIAN_POINT('Ctrl Pts',(-0.141160391942814,0.0653445413663976,
2.29472202109309));
#22487=CARTESIAN_POINT('Ctrl Pts',(-0.140906292577498,0.065890682447694,
2.29467935677631));
#22488=CARTESIAN_POINT('Ctrl Pts',(-0.140450196798941,0.0668562745815855,
2.29460352438548));
#22489=CARTESIAN_POINT('Ctrl Pts',(-0.140249476154686,0.0672763231865496,
2.29457040065216));
#22490=CARTESIAN_POINT('Ctrl Pts',(-0.139828065169565,0.0681481289365589,
2.2945013671757));
#22491=CARTESIAN_POINT('Ctrl Pts',(-0.139607064439,0.0685997291131404,2.29446544696394));
#22492=CARTESIAN_POINT('Ctrl Pts',(-0.13902908301142,0.0697664345199909,
2.2943722259436));
#22493=CARTESIAN_POINT('Ctrl Pts',(-0.138668777080451,0.0704798661135457,
2.2943148096748));
#22494=CARTESIAN_POINT('Ctrl Pts',(-0.137096615368179,0.0735341323943068,
2.29406719813965));
#22495=CARTESIAN_POINT('Ctrl Pts',(-0.135830931378845,0.0758466022510134,
2.29387512241506));
#22496=CARTESIAN_POINT('Ctrl Pts',(-0.132333980292388,0.0818672225739584,
2.29336233840094));
#22497=CARTESIAN_POINT('Ctrl Pts',(-0.130005813280161,0.0855161193777704,
2.29303835140121));
#22498=CARTESIAN_POINT('Ctrl Pts',(-0.120413358372476,0.0992515071173619,
2.29176696873169));
#22499=CARTESIAN_POINT('Ctrl Pts',(-0.112103539956648,0.108549482409988,
2.29078831055915));
#22500=CARTESIAN_POINT('Ctrl Pts',(-0.102205596553945,0.117262088814938,
2.28978386143935));
#22501=CARTESIAN_POINT('Ctrl Pts',(-0.10163077149136,0.117760637582091,
2.28972605354729));
#22502=CARTESIAN_POINT('Ctrl Pts',(-0.0985673771601378,0.120378397205244,
2.28942083866504));
#22503=CARTESIAN_POINT('Ctrl Pts',(-0.096015895619844,0.122423192972991,
2.28917651209152));
#22504=CARTESIAN_POINT('Ctrl Pts',(-0.0929618957269405,0.124716441781122,
2.2888970624849));
#22505=CARTESIAN_POINT('Ctrl Pts',(-0.0925203961023893,0.125044317092071,
2.28885697162915));
#22506=CARTESIAN_POINT('Ctrl Pts',(-0.0918089232626336,0.125566854184183,
2.28879286946916));
#22507=CARTESIAN_POINT('Ctrl Pts',(-0.0915400534011034,0.125762998888008,
2.28876875939932));
#22508=CARTESIAN_POINT('Ctrl Pts',(-0.0910608181521888,0.126110257245867,
2.28872599163525));
#22509=CARTESIAN_POINT('Ctrl Pts',(-0.0908507028094057,0.126261709905648,
2.28870731076351));
#22510=CARTESIAN_POINT('Ctrl Pts',(-0.0904025387994706,0.12658305180383,
2.28866761548282));
#22511=CARTESIAN_POINT('Ctrl Pts',(-0.0901643895298115,0.126752794406786,
2.28864661112834));
#22512=CARTESIAN_POINT('Ctrl Pts',(-0.0895159781805926,0.12721220211381,
2.28858966017326));
#22513=CARTESIAN_POINT('Ctrl Pts',(-0.0891047848199081,0.127500557085662,
2.28855380199679));
#22514=CARTESIAN_POINT('Ctrl Pts',(-0.0869996819098929,0.12896163147066,
2.28837149523992));
#22515=CARTESIAN_POINT('Ctrl Pts',(-0.0852838866305113,0.130102678055038,
2.28822707448014));
#22516=CARTESIAN_POINT('Ctrl Pts',(-0.080180324903344,0.133352302910331,
2.2878079733219));
#22517=CARTESIAN_POINT('Ctrl Pts',(-0.0767333407592146,0.135365139240659,
2.2875380941227));
#22518=CARTESIAN_POINT('Ctrl Pts',(-0.0700901186741811,0.138908967681779,
2.28703496338495));
#22519=CARTESIAN_POINT('Ctrl Pts',(-0.0669135888792809,0.140466612944173,
2.28680131598053));
#22520=CARTESIAN_POINT('Ctrl Pts',(-0.0636886081915498,0.141913930558713,
2.28656840831392));
#22521=CARTESIAN_POINT('',(-0.155549964955187,-0.000104414750328626,2.28559437743963));
#22522=CARTESIAN_POINT('Ctrl Pts',(-0.0636886258329926,0.141913922641526,
2.27279455889198));
#22523=CARTESIAN_POINT('Ctrl Pts',(-0.0730870322701466,0.13769607297702,
2.27353010174628));
#22524=CARTESIAN_POINT('Ctrl Pts',(-0.0820652852127109,0.132540364111075,
2.27426564460058));
#22525=CARTESIAN_POINT('Ctrl Pts',(-0.0904363479891319,0.126558561395066,
2.27500118745488));
#22526=CARTESIAN_POINT('Ctrl Pts',(-0.0988275156773907,0.120562392090315,
2.27573849687391));
#22527=CARTESIAN_POINT('Ctrl Pts',(-0.106607849649866,0.113736743601892,
2.27647580629294));
#22528=CARTESIAN_POINT('Ctrl Pts',(-0.113622041823003,0.106234806499431,
2.27721311571197));
#22529=CARTESIAN_POINT('Ctrl Pts',(-0.117754033036061,0.101815489574099,
2.27764745739602));
#22530=CARTESIAN_POINT('Ctrl Pts',(-0.121620840829677,0.0971622129555324,
2.27808179908007));
#22531=CARTESIAN_POINT('Ctrl Pts',(-0.125197443581938,0.0923114436055868,
2.27851614076412));
#22532=CARTESIAN_POINT('Ctrl Pts',(-0.131302103576993,0.0840319953003109,
2.27925748904529));
#22533=CARTESIAN_POINT('Ctrl Pts',(-0.136604901482101,0.0751133412550397,
2.27999883732645));
#22534=CARTESIAN_POINT('Ctrl Pts',(-0.140978435979441,0.0657334244413799,
2.28074018560762));
#22535=CARTESIAN_POINT('Ctrl Pts',(-0.145341634266567,0.0563756756915671,
2.28147978182037));
#22536=CARTESIAN_POINT('Ctrl Pts',(-0.14877946960056,0.046559610988197,
2.28221937803311));
#22537=CARTESIAN_POINT('Ctrl Pts',(-0.151209668956078,0.0364888820628031,
2.28295897424586));
#22538=CARTESIAN_POINT('Ctrl Pts',(-0.15363754951923,0.0264277621965591,
2.28369786476751));
#22539=CARTESIAN_POINT('Ctrl Pts',(-0.155059453099014,0.0161133364418129,
2.28443675528916));
#22540=CARTESIAN_POINT('Ctrl Pts',(-0.155443196067471,0.00576327132190011,
2.28517564581081));
#22541=CARTESIAN_POINT('Ctrl Pts',(-0.155515685524535,0.00380813295380514,
2.28531522302041));
#22542=CARTESIAN_POINT('Ctrl Pts',(-0.155551278048855,0.00185174253079008,
2.28545480023002));
#22543=CARTESIAN_POINT('Ctrl Pts',(-0.155549964955187,-0.000104414750328626,
2.28559437743963));
#22544=CARTESIAN_POINT('Ctrl Pts',(-0.0636886258465365,0.141913922635448,
2.34279739246514));
#22545=CARTESIAN_POINT('Ctrl Pts',(-0.0530015079944167,0.146710124710772,
2.3418890487664));
#22546=CARTESIAN_POINT('Ctrl Pts',(-0.0418044881726883,0.150284807036787,
2.34099118900849));
#22547=CARTESIAN_POINT('Ctrl Pts',(-0.0286036919340213,0.15290735101411,
2.34000864466546));
#22548=CARTESIAN_POINT('Ctrl Pts',(-0.0268916737630272,0.15321771283392,
2.33988254320508));
#22549=CARTESIAN_POINT('Ctrl Pts',(-0.024481200040181,0.153613043989164,
2.33970677757529));
#22550=CARTESIAN_POINT('Ctrl Pts',(-0.0237868842987554,0.153722088863226,
2.33965635601679));
#22551=CARTESIAN_POINT('Ctrl Pts',(-0.0226632431977504,0.153890765625645,
2.33957508212066));
#22552=CARTESIAN_POINT('Ctrl Pts',(-0.0222343727673696,0.153953314390246,
2.33954413803104));
#22553=CARTESIAN_POINT('Ctrl Pts',(-0.0213406382486043,0.154079848919459,
2.33947980943997));
#22554=CARTESIAN_POINT('Ctrl Pts',(-0.0208757341446579,0.15414352538027,
2.33944643499923));
#22555=CARTESIAN_POINT('Ctrl Pts',(-0.0197772878657009,0.154288915427545,
2.33936778390241));
#22556=CARTESIAN_POINT('Ctrl Pts',(-0.0191435127150886,0.154368832612304,
2.33932256421805));
#22557=CARTESIAN_POINT('Ctrl Pts',(-0.0170448491715186,0.154620344392983,
2.33917333871667));
#22558=CARTESIAN_POINT('Ctrl Pts',(-0.0155779793154829,0.154775012862032,
2.33906986456883));
#22559=CARTESIAN_POINT('Ctrl Pts',(-0.00783451502552429,0.15548028722424,
2.33852764030594));
#22560=CARTESIAN_POINT('Ctrl Pts',(-0.00153053058273112,0.155670074982046,
2.33810038589204));
#22561=CARTESIAN_POINT('Ctrl Pts',(0.0124127457534963,0.15524245276642,
2.33716937993307));
#22562=CARTESIAN_POINT('Ctrl Pts',(0.0200295063764908,0.154444543425745,
2.33667024015484));
#22563=CARTESIAN_POINT('Ctrl Pts',(0.0323143233411157,0.152233224586033,
2.33584586065423));
#22564=CARTESIAN_POINT('Ctrl Pts',(0.037029046826082,0.151155593218615,
2.33552451551866));
#22565=CARTESIAN_POINT('Ctrl Pts',(0.0450544662884326,0.148923218548605,
2.33495748521316));
#22566=CARTESIAN_POINT('Ctrl Pts',(0.0483904535159426,0.147872881621639,
2.33471560034705));
#22567=CARTESIAN_POINT('Ctrl Pts',(0.0522164532777445,0.146524941819857,
2.3344278489321));
#22568=CARTESIAN_POINT('Ctrl Pts',(0.0527440054880084,0.146335868561983,
2.33438794029564));
#22569=CARTESIAN_POINT('Ctrl Pts',(0.0535858805145219,0.146028999106245,
2.334323864636));
#22570=CARTESIAN_POINT('Ctrl Pts',(0.0539008703363946,0.145913026634763,
2.33429980311827));
#22571=CARTESIAN_POINT('Ctrl Pts',(0.0544584136093846,0.145705699495882,
2.33425705402176));
#22572=CARTESIAN_POINT('Ctrl Pts',(0.054701117101631,0.145614757029952,
2.33423839116031));
#22573=CARTESIAN_POINT('Ctrl Pts',(0.055215384782725,0.14542059064302,2.33419873055255));
#22574=CARTESIAN_POINT('Ctrl Pts',(0.0554868831893145,0.145317214017533,
2.33417772424008));
#22575=CARTESIAN_POINT('Ctrl Pts',(0.0562188328229594,0.145036164183714,
2.33412091076026));
#22576=CARTESIAN_POINT('Ctrl Pts',(0.0566787252806646,0.144857061159592,
2.33408502016328));
#22577=CARTESIAN_POINT('Ctrl Pts',(0.0589552135095668,0.143957992794488,
2.3339064231794));
#22578=CARTESIAN_POINT('Ctrl Pts',(0.0607588781406035,0.14320607057419,
2.33376195469208));
#22579=CARTESIAN_POINT('Ctrl Pts',(0.0659237938550596,0.140937758068222,
2.3333405802116));
#22580=CARTESIAN_POINT('Ctrl Pts',(0.0692457653622815,0.139335630751505,
2.33306003069803));
#22581=CARTESIAN_POINT('Ctrl Pts',(0.0790024955367837,0.134195026847908,
2.33221302313821));
#22582=CARTESIAN_POINT('Ctrl Pts',(0.085247107347394,0.130317421189606,
2.33164029131531));
#22583=CARTESIAN_POINT('Ctrl Pts',(0.0930193405561323,0.124692737036863,
2.33090008741605));
#22584=CARTESIAN_POINT('Ctrl Pts',(0.0948152934516282,0.123332627707784,
2.33072692548805));
#22585=CARTESIAN_POINT('Ctrl Pts',(0.102673874001872,0.117108024289342,
2.32996039764098));
#22586=CARTESIAN_POINT('Ctrl Pts',(0.10839717868291,0.111831581951046,2.32937894396787));
#22587=CARTESIAN_POINT('Ctrl Pts',(0.114402229443738,0.105399159905103,
2.32874142540456));
#22588=CARTESIAN_POINT('Ctrl Pts',(0.11509425129291,0.104643042880166,2.32866748840836));
#22589=CARTESIAN_POINT('Ctrl Pts',(0.116185522574125,0.103426775166139,
2.32855011857869));
#22590=CARTESIAN_POINT('Ctrl Pts',(0.116589619494865,0.10297103535781,2.32850648274694));
#22591=CARTESIAN_POINT('Ctrl Pts',(0.117298563479992,0.10216196578903,2.32842961377933));
#22592=CARTESIAN_POINT('Ctrl Pts',(0.117604514672402,0.101809618336083,
2.3283963350043));
#22593=CARTESIAN_POINT('Ctrl Pts',(0.118234957400573,0.101076937454874,
2.32832753835453));
#22594=CARTESIAN_POINT('Ctrl Pts',(0.11855921061435,0.100696405228326,2.32829203053596));
#22595=CARTESIAN_POINT('Ctrl Pts',(0.119388660875931,0.0997134308705711,
2.32820087444282));
#22596=CARTESIAN_POINT('Ctrl Pts',(0.119891139884938,0.0991087042572439,
2.32814533723447));
#22597=CARTESIAN_POINT('Ctrl Pts',(0.121983560761576,0.0965513029354718,
2.32791269533805));
#22598=CARTESIAN_POINT('Ctrl Pts',(0.123530616193694,0.0945639006882726,
2.32773731260164));
#22599=CARTESIAN_POINT('Ctrl Pts',(0.127445153977421,0.0892750357863676,
2.32728348013581));
#22600=CARTESIAN_POINT('Ctrl Pts',(0.129732833737647,0.0859167929890493,
2.32700795256521));
#22601=CARTESIAN_POINT('Ctrl Pts',(0.136152312607891,0.0756510449344167,
2.32619597017108));
#22602=CARTESIAN_POINT('Ctrl Pts',(0.139882407007321,0.0685087653338176,
2.32567043438522));
#22603=CARTESIAN_POINT('Ctrl Pts',(0.144786099957893,0.057030399456948,
2.32484688521895));
#22604=CARTESIAN_POINT('Ctrl Pts',(0.146353467827657,0.052878534115516,
2.32455279974261));
#22605=CARTESIAN_POINT('Ctrl Pts',(0.149081033426038,0.0445980727842855,
2.32396371123359));
#22606=CARTESIAN_POINT('Ctrl Pts',(0.150252173729564,0.0404773829726443,
2.32366933549607));
#22607=CARTESIAN_POINT('Ctrl Pts',(0.151402869711126,0.0356846278700788,
2.32331994877204));
#22608=CARTESIAN_POINT('Ctrl Pts',(0.151550073666467,0.0350541974024073,
2.32327385317321));
#22609=CARTESIAN_POINT('Ctrl Pts',(0.151765892115636,0.0341031375527303,
2.32320408076961));
#22610=CARTESIAN_POINT('Ctrl Pts',(0.151837437635468,0.0337831692936692,
2.32318056736433));
#22611=CARTESIAN_POINT('Ctrl Pts',(0.151963473478506,0.0332110191631024,
2.32313844720577));
#22612=CARTESIAN_POINT('Ctrl Pts',(0.15201834853869,0.0329589255192188,
2.32311986270344));
#22613=CARTESIAN_POINT('Ctrl Pts',(0.152135535614555,0.0324140540885293,
2.32307963711892));
#22614=CARTESIAN_POINT('Ctrl Pts',(0.152197628880029,0.0321212368744975,
2.32305798431743));
#22615=CARTESIAN_POINT('Ctrl Pts',(0.152368024104424,0.0313061060122979,
2.32299761344817));
#22616=CARTESIAN_POINT('Ctrl Pts',(0.152474483631643,0.0307834186205562,
2.32295879359515));
#22617=CARTESIAN_POINT('Ctrl Pts',(0.153064466997916,0.0278085996563416,
2.32273727937973));
#22618=CARTESIAN_POINT('Ctrl Pts',(0.15349148794031,0.0253458175261111,
2.32255167809452));
#22619=CARTESIAN_POINT('Ctrl Pts',(0.156034164148296,0.00824285191596339,
2.32125220228198));
#22620=CARTESIAN_POINT('Ctrl Pts',(0.156111509125902,-0.00662412420394627,
2.32007857379173));
#22621=CARTESIAN_POINT('Ctrl Pts',(0.153840848749251,-0.0230661747018645,
2.31882428925722));
#22622=CARTESIAN_POINT('Ctrl Pts',(0.153563063333852,-0.0248483637352175,
2.31868877315135));
#22623=CARTESIAN_POINT('Ctrl Pts',(0.152547371719703,-0.0306946330303252,
2.31824574247194));
#22624=CARTESIAN_POINT('Ctrl Pts',(0.151678561686477,-0.0347344355171594,
2.31794208325195));
#22625=CARTESIAN_POINT('Ctrl Pts',(0.150431745102537,-0.0395835804017798,
2.31758019106565));
#22626=CARTESIAN_POINT('Ctrl Pts',(0.150206451356824,-0.0404300853469675,
2.31751711082726));
#22627=CARTESIAN_POINT('Ctrl Pts',(0.149822617567476,-0.0418247690743199,
2.31741332415453));
#22628=CARTESIAN_POINT('Ctrl Pts',(0.149668193027019,-0.0423740493103708,
2.31737248574901));
#22629=CARTESIAN_POINT('Ctrl Pts',(0.1493836748254,-0.0433651042254198,
2.31729886369866));
#22630=CARTESIAN_POINT('Ctrl Pts',(0.14925463562904,-0.0438071720205702,
2.31726604632634));
#22631=CARTESIAN_POINT('Ctrl Pts',(0.148974021448409,-0.0447528775388686,
2.31719588548058));
#22632=CARTESIAN_POINT('Ctrl Pts',(0.148821851098604,-0.0452563339485949,
2.31715856180815));
#22633=CARTESIAN_POINT('Ctrl Pts',(0.148401082425138,-0.0466233754167217,
2.31705728374322));
#22634=CARTESIAN_POINT('Ctrl Pts',(0.148127498366406,-0.0474854155467141,
2.31699349245682));
#22635=CARTESIAN_POINT('Ctrl Pts',(0.146661483065464,-0.0519687111838243,
2.31666203787263));
#22636=CARTESIAN_POINT('Ctrl Pts',(0.14534366354283,-0.0555478277151331,
2.31639853774858));
#22637=CARTESIAN_POINT('Ctrl Pts',(0.138254173709412,-0.0728164363552954,
2.31512578325496));
#22638=CARTESIAN_POINT('Ctrl Pts',(0.130674397762153,-0.0856773278012026,
2.31418146184917));
#22639=CARTESIAN_POINT('Ctrl Pts',(0.11858667356339,-0.100762371833234,
2.3128775623731));
#22640=CARTESIAN_POINT('Ctrl Pts',(0.115637257034872,-0.104133904437349,
2.31257023946688));
#22641=CARTESIAN_POINT('Ctrl Pts',(0.112090133970917,-0.107851946131488,
2.3122060398644));
#22642=CARTESIAN_POINT('Ctrl Pts',(0.111630298353429,-0.108327821291003,
2.31215892421139));
#22643=CARTESIAN_POINT('Ctrl Pts',(0.110939273374976,-0.109033877960786,
2.31208823823891));
#22644=CARTESIAN_POINT('Ctrl Pts',(0.110710365381722,-0.109266298152218,
2.31206484195021));
#22645=CARTESIAN_POINT('Ctrl Pts',(0.110299305468879,-0.109681047300221,
2.3120228583086));
#22646=CARTESIAN_POINT('Ctrl Pts',(0.110117429916292,-0.109863645263576,
2.31200429271565));
#22647=CARTESIAN_POINT('Ctrl Pts',(0.109722710186307,-0.110257967952639,
2.31196402152518));
#22648=CARTESIAN_POINT('Ctrl Pts',(0.109509709591646,-0.110469525791773,
2.31194230382787));
#22649=CARTESIAN_POINT('Ctrl Pts',(0.10891347724871,-0.111058300613369,
2.3118815529489));
#22650=CARTESIAN_POINT('Ctrl Pts',(0.108528904981357,-0.111434143879265,
2.3118424158559));
#22651=CARTESIAN_POINT('Ctrl Pts',(0.106295078545265,-0.113594735232751,
2.31161539775766));
#22652=CARTESIAN_POINT('Ctrl Pts',(0.104403902020008,-0.115335297047218,
2.3114244402375));
#22653=CARTESIAN_POINT('Ctrl Pts',(0.0913914081128948,-0.126729131983352,
2.31012362675339));
#22654=CARTESIAN_POINT('Ctrl Pts',(0.0789905509696638,-0.1348081325099,
2.3089555088151));
#22655=CARTESIAN_POINT('Ctrl Pts',(0.0604174829504804,-0.143452706174698,
2.30740748590841));
#22656=CARTESIAN_POINT('Ctrl Pts',(0.0550662828774975,-0.145590766905035,
2.30698076857946));
#22657=CARTESIAN_POINT('Ctrl Pts',(0.0486947663130901,-0.147734731729573,
2.30649419254587));
#22658=CARTESIAN_POINT('Ctrl Pts',(0.0477785304627239,-0.148033588519964,
2.30642472063432));
#22659=CARTESIAN_POINT('Ctrl Pts',(0.0462900058302921,-0.148503853908897,
2.3063126441547));
#22660=CARTESIAN_POINT('Ctrl Pts',(0.0457194158866239,-0.148680510810826,
2.30626986865034));
#22661=CARTESIAN_POINT('Ctrl Pts',(0.044704535775544,-0.148988326904816,
2.30619411089933));
#22662=CARTESIAN_POINT('Ctrl Pts',(0.0442606537383057,-0.14912079537071,
2.30616108629661));
#22663=CARTESIAN_POINT('Ctrl Pts',(0.0433439256866625,-0.149389922196192,
2.30609310530312));
#22664=CARTESIAN_POINT('Ctrl Pts',(0.0428710089901583,-0.149526323254562,
2.30605815760138));
#22665=CARTESIAN_POINT('Ctrl Pts',(0.041638306356025,-0.149875536661246,
2.3059673749103));
#22666=CARTESIAN_POINT('Ctrl Pts',(0.0408775272656315,-0.150084818857559,
2.3059116546327));
#22667=CARTESIAN_POINT('Ctrl Pts',(0.0392106841493979,-0.150529735074436,
2.30579022419615));
#22668=CARTESIAN_POINT('Ctrl Pts',(0.0383040144313007,-0.150762997577024,
2.30572459108073));
#22669=CARTESIAN_POINT('Ctrl Pts',(0.0356443258621845,-0.151421723744951,
2.3055332292586));
#22670=CARTESIAN_POINT('Ctrl Pts',(0.0338859066404297,-0.151824906288308,
2.30540819652155));
#22671=CARTESIAN_POINT('Ctrl Pts',(0.027684854229208,-0.153133619775831,
2.30497195035553));
#22672=CARTESIAN_POINT('Ctrl Pts',(0.0232098347193774,-0.153875487792479,
2.304665590818));
#22673=CARTESIAN_POINT('Ctrl Pts',(0.00758520190213225,-0.155768451287645,
2.30361433606078));
#22674=CARTESIAN_POINT('Ctrl Pts',(-0.00365031097533175,-0.155910218561,
2.30289265779029));
#22675=CARTESIAN_POINT('Ctrl Pts',(-0.0156077146023947,-0.154767100120844,
2.30208476417693));
#22676=CARTESIAN_POINT('Ctrl Pts',(-0.0164118367845981,-0.154683895765872,
2.30203022697767));
#22677=CARTESIAN_POINT('Ctrl Pts',(-0.0183521753656967,-0.154467824354113,
2.30189805132988));
#22678=CARTESIAN_POINT('Ctrl Pts',(-0.0194876297847783,-0.154328685785224,
2.3018202247326));
#22679=CARTESIAN_POINT('Ctrl Pts',(-0.0235967877031521,-0.153779079562254,
2.30153650103275));
#22680=CARTESIAN_POINT('Ctrl Pts',(-0.0265597550136452,-0.15329510734718,
2.30132797565328));
#22681=CARTESIAN_POINT('Ctrl Pts',(-0.0300330182196448,-0.152624073389732,
2.3010768796363));
#22682=CARTESIAN_POINT('Ctrl Pts',(-0.0305588983299304,-0.152519650117446,
2.30103868036519));
#22683=CARTESIAN_POINT('Ctrl Pts',(-0.0314097200720829,-0.152346126776305,
2.3009765681056));
#22684=CARTESIAN_POINT('Ctrl Pts',(-0.0317350047007945,-0.152278699527575,
2.30095274798034));
#22685=CARTESIAN_POINT('Ctrl Pts',(-0.0323127866945208,-0.152157001208942,
2.30091030305215));
#22686=CARTESIAN_POINT('Ctrl Pts',(-0.0325653676357921,-0.152103142735537,
2.30089170197761));
#22687=CARTESIAN_POINT('Ctrl Pts',(-0.0331072912876139,-0.151986175236567,
2.30085169252804));
#22688=CARTESIAN_POINT('Ctrl Pts',(-0.0333965839233371,-0.151922869831011,
2.30083027353632));
#22689=CARTESIAN_POINT('Ctrl Pts',(-0.034192402860361,-0.151746339256154,
2.3007711872005));
#22690=CARTESIAN_POINT('Ctrl Pts',(-0.0346985395758841,-0.151631405789171,
2.30073342485367));
#22691=CARTESIAN_POINT('Ctrl Pts',(-0.0374304819687104,-0.150996642273901,
2.30052863766208));
#22692=CARTESIAN_POINT('Ctrl Pts',(-0.0396450526568146,-0.150430366785879,
2.30035918695675));
#22693=CARTESIAN_POINT('Ctrl Pts',(-0.0555856099153824,-0.145977882427733,
2.29911817184775));
#22694=CARTESIAN_POINT('Ctrl Pts',(-0.0687319353566795,-0.140268570800756,
2.29798722909077));
#22695=CARTESIAN_POINT('Ctrl Pts',(-0.0864509634863847,-0.129475964106872,
2.29641219325171));
#22696=CARTESIAN_POINT('Ctrl Pts',(-0.0917698688313938,-0.125762107635986,
2.29593026562642));
#22697=CARTESIAN_POINT('Ctrl Pts',(-0.0976197527097639,-0.121108106566357,
2.29538895531626));
#22698=CARTESIAN_POINT('Ctrl Pts',(-0.0983913157112131,-0.120482109348251,
2.29531730941778));
#22699=CARTESIAN_POINT('Ctrl Pts',(-0.0996189600708093,-0.11946641796668,
2.29520288954043));
#22700=CARTESIAN_POINT('Ctrl Pts',(-0.100078865983213,-0.119081412611466,
2.29515992807081));
#22701=CARTESIAN_POINT('Ctrl Pts',(-0.100891393009271,-0.118393182150484,
2.29508384869341));
#22702=CARTESIAN_POINT('Ctrl Pts',(-0.10124490026642,-0.118091019733701,
2.29505068805746));
#22703=CARTESIAN_POINT('Ctrl Pts',(-0.101607125717096,-0.117778583284636,
2.29501664536663));
#22704=CARTESIAN_POINT('Ctrl Pts',(-0.10161719976442,-0.117769891691691,
2.29501569853566));
#22705=CARTESIAN_POINT('Ctrl Pts',(-0.101633283523633,-0.117756011495156,
2.29501418678699));
#22706=CARTESIAN_POINT('Ctrl Pts',(-0.101639293870939,-0.117750823795233,
2.29501362184264));
#22707=CARTESIAN_POINT('Ctrl Pts',(-0.10165299888429,-0.117738992781383,
2.29501233359418));
#22708=CARTESIAN_POINT('Ctrl Pts',(-0.101660693111013,-0.117732349333234,
2.29501161031966));
#22709=CARTESIAN_POINT('Ctrl Pts',(-0.101675342103734,-0.117719698404918,
2.29501023322438));
#22710=CARTESIAN_POINT('Ctrl Pts',(-0.101682296928704,-0.117713691114315,
2.29500957940358));
#22711=CARTESIAN_POINT('Ctrl Pts',(-0.10169554829551,-0.11770224308024,
2.29500833360016));
#22712=CARTESIAN_POINT('Ctrl Pts',(-0.101701844857993,-0.117696802512736,
2.29500774162002));
#22713=CARTESIAN_POINT('Ctrl Pts',(-0.101713850186109,-0.117686427583007,
2.29500661288387));
#22714=CARTESIAN_POINT('Ctrl Pts',(-0.10171955930256,-0.11768149307447,
2.29500607609845));
#22715=CARTESIAN_POINT('Ctrl Pts',(-0.101730451612529,-0.117672077238649,
2.29500505194457));
#22716=CARTESIAN_POINT('Ctrl Pts',(-0.10173563486942,-0.117667595984042,
2.29500456457307));
#22717=CARTESIAN_POINT('Ctrl Pts',(-0.101745529775735,-0.117659040066871,
2.29500363414828));
#22718=CARTESIAN_POINT('Ctrl Pts',(-0.101750241475586,-0.117654965464542,
2.29500319109262));
#22719=CARTESIAN_POINT('Ctrl Pts',(-0.101759240998286,-0.117647181876978,
2.29500234481817));
#22720=CARTESIAN_POINT('Ctrl Pts',(-0.101763528863751,-0.117643472939804,
2.29500194159731));
#22721=CARTESIAN_POINT('Ctrl Pts',(-0.101771722869697,-0.117636384468466,
2.29500117103421));
#22722=CARTESIAN_POINT('Ctrl Pts',(-0.101775629043845,-0.117633004974832,
2.2950008036904));
#22723=CARTESIAN_POINT('Ctrl Pts',(-0.101783097003189,-0.117626543291154,
2.29500010137486));
#22724=CARTESIAN_POINT('Ctrl Pts',(-0.101786658817873,-0.117623461132889,
2.29499976640168));
#22725=CARTESIAN_POINT('Ctrl Pts',(-0.101793471223949,-0.117617565587205,
2.29499912571213));
#22726=CARTESIAN_POINT('Ctrl Pts',(-0.101796721838939,-0.117614752226611,
2.29499881999463));
#22727=CARTESIAN_POINT('Ctrl Pts',(-0.101802941384818,-0.117609368847974,
2.29499823504145));
#22728=CARTESIAN_POINT('Ctrl Pts',(-0.101805910334738,-0.11760679885251,
2.29499795580487));
#22729=CARTESIAN_POINT('Ctrl Pts',(-0.101813013726995,-0.117600649512374,
2.2949972877037));
#22730=CARTESIAN_POINT('Ctrl Pts',(-0.101817147709411,-0.117597070381089,
2.29499689887815));
#22731=CARTESIAN_POINT('Ctrl Pts',(-0.1018253341519,-0.117589981943983,
2.29499612887739));
#22732=CARTESIAN_POINT('Ctrl Pts',(-0.101829386571973,-0.117586472687579,
2.2949957477063));
#22733=CARTESIAN_POINT('Ctrl Pts',(-0.1018374121774,-0.117579522063298,
2.29499499280031));
#22734=CARTESIAN_POINT('Ctrl Pts',(-0.101841385801765,-0.117576080329339,
2.29499461902444));
#22735=CARTESIAN_POINT('Ctrl Pts',(-0.101849256544208,-0.117569262428486,
2.29499387865321));
#22736=CARTESIAN_POINT('Ctrl Pts',(-0.101853153668494,-0.11756588626965,
2.29499351205757));
#22737=CARTESIAN_POINT('Ctrl Pts',(-0.101860874049315,-0.117559197273126,
2.29499278579951));
#22738=CARTESIAN_POINT('Ctrl Pts',(-0.101864697312784,-0.117555884442111,
2.29499242613672));
#22739=CARTESIAN_POINT('Ctrl Pts',(-0.101872272364746,-0.117549320065628,
2.29499171352012));
#22740=CARTESIAN_POINT('Ctrl Pts',(-0.101876024158912,-0.117546068527285,
2.29499136056605));
#22741=CARTESIAN_POINT('Ctrl Pts',(-0.101883458568497,-0.117539624781915,
2.29499066115168));
#22742=CARTESIAN_POINT('Ctrl Pts',(-0.101887141188776,-0.117536432582116,
2.29499031469119));
#22743=CARTESIAN_POINT('Ctrl Pts',(-0.101894439453545,-0.117530105638289,
2.2949896280575));
#22744=CARTESIAN_POINT('Ctrl Pts',(-0.101898055103377,-0.117526970900507,
2.29498928788406));
#22745=CARTESIAN_POINT('Ctrl Pts',(-0.102309596041633,-0.11717013512522,
2.29495056785704));
#22746=CARTESIAN_POINT('Ctrl Pts',(-0.102715681769539,-0.116814308795776,
2.29491227575156));
#22747=CARTESIAN_POINT('Ctrl Pts',(-0.103850390269405,-0.115809545907973,
2.29480502946776));
#22748=CARTESIAN_POINT('Ctrl Pts',(-0.104574781649206,-0.115155849190516,
2.29473627408903));
#22749=CARTESIAN_POINT('Ctrl Pts',(-0.10618677031788,-0.113673421464368,
2.29458257605452));
#22750=CARTESIAN_POINT('Ctrl Pts',(-0.10707091726593,-0.112841019833296,
2.29449779078458));
#22751=CARTESIAN_POINT('Ctrl Pts',(-0.109810328884732,-0.110200744145112,
2.29423343432206));
#22752=CARTESIAN_POINT('Ctrl Pts',(-0.111630297294349,-0.108356773289963,
2.29405537427602));
#22753=CARTESIAN_POINT('Ctrl Pts',(-0.11752884350704,-0.102073995804524,
2.29346839907961));
#22754=CARTESIAN_POINT('Ctrl Pts',(-0.12139557014892,-0.097443597040058,
2.29306733138319));
#22755=CARTESIAN_POINT('Ctrl Pts',(-0.130028326557518,-0.0857918089324549,
2.2921098405174));
#22756=CARTESIAN_POINT('Ctrl Pts',(-0.134507522177228,-0.0785831410819303,
2.29155834678455));
#22757=CARTESIAN_POINT('Ctrl Pts',(-0.138920994462656,-0.0699869794310976,
2.29090750736873));
#22758=CARTESIAN_POINT('Ctrl Pts',(-0.139452593225423,-0.0689216519102421,
2.29082694740148));
#22759=CARTESIAN_POINT('Ctrl Pts',(-0.141512862266604,-0.0646714195041184,
2.29050552859275));
#22760=CARTESIAN_POINT('Ctrl Pts',(-0.142944931834371,-0.0614412253729993,
2.29026121758013));
#22761=CARTESIAN_POINT('Ctrl Pts',(-0.144475991736227,-0.0576437910777903,
2.28997078127456));
#22762=CARTESIAN_POINT('Ctrl Pts',(-0.144683471855134,-0.0571210275133582,
2.2899307295005));
#22763=CARTESIAN_POINT('Ctrl Pts',(-0.145010532902854,-0.056283754835779,
2.28986645250326));
#22764=CARTESIAN_POINT('Ctrl Pts',(-0.145131938897866,-0.0559699563797075,
2.28984233353715));
#22765=CARTESIAN_POINT('Ctrl Pts',(-0.145345158906176,-0.0554134875444801,
2.28979950738275));
#22766=CARTESIAN_POINT('Ctrl Pts',(-0.145437385110067,-0.0551709781533011,
2.28978082509871));
#22767=CARTESIAN_POINT('Ctrl Pts',(-0.145631510470751,-0.0546566548701083,
2.28974116201168));
#22768=CARTESIAN_POINT('Ctrl Pts',(-0.145733254029886,-0.0543847904258592,
2.28972017279199));
#22769=CARTESIAN_POINT('Ctrl Pts',(-0.14600559322731,-0.053650832995713,
2.28966344660182));
#22770=CARTESIAN_POINT('Ctrl Pts',(-0.146174753863473,-0.053188217210018,
2.2896276266137));
#22771=CARTESIAN_POINT('Ctrl Pts',(-0.147000317391728,-0.0508968031751458,
2.28944990874089));
#22772=CARTESIAN_POINT('Ctrl Pts',(-0.147624573347133,-0.0490567251148018,
2.28930626890348));
#22773=CARTESIAN_POINT('Ctrl Pts',(-0.14932388052995,-0.0437213069692471,
2.2888880528355));
#22774=CARTESIAN_POINT('Ctrl Pts',(-0.150310308005517,-0.0401992679072003,
2.28860989262441));
#22775=CARTESIAN_POINT('Ctrl Pts',(-0.154071104219069,-0.0246852926814152,
2.28738409848849));
#22776=CARTESIAN_POINT('Ctrl Pts',(-0.155541082746387,-0.0124211275142716,
2.28641821317254));
#22777=CARTESIAN_POINT('Ctrl Pts',(-0.15554995955069,-0.000112177443420774,
2.28549129411633));
#22778=CARTESIAN_POINT('Origin',(0.,0.,0.));
#22779=CARTESIAN_POINT('',(-0.195399959231026,0.000126224060331325,0.022586969212423));
#22780=CARTESIAN_POINT('',(0.0861527862262976,0.175382032789696,3.89164997704322E-6));
#22781=CARTESIAN_POINT('Ctrl Pts',(-0.195399959231026,0.000126224060331325,
0.022586969212423));
#22782=CARTESIAN_POINT('Ctrl Pts',(-0.195395691015159,0.00673359514406753,
0.0222084605749147));
#22783=CARTESIAN_POINT('Ctrl Pts',(-0.195056309456599,0.0133308173981378,
0.0218299519374064));
#22784=CARTESIAN_POINT('Ctrl Pts',(-0.194384733506787,0.0198930987906703,
0.0214514432998981));
#22785=CARTESIAN_POINT('Ctrl Pts',(-0.193146662383657,0.031990868367168,
0.0207536508698904));
#22786=CARTESIAN_POINT('Ctrl Pts',(-0.190770597340965,0.0440147328451167,
0.0200558584398827));
#22787=CARTESIAN_POINT('Ctrl Pts',(-0.187282282163595,0.0557360456759846,
0.019358066009875));
#22788=CARTESIAN_POINT('Ctrl Pts',(-0.183801324713759,0.0674326353319801,
0.0186617453982992));
#22789=CARTESIAN_POINT('Ctrl Pts',(-0.179212949381552,0.07882709146759,
0.0179654247867235));
#22790=CARTESIAN_POINT('Ctrl Pts',(-0.173593710691015,0.0897016365989175,
0.0172691041751478));
#22791=CARTESIAN_POINT('Ctrl Pts',(-0.167975543236407,0.100574108637412,
0.0165729163081836));
#22792=CARTESIAN_POINT('Ctrl Pts',(-0.161327261645753,0.1109260719967,0.0158767284412195));
#22793=CARTESIAN_POINT('Ctrl Pts',(-0.153772634205927,0.120561755832312,
0.0151805405742553));
#22794=CARTESIAN_POINT('Ctrl Pts',(-0.146218660721959,0.130196605568303,
0.0144844129718293));
#22795=CARTESIAN_POINT('Ctrl Pts',(-0.137759054868081,0.139114627980258,
0.0137882853694032));
#22796=CARTESIAN_POINT('Ctrl Pts',(-0.128557927835573,0.147153046827525,
0.0130921577669772));
#22797=CARTESIAN_POINT('Ctrl Pts',(-0.119336310503073,0.155209366700727,
0.0123944799345243));
#22798=CARTESIAN_POINT('Ctrl Pts',(-0.109370572659015,0.162381645799003,
0.0116968021020714));
#22799=CARTESIAN_POINT('Ctrl Pts',(-0.0988569646754872,0.168548095614129,
0.0109991242696186));
#22800=CARTESIAN_POINT('Ctrl Pts',(-0.0955296651869108,0.17049962598775,
0.0107783263191197));
#22801=CARTESIAN_POINT('Ctrl Pts',(-0.092147681027628,0.17235076076533,
0.0105575283686208));
#22802=CARTESIAN_POINT('Ctrl Pts',(-0.088717691762081,0.174098624832043,
0.0103367304181219));
#22803=CARTESIAN_POINT('Ctrl Pts',(-0.0779973467121408,0.179561529944827,
0.00964663198561551));
#22804=CARTESIAN_POINT('Ctrl Pts',(-0.0667297219952147,0.18405116145512,
0.00895653355310913));
#22805=CARTESIAN_POINT('Ctrl Pts',(-0.0551164653379072,0.187465557499652,
0.00826643512060275));
#22806=CARTESIAN_POINT('Ctrl Pts',(-0.0435178297514944,0.190875654825219,
0.00757720552087978));
#22807=CARTESIAN_POINT('Ctrl Pts',(-0.0315752486213366,0.193212862185595,
0.00688797592115681));
#22808=CARTESIAN_POINT('Ctrl Pts',(-0.0195095720492338,0.19442360092966,
0.00619874632143384));
#22809=CARTESIAN_POINT('Ctrl Pts',(-0.00745527551376608,0.195633197736,
0.00551016678538927));
#22810=CARTESIAN_POINT('Ctrl Pts',(0.00472099927633243,0.195718325467519,
0.0048215872493447));
#22811=CARTESIAN_POINT('Ctrl Pts',(0.0167919026286014,0.194677148135346,
0.00413300771330014));
#22812=CARTESIAN_POINT('Ctrl Pts',(0.0288902804919299,0.193633600985663,
0.00344286090548424));
#22813=CARTESIAN_POINT('Ctrl Pts',(0.0408819121079928,0.191458712987708,
0.00275271409766835));
#22814=CARTESIAN_POINT('Ctrl Pts',(0.0525441651269303,0.188202738319914,
0.00206256728985245));
#22815=CARTESIAN_POINT('Ctrl Pts',(0.0641401501764159,0.184965264951094,
0.00137634207656065));
#22816=CARTESIAN_POINT('Ctrl Pts',(0.0754096998225287,0.180659351176491,
0.000690116863268847));
#22817=CARTESIAN_POINT('Ctrl Pts',(0.0861527862262976,0.175382032789696,
3.89164997704322E-6));
#22818=CARTESIAN_POINT('',(-0.0861525859670424,0.175382131162759,0.));
#22819=CARTESIAN_POINT('Origin',(0.,0.,0.));
#22820=CARTESIAN_POINT('',(-0.195399889995494,0.000207339694122921,0.0124130307921719));
#22821=CARTESIAN_POINT('Ctrl Pts',(-0.0861525859670426,0.175382131162759,
-6.38378239159465E-16));
#22822=CARTESIAN_POINT('Ctrl Pts',(-0.0973787392951184,0.169867532079808,
0.000713121939821653));
#22823=CARTESIAN_POINT('Ctrl Pts',(-0.108088311316424,0.163263883278222,
0.00142624387964394));
#22824=CARTESIAN_POINT('Ctrl Pts',(-0.118072608656115,0.155692064939546,
0.00213936581946623));
#22825=CARTESIAN_POINT('Ctrl Pts',(-0.128544465897827,0.14775049449096,
0.00288731140799201));
#22826=CARTESIAN_POINT('Ctrl Pts',(-0.138217415582637,0.138744057021195,
0.00363525699651779));
#22827=CARTESIAN_POINT('Ctrl Pts',(-0.146886675695703,0.128862191906957,
0.00438320258504356));
#22828=CARTESIAN_POINT('Ctrl Pts',(-0.155156273697141,0.119435891284598,
0.00509666708644155));
#22829=CARTESIAN_POINT('Ctrl Pts',(-0.162512351578732,0.109213971190783,
0.00581013158783954));
#22830=CARTESIAN_POINT('Ctrl Pts',(-0.168817837730545,0.098395618113732,
0.00652359608923752));
#22831=CARTESIAN_POINT('Ctrl Pts',(-0.175127968716422,0.0875692958724215,
0.00723758615268405));
#22832=CARTESIAN_POINT('Ctrl Pts',(-0.180385602605581,0.0761463975398017,
0.00795157621613059));
#22833=CARTESIAN_POINT('Ctrl Pts',(-0.184499920041503,0.0643501321263515,
0.00866556627957712));
#22834=CARTESIAN_POINT('Ctrl Pts',(-0.188625481498626,0.0525216286903234,
0.00938150760700247));
#22835=CARTESIAN_POINT('Ctrl Pts',(-0.19160129016889,0.040318514344953,
0.0100974489344278));
#22836=CARTESIAN_POINT('Ctrl Pts',(-0.19338664446451,0.0279779510107032,
0.0108133902618532));
#22837=CARTESIAN_POINT('Ctrl Pts',(-0.193637115470647,0.0262466681374884,
0.0109138311351606));
#22838=CARTESIAN_POINT('Ctrl Pts',(-0.19386423961171,0.0245126879456285,
0.0110142720084681));
#22839=CARTESIAN_POINT('Ctrl Pts',(-0.194067986277009,0.0227766701338622,
0.0111147128817756));
#22840=CARTESIAN_POINT('Ctrl Pts',(-0.194945875709514,0.0152966375681304,
0.0115474855170436));
#22841=CARTESIAN_POINT('Ctrl Pts',(-0.195391874966475,0.00776081463203696,
0.0119802581523117));
#22842=CARTESIAN_POINT('Ctrl Pts',(-0.195399889995409,0.000207339774271115,
0.0124130307875798));
#22843=CARTESIAN_POINT('',(-0.195388139417384,8.91918474211534E-5,0.0824130265070756));
#22844=CARTESIAN_POINT('Ctrl Pts',(-0.195399889995494,0.000207339694122791,
0.0124130307921719));
#22845=CARTESIAN_POINT('Ctrl Pts',(-0.19541248349625,-0.0116609553406007,
0.0130930189320593));
#22846=CARTESIAN_POINT('Ctrl Pts',(-0.194339510846434,-0.0235796520165797,
0.0137730070719468));
#22847=CARTESIAN_POINT('Ctrl Pts',(-0.192179861920935,-0.0353279021744901,
0.0144529952118342));
#22848=CARTESIAN_POINT('Ctrl Pts',(-0.190022526011279,-0.0470635697832568,
0.0151322550743976));
#22849=CARTESIAN_POINT('Ctrl Pts',(-0.186780890382315,-0.0586282396042047,
0.015811514936961));
#22850=CARTESIAN_POINT('Ctrl Pts',(-0.182505705615822,-0.0698056402998427,
0.0164907747995244));
#22851=CARTESIAN_POINT('Ctrl Pts',(-0.178233893778169,-0.0809742225281551,
0.0171694987565525));
#22852=CARTESIAN_POINT('Ctrl Pts',(-0.172930468207996,-0.0917552796565982,
0.0178482227135805));
#22853=CARTESIAN_POINT('Ctrl Pts',(-0.166695188924135,-0.10195035061022,
0.0185269466706086));
#22854=CARTESIAN_POINT('Ctrl Pts',(-0.160445205209005,-0.112169464227099,
0.0192072712375409));
#22855=CARTESIAN_POINT('Ctrl Pts',(-0.153259486033948,-0.121799059378327,
0.0198875958044733));
#22856=CARTESIAN_POINT('Ctrl Pts',(-0.145281699930208,-0.13066900039944,
0.0205679203714056));
#22857=CARTESIAN_POINT('Ctrl Pts',(-0.138787184776203,-0.137889796448328,
0.021121755502121));
#22858=CARTESIAN_POINT('Ctrl Pts',(-0.131768746190028,-0.144607600314278,
0.0216755906328364));
#22859=CARTESIAN_POINT('Ctrl Pts',(-0.124320713498993,-0.150749859685179,
0.0222294257635518));
#22860=CARTESIAN_POINT('Ctrl Pts',(-0.114940365634237,-0.158485664825235,
0.0229269477000608));
#22861=CARTESIAN_POINT('Ctrl Pts',(-0.104802633402424,-0.165369479385504,
0.0236244696365698));
#22862=CARTESIAN_POINT('Ctrl Pts',(-0.0940864764685079,-0.171256809925156,
0.0243219915730788));
#22863=CARTESIAN_POINT('Ctrl Pts',(-0.0833927779248148,-0.177131802089451,
0.0250180516777076));
#22864=CARTESIAN_POINT('Ctrl Pts',(-0.0721237827245387,-0.182013975205295,
0.0257141117823364));
#22865=CARTESIAN_POINT('Ctrl Pts',(-0.0604869483569958,-0.185802284911833,
0.0264101718869652));
#22866=CARTESIAN_POINT('Ctrl Pts',(-0.0488520442556239,-0.189589966230458,
0.0271061165322491));
#22867=CARTESIAN_POINT('Ctrl Pts',(-0.0368502364226137,-0.192283831461089,
0.027802061177533));
#22868=CARTESIAN_POINT('Ctrl Pts',(-0.0247070928623388,-0.193831678428196,
0.0284980058228169));
#22869=CARTESIAN_POINT('Ctrl Pts',(-0.0125648311255019,-0.195379412992142,
0.0291938999292682));
#22870=CARTESIAN_POINT('Ctrl Pts',(-0.000282122853219399,-0.195781209666355,
0.0298897940357194));
#22871=CARTESIAN_POINT('Ctrl Pts',(0.0119099790838408,-0.195036695004357,
0.0305856881421707));
#22872=CARTESIAN_POINT('Ctrl Pts',(0.0241295498036195,-0.194290502952226,
0.0312831500967342));
#22873=CARTESIAN_POINT('Ctrl Pts',(0.036257240023152,-0.192392959679809,
0.0319806120512976));
#22874=CARTESIAN_POINT('Ctrl Pts',(0.0480679653519524,-0.189395434757344,
0.0326780740058611));
#22875=CARTESIAN_POINT('Ctrl Pts',(0.0518276478486094,-0.18844123917066,
0.03290009555235));
#22876=CARTESIAN_POINT('Ctrl Pts',(0.0555553214346533,-0.187375961169439,
0.0331221170988389));
#22877=CARTESIAN_POINT('Ctrl Pts',(0.0592440995815707,-0.186202300374536,
0.0333441386453279));
#22878=CARTESIAN_POINT('Ctrl Pts',(0.0708356461158782,-0.182514210937394,
0.0340418149449709));
#22879=CARTESIAN_POINT('Ctrl Pts',(0.0821208716200282,-0.177727063673689,
0.034739491244614));
#22880=CARTESIAN_POINT('Ctrl Pts',(0.0928813521728905,-0.171913392202398,
0.035437167544257));
#22881=CARTESIAN_POINT('Ctrl Pts',(0.10361992062053,-0.166111559401358,
0.0361334231307253));
#22882=CARTESIAN_POINT('Ctrl Pts',(0.113835071487107,-0.159287699999734,
0.0368296787171935));
#22883=CARTESIAN_POINT('Ctrl Pts',(0.123329561574715,-0.151561800074387,
0.0375259343036618));
#22884=CARTESIAN_POINT('Ctrl Pts',(0.132823263600492,-0.14383654141432,
0.0382221320995117));
#22885=CARTESIAN_POINT('Ctrl Pts',(0.14159572037423,-0.135209906558148,
0.0389183298953617));
#22886=CARTESIAN_POINT('Ctrl Pts',(0.149480998995562,-0.125843517668924,
0.0396145276912116));
#22887=CARTESIAN_POINT('Ctrl Pts',(0.157366087284026,-0.116477354863234,
0.0403107086824147));
#22888=CARTESIAN_POINT('Ctrl Pts',(0.164363499650161,-0.106372158645069,
0.0410068896736177));
#22889=CARTESIAN_POINT('Ctrl Pts',(0.170347959658608,-0.0957221637874385,
0.0417030706648208));
#22890=CARTESIAN_POINT('Ctrl Pts',(0.176346285302151,-0.0850474935301456,
0.0424008646656473));
#22891=CARTESIAN_POINT('Ctrl Pts',(0.181326603057855,-0.0738262963564154,
0.0430986586664738));
#22892=CARTESIAN_POINT('Ctrl Pts',(0.185210396967689,-0.0622757485307955,
0.0437964526673002));
#22893=CARTESIAN_POINT('Ctrl Pts',(0.186439327308421,-0.0586208638987797,
0.0440172522872349));
#22894=CARTESIAN_POINT('Ctrl Pts',(0.187558844857637,-0.0549331151734461,
0.0442380519071695));
#22895=CARTESIAN_POINT('Ctrl Pts',(0.188567520760656,-0.0512196262596647,
0.0444588515271041));
#22896=CARTESIAN_POINT('Ctrl Pts',(0.191744677001402,-0.039522772550707,
0.0451543324921298));
#22897=CARTESIAN_POINT('Ctrl Pts',(0.193840871021327,-0.0274866554491859,
0.0458498134571554));
#22898=CARTESIAN_POINT('Ctrl Pts',(0.194797524331189,-0.0153324660260424,
0.0465452944221811));
#22899=CARTESIAN_POINT('Ctrl Pts',(0.195752137868602,-0.0032041917180958,
0.0472392924854106));
#22900=CARTESIAN_POINT('Ctrl Pts',(0.195571888140668,0.00904079464269347,
0.0479332905486402));
#22901=CARTESIAN_POINT('Ctrl Pts',(0.194249488119407,0.0211730103043578,
0.0486272886118697));
#22902=CARTESIAN_POINT('Ctrl Pts',(0.192927305321299,0.0333032330757399,
0.0493211726759721));
#22903=CARTESIAN_POINT('Ctrl Pts',(0.190463392484403,0.045319844906771,
0.0500150567400744));
#22904=CARTESIAN_POINT('Ctrl Pts',(0.186902439992509,0.056996823813669,
0.0507089408041768));
#22905=CARTESIAN_POINT('Ctrl Pts',(0.183341753083698,0.0686729318277191,
0.0514027731169937));
#22906=CARTESIAN_POINT('Ctrl Pts',(0.178684470441836,0.0800086245418753,
0.0520966054298106));
#22907=CARTESIAN_POINT('Ctrl Pts',(0.173024791587216,0.0907941710474873,
0.0527904377426275));
#22908=CARTESIAN_POINT('Ctrl Pts',(0.16735202485232,0.101604658887229,0.0534858745270894));
#22909=CARTESIAN_POINT('Ctrl Pts',(0.160672700054938,0.11186171361103,0.0541813113115513));
#22910=CARTESIAN_POINT('Ctrl Pts',(0.153125715666315,0.1213823512776,0.0548767480960132));
#22911=CARTESIAN_POINT('Ctrl Pts',(0.150605063920322,0.124562192485883,
0.0551090202003022));
#22912=CARTESIAN_POINT('Ctrl Pts',(0.14798795211152,0.127660164716599,0.0553412923045913));
#22913=CARTESIAN_POINT('Ctrl Pts',(0.145280482942679,0.130670353469874,
0.0555735644088803));
#22914=CARTESIAN_POINT('Ctrl Pts',(0.13715996025331,0.139698824172913,0.0562702190244504));
#22915=CARTESIAN_POINT('Ctrl Pts',(0.128165982374556,0.147999250676689,
0.0569668736400205));
#22916=CARTESIAN_POINT('Ctrl Pts',(0.118453589953988,0.155402403543229,
0.0576635282555905));
#22917=CARTESIAN_POINT('Ctrl Pts',(0.108761558649387,0.162790036397035,
0.0583587224003721));
#22918=CARTESIAN_POINT('Ctrl Pts',(0.0983547461448614,0.169283544951386,
0.0590539165451536));
#22919=CARTESIAN_POINT('Ctrl Pts',(0.0874228563386221,0.174752408251207,
0.0597491106899351));
#22920=CARTESIAN_POINT('Ctrl Pts',(0.0764925301188179,0.180220489340394,
0.0604442054012103));
#22921=CARTESIAN_POINT('Ctrl Pts',(0.0650380365633925,0.18466378412364,
0.0611393001124855));
#22922=CARTESIAN_POINT('Ctrl Pts',(0.0532742562263546,0.187997376640018,
0.0618343948237606));
#22923=CARTESIAN_POINT('Ctrl Pts',(0.0415111862009438,0.191330767869951,
0.0625294475643562));
#22924=CARTESIAN_POINT('Ctrl Pts',(0.0294397157166617,0.193554376859989,
0.0632245003049518));
#22925=CARTESIAN_POINT('Ctrl Pts',(0.017287816857642,0.194633736511162,
0.0639195530455473));
#22926=CARTESIAN_POINT('Ctrl Pts',(0.00510800481860889,0.195715575475289,
0.064616202337636));
#22927=CARTESIAN_POINT('Ctrl Pts',(-0.00715172753794594,0.195647904879166,
0.0653128516297247));
#22928=CARTESIAN_POINT('Ctrl Pts',(-0.0192616770895324,0.194448316515465,
0.0660095009218133));
#22929=CARTESIAN_POINT('Ctrl Pts',(-0.0231947644535041,0.194058712428748,
0.0662357597114277));
#22930=CARTESIAN_POINT('Ctrl Pts',(-0.0271121067131916,0.193550118186344,
0.0664620185010421));
#22931=CARTESIAN_POINT('Ctrl Pts',(-0.0310060669591839,0.192924295545487,
0.0666882772906565));
#22932=CARTESIAN_POINT('Ctrl Pts',(-0.0429945409988469,0.190997553100938,
0.0673848682813658));
#22933=CARTESIAN_POINT('Ctrl Pts',(-0.0548449574354469,0.187942291874567,
0.068081459272075));
#22934=CARTESIAN_POINT('Ctrl Pts',(-0.0663310882544109,0.183797025903537,
0.0687780502627842));
#22935=CARTESIAN_POINT('Ctrl Pts',(-0.0777932036131686,0.17966042694767,
0.06947318480541));
#22936=CARTESIAN_POINT('Ctrl Pts',(-0.0888917048713986,0.174438571179859,
0.0701683193480358));
#22937=CARTESIAN_POINT('Ctrl Pts',(-0.0994140975485735,0.168220085627736,
0.0708634538906616));
#22938=CARTESIAN_POINT('Ctrl Pts',(-0.109935089131981,0.162002428088937,
0.0715584958736667));
#22939=CARTESIAN_POINT('Ctrl Pts',(-0.119879348724295,0.154788809414352,
0.0722535378566717));
#22940=CARTESIAN_POINT('Ctrl Pts',(-0.129059053527509,0.146713737266091,
0.0729485798396768));
#22941=CARTESIAN_POINT('Ctrl Pts',(-0.138238256019874,0.138639106983493,
0.0736435837901813));
#22942=CARTESIAN_POINT('Ctrl Pts',(-0.146652347325546,0.12970371515905,
0.0743385877406857));
#22943=CARTESIAN_POINT('Ctrl Pts',(-0.154148802646238,0.120080417399054,
0.0750335916911901));
#22944=CARTESIAN_POINT('Ctrl Pts',(-0.161662552042581,0.110434919007913,
0.0757301989929297));
#22945=CARTESIAN_POINT('Ctrl Pts',(-0.168253952897313,0.10009907648672,
0.0764268062946693));
#22946=CARTESIAN_POINT('Ctrl Pts',(-0.173813289290223,0.0892754191595494,
0.0771234135964089));
#22947=CARTESIAN_POINT('Ctrl Pts',(-0.175621096348529,0.0857557393399034,
0.0773499391217501));
#22948=CARTESIAN_POINT('Ctrl Pts',(-0.177320141305075,0.0821846514608763,
0.0775764646470914));
#22949=CARTESIAN_POINT('Ctrl Pts',(-0.178907755968516,0.0785695542453295,
0.0778029901724326));
#22950=CARTESIAN_POINT('Ctrl Pts',(-0.184292698038043,0.0663077066259412,
0.0785713295304148));
#22951=CARTESIAN_POINT('Ctrl Pts',(-0.18842496616365,0.0534633499586128,
0.0793396688883969));
#22952=CARTESIAN_POINT('Ctrl Pts',(-0.191200323201082,0.0402938755619492,
0.0801080082463791));
#22953=CARTESIAN_POINT('Ctrl Pts',(-0.193975680238514,0.0271244011652855,
0.0808763476043612));
#22954=CARTESIAN_POINT('Ctrl Pts',(-0.195393798080322,0.0136303363268635,
0.0816446869623434));
#22955=CARTESIAN_POINT('Ctrl Pts',(-0.195399979639876,8.92005390054972E-5,
0.0824130263203255));
#22956=CARTESIAN_POINT('',(-0.195296072527608,-0.000171556393799694,0.15241303078758));
#22957=CARTESIAN_POINT('Ctrl Pts',(-0.195116749400228,8.89926274127593E-5,
0.0824130307875797));
#22958=CARTESIAN_POINT('Ctrl Pts',(-0.194962860530686,-0.0380682611678014,
0.0845812548764561));
#22959=CARTESIAN_POINT('Ctrl Pts',(-0.165715764002923,-0.1416455872943,
0.090454383259258));
#22960=CARTESIAN_POINT('Ctrl Pts',(0.00247549259342833,-0.230944160436683,
0.100032415935985));
#22961=CARTESIAN_POINT('Ctrl Pts',(0.195382766643704,-0.123157545007233,
0.111147128817761));
#22962=CARTESIAN_POINT('Ctrl Pts',(0.209427835089859,0.0973768392715823,
0.122261841699537));
#22963=CARTESIAN_POINT('Ctrl Pts',(0.0317514812939098,0.228765894785075,
0.133376554581314));
#22964=CARTESIAN_POINT('Ctrl Pts',(-0.155194310144234,0.158204250355088,
0.143426950943994));
#22965=CARTESIAN_POINT('Ctrl Pts',(-0.194905030259773,0.0461907277712621,
0.14977244301275));
#22966=CARTESIAN_POINT('Ctrl Pts',(-0.195296072527608,-0.000171556393799694,
0.15241303078758));
#22967=CARTESIAN_POINT('',(-0.195431294938471,1.28888134066882E-5,0.22241303078758));
#22968=CARTESIAN_POINT('Ctrl Pts',(-0.195296072527608,-0.000171556393799694,
0.15241303078758));
#22969=CARTESIAN_POINT('Ctrl Pts',(-0.195453686203354,-0.0188583599040719,
0.153477347306675));
#22970=CARTESIAN_POINT('Ctrl Pts',(-0.184414778781475,-0.102411837350248,
0.158246568119694));
#22971=CARTESIAN_POINT('Ctrl Pts',(-0.0652778999832005,-0.221542065857058,
0.166720693226644));
#22972=CARTESIAN_POINT('Ctrl Pts',(0.150741393243207,-0.174983271977123,
0.177835406108417));
#22973=CARTESIAN_POINT('Ctrl Pts',(0.228764398331316,0.0317641428286245,
0.188950118990195));
#22974=CARTESIAN_POINT('Ctrl Pts',(0.0973648674331604,0.209433016993645,
0.20006483187197));
#22975=CARTESIAN_POINT('Ctrl Pts',(-0.123167391259255,0.195376311478096,
0.211179544753746));
#22976=CARTESIAN_POINT('Ctrl Pts',(-0.195403696181917,0.0660797489631491,
0.218628944392284));
#22977=CARTESIAN_POINT('Ctrl Pts',(-0.195720085887096,0.000704139451294379,
0.222373439736894));
#22978=CARTESIAN_POINT('Ctrl Pts',(-0.195719426634615,1.29078158682454E-5,
0.22241303078758));
#22979=CARTESIAN_POINT('',(-0.195399931451662,0.000163672496008518,0.292413028611086));
#22980=CARTESIAN_POINT('Ctrl Pts',(-0.195399999575055,1.28867494583334E-5,
0.22241303078758));
#22981=CARTESIAN_POINT('Ctrl Pts',(-0.195400798685208,-0.0121039099641912,
0.223108168176893));
#22982=CARTESIAN_POINT('Ctrl Pts',(-0.194270226249095,-0.0242644285419508,
0.223803305566206));
#22983=CARTESIAN_POINT('Ctrl Pts',(-0.192009952717491,-0.0362400063110751,
0.224498442955518));
#22984=CARTESIAN_POINT('Ctrl Pts',(-0.189754413542218,-0.0481905001018107,
0.225192124313933));
#22985=CARTESIAN_POINT('Ctrl Pts',(-0.186373957051199,-0.0599559525316625,
0.225885805672348));
#22986=CARTESIAN_POINT('Ctrl Pts',(-0.181921919938222,-0.0713132178911548,
0.226579487030763));
#22987=CARTESIAN_POINT('Ctrl Pts',(-0.177470480318604,-0.0826689590291572,
0.227273075292468));
#22988=CARTESIAN_POINT('Ctrl Pts',(-0.171948023705749,-0.0936157877531208,
0.227966663554174));
#22989=CARTESIAN_POINT('Ctrl Pts',(-0.16545710676997,-0.103947610936042,
0.228660251815879));
#22990=CARTESIAN_POINT('Ctrl Pts',(-0.158966419617711,-0.114279068364367,
0.229353815524019));
#22991=CARTESIAN_POINT('Ctrl Pts',(-0.151507832196829,-0.123994834102582,
0.230047379232159));
#22992=CARTESIAN_POINT('Ctrl Pts',(-0.143227346908922,-0.13291759513861,
0.230740942940299));
#22993=CARTESIAN_POINT('Ctrl Pts',(-0.134927937041833,-0.14186074863859,
0.231436091748933));
#22994=CARTESIAN_POINT('Ctrl Pts',(-0.1258035275967,-0.150006682752804,
0.232131240557566));
#22995=CARTESIAN_POINT('Ctrl Pts',(-0.116036115709074,-0.157215711209632,
0.232826389366199));
#22996=CARTESIAN_POINT('Ctrl Pts',(-0.113307534437414,-0.159229593726359,
0.233020583083232));
#22997=CARTESIAN_POINT('Ctrl Pts',(-0.110528948520751,-0.161170620676228,
0.233214776800265));
#22998=CARTESIAN_POINT('Ctrl Pts',(-0.107704695813929,-0.163036371707754,
0.233408970517299));
#22999=CARTESIAN_POINT('Ctrl Pts',(-0.0975759729852575,-0.169727584225665,
0.234105414688228));
#23000=CARTESIAN_POINT('Ctrl Pts',(-0.0867854693978241,-0.175494992900072,
0.234801858859158));
#23001=CARTESIAN_POINT('Ctrl Pts',(-0.0755256889197688,-0.180213846064042,
0.235498303030088));
#23002=CARTESIAN_POINT('Ctrl Pts',(-0.0642895405604371,-0.184922795260663,
0.236193285498335));
#23003=CARTESIAN_POINT('Ctrl Pts',(-0.0525868409204017,-0.188587153133365,
0.236888267966582));
#23004=CARTESIAN_POINT('Ctrl Pts',(-0.0406339125343382,-0.191128347327527,
0.237583250434829));
#23005=CARTESIAN_POINT('Ctrl Pts',(-0.028682668364382,-0.193669183457116,
0.238278134977227));
#23006=CARTESIAN_POINT('Ctrl Pts',(-0.0164821110971703,-0.195086943165573,
0.238973019519625));
#23007=CARTESIAN_POINT('Ctrl Pts',(-0.00426145998030663,-0.195353525585888,
0.239667904062022));
#23008=CARTESIAN_POINT('Ctrl Pts',(0.00795846468967088,-0.195620092159423,
0.240362747297561));
#23009=CARTESIAN_POINT('Ctrl Pts',(0.0201976047040516,-0.194735624932464,
0.241057590533099));
#23010=CARTESIAN_POINT('Ctrl Pts',(0.0322267690432934,-0.192724143160711,
0.241752433768638));
#23011=CARTESIAN_POINT('Ctrl Pts',(0.0442836575924967,-0.190708025427439,
0.242448878443745));
#23012=CARTESIAN_POINT('Ctrl Pts',(0.056128751836065,-0.187559915954382,
0.243145323118853));
#23013=CARTESIAN_POINT('Ctrl Pts',(0.0675442942408393,-0.183354651742209,
0.24384176779396));
#23014=CARTESIAN_POINT('Ctrl Pts',(0.0712700922282979,-0.181982140092488,
0.244069072995665));
#23015=CARTESIAN_POINT('Ctrl Pts',(0.0749502895998998,-0.180497401018055,
0.24429637819737));
#23016=CARTESIAN_POINT('Ctrl Pts',(0.0785778410801077,-0.178904116473572,
0.244523683399075));
#23017=CARTESIAN_POINT('Ctrl Pts',(0.0896923560591145,-0.174022425605202,
0.245220127566151));
#23018=CARTESIAN_POINT('Ctrl Pts',(0.100389556815391,-0.168083750291963,
0.245916571733227));
#23019=CARTESIAN_POINT('Ctrl Pts',(0.110460236869427,-0.161182182857629,
0.246613015900303));
#23020=CARTESIAN_POINT('Ctrl Pts',(0.12050978049426,-0.154295100491898,
0.24730799836442));
#23021=CARTESIAN_POINT('Ctrl Pts',(0.129934656102679,-0.146449565744652,
0.248002980828537));
#23022=CARTESIAN_POINT('Ctrl Pts',(0.138551540872232,-0.137784725285245,
0.248697963292654));
#23023=CARTESIAN_POINT('Ctrl Pts',(0.147167211483506,-0.129121105741289,
0.249392847830579));
#23024=CARTESIAN_POINT('Ctrl Pts',(0.154974468037342,-0.119638997132723,
0.250087732368505));
#23025=CARTESIAN_POINT('Ctrl Pts',(0.161825400358542,-0.109515751373023,
0.25078261690643));
#23026=CARTESIAN_POINT('Ctrl Pts',(0.168675925429507,-0.099393107384586,
0.251477460137292));
#23027=CARTESIAN_POINT('Ctrl Pts',(0.174569770435743,-0.0886301421763397,
0.252172303368155));
#23028=CARTESIAN_POINT('Ctrl Pts',(0.179402831902806,-0.0774324473670666,
0.252867146599017));
#23029=CARTESIAN_POINT('Ctrl Pts',(0.184247032364217,-0.0662089446801096,
0.253563591269231));
#23030=CARTESIAN_POINT('Ctrl Pts',(0.188025281244286,-0.0545495414013264,
0.254260035939445));
#23031=CARTESIAN_POINT('Ctrl Pts',(0.190682372292722,-0.0426777798956278,
0.254956480609659));
#23032=CARTESIAN_POINT('Ctrl Pts',(0.191549592189821,-0.0388030809847963,
0.25518378583339));
#23033=CARTESIAN_POINT('Ctrl Pts',(0.192297790378953,-0.0349058376759882,
0.255411091057121));
#23034=CARTESIAN_POINT('Ctrl Pts',(0.192926239968484,-0.0309939660518479,
0.255638396280852));
#23035=CARTESIAN_POINT('Ctrl Pts',(0.194851756905226,-0.0190083188461995,
0.256334840459343));
#23036=CARTESIAN_POINT('Ctrl Pts',(0.195662895185079,-0.00680012371250248,
0.257031284637835));
#23037=CARTESIAN_POINT('Ctrl Pts',(0.195325263932807,0.00540381990626342,
0.257727728816327));
#23038=CARTESIAN_POINT('Ctrl Pts',(0.194988341303727,0.0175821497898641,
0.258422711292167));
#23039=CARTESIAN_POINT('Ctrl Pts',(0.193507384081088,0.0297553772293582,
0.259117693768007));
#23040=CARTESIAN_POINT('Ctrl Pts',(0.190899892160004,0.041694018435488,
0.259812676243847));
#23041=CARTESIAN_POINT('Ctrl Pts',(0.188292767645379,0.0536309774374055,
0.260507560793766));
#23042=CARTESIAN_POINT('Ctrl Pts',(0.184559565079072,0.0653325517697591,
0.261202445343684));
#23043=CARTESIAN_POINT('Ctrl Pts',(0.179769087832285,0.0765782936604638,
0.261897329893602));
#23044=CARTESIAN_POINT('Ctrl Pts',(0.174978895351844,0.0878233670564318,
0.262592173136627));
#23045=CARTESIAN_POINT('Ctrl Pts',(0.169131920778233,0.0986118665811072,
0.263287016379651));
#23046=CARTESIAN_POINT('Ctrl Pts',(0.162344449782597,0.10874483723279,0.263981859622676));
#23047=CARTESIAN_POINT('Ctrl Pts',(0.155541335368905,0.11890116184004,0.264678304305079));
#23048=CARTESIAN_POINT('Ctrl Pts',(0.147793938166803,0.128398250377176,
0.265374748987482));
#23049=CARTESIAN_POINT('Ctrl Pts',(0.139260141812556,0.137068497118582,
0.266071193669885));
#23050=CARTESIAN_POINT('Ctrl Pts',(0.136474886887117,0.139898286632982,
0.266298498834133));
#23051=CARTESIAN_POINT('Ctrl Pts',(0.133606147718333,0.142640299256972,
0.26652580399838));
#23052=CARTESIAN_POINT('Ctrl Pts',(0.130660181228968,0.145289631568165,
0.266753109162628));
#23053=CARTESIAN_POINT('Ctrl Pts',(0.12163398421183,0.153406966062983,0.267449553335677));
#23054=CARTESIAN_POINT('Ctrl Pts',(0.111816502841543,0.160708680302889,
0.268145997508725));
#23055=CARTESIAN_POINT('Ctrl Pts',(0.101379644996105,0.167042891439485,
0.268842441681773));
#23056=CARTESIAN_POINT('Ctrl Pts',(0.0909646921136319,0.173363808281725,
0.269537424152071));
#23057=CARTESIAN_POINT('Ctrl Pts',(0.0799336453451763,0.178720738884986,
0.270232406622369));
#23058=CARTESIAN_POINT('Ctrl Pts',(0.0684888070103471,0.183003943439204,
0.270927389092667));
#23059=CARTESIAN_POINT('Ctrl Pts',(0.0570455813018427,0.187286544471711,
0.271622273636983));
#23060=CARTESIAN_POINT('Ctrl Pts',(0.0451894825021334,0.190495370158818,
0.2723171581813));
#23061=CARTESIAN_POINT('Ctrl Pts',(0.0331430414331587,0.192568685939744,
0.273012042725616));
#23062=CARTESIAN_POINT('Ctrl Pts',(0.0210973164565891,0.19464187847384,
0.273706885962999));
#23063=CARTESIAN_POINT('Ctrl Pts',(0.00886213927854251,0.195579572915857,
0.274401729200381));
#23064=CARTESIAN_POINT('Ctrl Pts',(-0.00333226908389658,0.195371584378979,
0.275096572437764));
#23065=CARTESIAN_POINT('Ctrl Pts',(-0.0155547824997445,0.195163116480678,
0.27579301711457));
#23066=CARTESIAN_POINT('Ctrl Pts',(-0.0277354655587635,0.193803773974419,
0.276489461791376));
#23067=CARTESIAN_POINT('Ctrl Pts',(-0.0396478794232672,0.191335322555032,
0.277185906468182));
#23068=CARTESIAN_POINT('Ctrl Pts',(-0.0435358458500477,0.19052967087487,
0.277413211660256));
#23069=CARTESIAN_POINT('Ctrl Pts',(-0.0473953334042183,0.189606276414027,
0.27764051685233));
#23070=CARTESIAN_POINT('Ctrl Pts',(-0.0512188292505198,0.188567737246344,
0.277867822044403));
#23071=CARTESIAN_POINT('Ctrl Pts',(-0.0629337020096656,0.185385739751415,
0.278564266217401));
#23072=CARTESIAN_POINT('Ctrl Pts',(-0.0743923830398956,0.181096613933035,
0.279260710390398));
#23073=CARTESIAN_POINT('Ctrl Pts',(-0.085374038891261,0.17576243479024,
0.279957154563396));
#23074=CARTESIAN_POINT('Ctrl Pts',(-0.0963326463526684,0.170439451066666,
0.280652137033613));
#23075=CARTESIAN_POINT('Ctrl Pts',(-0.106815403444239,0.164076079160796,
0.281347119503831));
#23076=CARTESIAN_POINT('Ctrl Pts',(-0.116620403215248,0.15678278462227,
0.282042101974049));
#23077=CARTESIAN_POINT('Ctrl Pts',(-0.126424021419587,0.149490517740336,
0.282736986518245));
#23078=CARTESIAN_POINT('Ctrl Pts',(-0.135549342818769,0.141269073197698,
0.283431871062442));
#23079=CARTESIAN_POINT('Ctrl Pts',(-0.143823825129738,0.132271944587847,
0.284126755606638));
#23080=CARTESIAN_POINT('Ctrl Pts',(-0.152097815569515,0.123275350806426,
0.284821598843877));
#23081=CARTESIAN_POINT('Ctrl Pts',(-0.159520494186149,0.113503827200428,
0.285516442081116));
#23082=CARTESIAN_POINT('Ctrl Pts',(-0.165958460600679,0.103145282757151,
0.286211285318355));
#23083=CARTESIAN_POINT('Ctrl Pts',(-0.172411264913106,0.0927628644669315,
0.286907729994984));
#23084=CARTESIAN_POINT('Ctrl Pts',(-0.177874419363226,0.0817915019588945,
0.287604174671613));
#23085=CARTESIAN_POINT('Ctrl Pts',(-0.182260223497348,0.0704440979124345,
0.288300619348242));
#23086=CARTESIAN_POINT('Ctrl Pts',(-0.183691659599983,0.0667405390378119,
0.288527924540888));
#23087=CARTESIAN_POINT('Ctrl Pts',(-0.185008724695846,0.0629970592217985,
0.288755229733534));
#23088=CARTESIAN_POINT('Ctrl Pts',(-0.186209527669695,0.0592213796278757,
0.28898253492618));
#23089=CARTESIAN_POINT('Ctrl Pts',(-0.190617370485671,0.0453618185375623,
0.289816914572349));
#23090=CARTESIAN_POINT('Ctrl Pts',(-0.193480354578723,0.0309884032053344,
0.290651294218517));
#23091=CARTESIAN_POINT('Ctrl Pts',(-0.1947089295262,0.0164192802144656,
0.291485673864686));
#23092=CARTESIAN_POINT('Ctrl Pts',(-0.195164087964002,0.0110217590666684,
0.291794792113486));
#23093=CARTESIAN_POINT('Ctrl Pts',(-0.195395379853359,0.00559758483881988,
0.292103910362286));
#23094=CARTESIAN_POINT('Ctrl Pts',(-0.195399931451662,0.000163672496008518,
0.292413028611086));
#23095=CARTESIAN_POINT('',(-0.195138177948142,-0.000106777846584659,0.36241303078758));
#23096=CARTESIAN_POINT('Ctrl Pts',(-0.195258340825392,0.000163515663356278,
0.29241303078758));
#23097=CARTESIAN_POINT('Ctrl Pts',(-0.194901896811807,-0.0448304971854093,
0.294974436461039));
#23098=CARTESIAN_POINT('Ctrl Pts',(-0.157071388863312,-0.155446575493477,
0.301240746428423));
#23099=CARTESIAN_POINT('Ctrl Pts',(0.0268669425771182,-0.229391098189835,
0.311211960689732));
#23100=CARTESIAN_POINT('Ctrl Pts',(0.207303956765325,-0.101819340194787,
0.322326673571509));
#23101=CARTESIAN_POINT('Ctrl Pts',(0.197964422771547,0.118963001998054,
0.333441386453286));
#23102=CARTESIAN_POINT('Ctrl Pts',(0.00739822334892354,0.230840583131222,
0.344556099335061));
#23103=CARTESIAN_POINT('Ctrl Pts',(-0.164063175527352,0.144435526251838,
0.354213314113159));
#23104=CARTESIAN_POINT('Ctrl Pts',(-0.19494196408341,0.0394326521564634,
0.360165624597332));
#23105=CARTESIAN_POINT('Ctrl Pts',(-0.195138177948142,-0.000106777846584659,
0.36241303078758));
#23106=CARTESIAN_POINT('',(-0.195399971017471,-0.000106425426877684,0.43241303078758));
#23107=CARTESIAN_POINT('Ctrl Pts',(-0.195138177948142,-0.000106777846584659,
0.36241303078758));
#23108=CARTESIAN_POINT('Ctrl Pts',(-0.195265427457823,-0.0257490691689222,
0.363870528891258));
#23109=CARTESIAN_POINT('Ctrl Pts',(-0.17864031290789,-0.116414623642343,
0.369032931288858));
#23110=CARTESIAN_POINT('Ctrl Pts',(-0.0415002571887793,-0.227199993798136,
0.377900237980392));
#23111=CARTESIAN_POINT('Ctrl Pts',(0.168389188041786,-0.158073368658769,
0.389014950862164));
#23112=CARTESIAN_POINT('Ctrl Pts',(0.224126636583553,0.0557616293005508,
0.400129663743943));
#23113=CARTESIAN_POINT('Ctrl Pts',(0.0746872032705934,0.218549605801867,
0.411244376625718));
#23114=CARTESIAN_POINT('Ctrl Pts',(-0.136194829554037,0.182452397202414,
0.422005466425645));
#23115=CARTESIAN_POINT('Ctrl Pts',(-0.195262132691462,0.0584632240203973,
0.429061651931645));
#23116=CARTESIAN_POINT('Ctrl Pts',(-0.195647644016423,-0.000104853873465957,
0.432412933143721));
#23117=CARTESIAN_POINT('',(-0.195399922987737,0.000173483101027086,0.502413030787579));
#23118=CARTESIAN_POINT('Ctrl Pts',(-0.195399971017471,-0.000106425426877684,
0.43241303078758));
#23119=CARTESIAN_POINT('Ctrl Pts',(-0.195396609620896,-0.00627804073125874,
0.432766621321477));
#23120=CARTESIAN_POINT('Ctrl Pts',(-0.19510088201498,-0.0124415176703404,
0.433120211855374));
#23121=CARTESIAN_POINT('Ctrl Pts',(-0.194514937660211,-0.0185768411481667,
0.433473802389271));
#23122=CARTESIAN_POINT('Ctrl Pts',(-0.193360841345552,-0.0306611869693582,
0.434170246563104));
#23123=CARTESIAN_POINT('Ctrl Pts',(-0.191072232655043,-0.0426803484164101,
0.434866690736937));
#23124=CARTESIAN_POINT('Ctrl Pts',(-0.187672929088017,-0.0544061732483001,
0.43556313491077));
#23125=CARTESIAN_POINT('Ctrl Pts',(-0.184280760007233,-0.0661073878227418,
0.436258117381852));
#23126=CARTESIAN_POINT('Ctrl Pts',(-0.179782692702317,-0.0775156343635371,
0.436953099852933));
#23127=CARTESIAN_POINT('Ctrl Pts',(-0.174253439762954,-0.0884132271256893,
0.437648082324015));
#23128=CARTESIAN_POINT('Ctrl Pts',(-0.168724965918913,-0.099309284370541,
0.438342966869103));
#23129=CARTESIAN_POINT('Ctrl Pts',(-0.162165949397607,-0.109694030088432,
0.43903785141419));
#23130=CARTESIAN_POINT('Ctrl Pts',(-0.154698478704145,-0.119371439995601,
0.439732735959278));
#23131=CARTESIAN_POINT('Ctrl Pts',(-0.147231451909415,-0.129048274635699,
0.440427579197425));
#23132=CARTESIAN_POINT('Ctrl Pts',(-0.138856634330092,-0.138017179935642,
0.441122422435572));
#23133=CARTESIAN_POINT('Ctrl Pts',(-0.129736656101347,-0.146114886523039,
0.441817265673719));
#23134=CARTESIAN_POINT('Ctrl Pts',(-0.120595658610059,-0.154231256293231,
0.442513710351264));
#23135=CARTESIAN_POINT('Ctrl Pts',(-0.110706769418908,-0.161471886288798,
0.44321015502881));
#23136=CARTESIAN_POINT('Ctrl Pts',(-0.100264983963729,-0.167714319575739,
0.443906599706355));
#23137=CARTESIAN_POINT('Ctrl Pts',(-0.0968570004082841,-0.169751721136916,
0.444133904894586));
#23138=CARTESIAN_POINT('Ctrl Pts',(-0.0933903211066352,-0.171683154698311,
0.444361210082816));
#23139=CARTESIAN_POINT('Ctrl Pts',(-0.0898722359545557,-0.173505450071543,
0.444588515271047));
#23140=CARTESIAN_POINT('Ctrl Pts',(-0.0790931159252374,-0.179088811391074,
0.445284959444882));
#23141=CARTESIAN_POINT('Ctrl Pts',(-0.0677535465776804,-0.183683606124434,
0.445981403618718));
#23142=CARTESIAN_POINT('Ctrl Pts',(-0.0560581373434789,-0.187186124586145,
0.446677847792554));
#23143=CARTESIAN_POINT('Ctrl Pts',(-0.0443872745302157,-0.190681291933347,
0.447372830263638));
#23144=CARTESIAN_POINT('Ctrl Pts',(-0.0323628632506873,-0.193088413034795,
0.448067812734723));
#23145=CARTESIAN_POINT('Ctrl Pts',(-0.0202083180909325,-0.194352216040712,
0.448762795205808));
#23146=CARTESIAN_POINT('Ctrl Pts',(-0.00805548555843536,-0.195615840971395,
0.449457679750898));
#23147=CARTESIAN_POINT('Ctrl Pts',(0.00422657955392215,-0.19573633133975,
0.450152564295988));
#23148=CARTESIAN_POINT('Ctrl Pts',(0.0164069718891545,-0.194709967062368,
0.450847448841078));
#23149=CARTESIAN_POINT('Ctrl Pts',(0.0285866401692253,-0.193683663796515,
0.451542292079227));
#23150=CARTESIAN_POINT('Ctrl Pts',(0.0406637772497165,-0.191510741408034,
0.452237135317377));
#23151=CARTESIAN_POINT('Ctrl Pts',(0.0524130137934869,-0.188239305101468,
0.452931978555526));
#23152=CARTESIAN_POINT('Ctrl Pts',(0.0641893293808049,-0.184960328954686,
0.453628423233074));
#23153=CARTESIAN_POINT('Ctrl Pts',(0.0756354100046736,-0.180578081754846,
0.454324867910622));
#23154=CARTESIAN_POINT('Ctrl Pts',(0.0865426261085684,-0.175189993624729,
0.45502131258817));
#23155=CARTESIAN_POINT('Ctrl Pts',(0.0901025166344817,-0.173431432713816,
0.455248617776388));
#23156=CARTESIAN_POINT('Ctrl Pts',(0.0936052019270259,-0.171566091800692,
0.455475922964606));
#23157=CARTESIAN_POINT('Ctrl Pts',(0.0970440652641103,-0.1695983767523,
0.455703228152823));
#23158=CARTESIAN_POINT('Ctrl Pts',(0.107580456248006,-0.163569461653763,
0.456399672326659));
#23159=CARTESIAN_POINT('Ctrl Pts',(0.117590169783062,-0.156533581710509,
0.457096116500494));
#23160=CARTESIAN_POINT('Ctrl Pts',(0.126875114348702,-0.148606410894698,
0.45779256067433));
#23161=CARTESIAN_POINT('Ctrl Pts',(0.136140571596443,-0.140695877690089,
0.458487543145414));
#23162=CARTESIAN_POINT('Ctrl Pts',(0.144683571368738,-0.131898272703116,
0.459182525616499));
#23163=CARTESIAN_POINT('Ctrl Pts',(0.152336522117895,-0.122371336631681,
0.459877508087583));
#23164=CARTESIAN_POINT('Ctrl Pts',(0.159988394533649,-0.112845742946173,
0.460572392632673));
#23165=CARTESIAN_POINT('Ctrl Pts',(0.166749883378749,-0.10259167497533,
0.461267277177763));
#23166=CARTESIAN_POINT('Ctrl Pts',(0.172492648910389,-0.0918011223889852,
0.461962161722853));
#23167=CARTESIAN_POINT('Ctrl Pts',(0.178235073067225,-0.0810112112397224,
0.462657004961003));
#23168=CARTESIAN_POINT('Ctrl Pts',(0.182958506296677,-0.0696856644408173,
0.463351848199152));
#23169=CARTESIAN_POINT('Ctrl Pts',(0.186581154572559,-0.0580399238315401,
0.464046691437302));
#23170=CARTESIAN_POINT('Ctrl Pts',(0.190212152144164,-0.0463673427108855,
0.46474313611485));
#23171=CARTESIAN_POINT('Ctrl Pts',(0.192737101910838,-0.0343739494944365,
0.465439580792398));
#23172=CARTESIAN_POINT('Ctrl Pts',(0.194124730264744,-0.0222878688896088,
0.466136025469946));
#23173=CARTESIAN_POINT('Ctrl Pts',(0.194577623558826,-0.0183432212883551,
0.466363330658164));
#23174=CARTESIAN_POINT('Ctrl Pts',(0.194909779209757,-0.0143887335080788,
0.466590635846381));
#23175=CARTESIAN_POINT('Ctrl Pts',(0.195121310951865,-0.0104323541171564,
0.466817941034599));
#23176=CARTESIAN_POINT('Ctrl Pts',(0.195769426599936,0.00168966297313779,
0.467514385208434));
#23177=CARTESIAN_POINT('Ctrl Pts',(0.195285885260745,0.0139152165149137,
0.468210829382269));
#23178=CARTESIAN_POINT('Ctrl Pts',(0.193660456341936,0.0260151426948438,
0.468907273556104));
#23179=CARTESIAN_POINT('Ctrl Pts',(0.192038438886689,0.0380896734503476,
0.469602256027188));
#23180=CARTESIAN_POINT('Ctrl Pts',(0.189279332201416,0.0500382310585006,
0.470297238498273));
#23181=CARTESIAN_POINT('Ctrl Pts',(0.185424789573062,0.0616344661028701,
0.470992220969357));
#23182=CARTESIAN_POINT('Ctrl Pts',(0.181570790066204,0.0732290671882591,
0.471687105514446));
#23183=CARTESIAN_POINT('Ctrl Pts',(0.176621893083348,0.0844706000021562,
0.472381990059536));
#23184=CARTESIAN_POINT('Ctrl Pts',(0.170669813200684,0.0951471221952799,
0.473076874604625));
#23185=CARTESIAN_POINT('Ctrl Pts',(0.164718087135373,0.105823009729781,
0.473771717842774));
#23186=CARTESIAN_POINT('Ctrl Pts',(0.157763746352208,0.115933201421272,
0.474466561080923));
#23187=CARTESIAN_POINT('Ctrl Pts',(0.149943450532847,0.125292145174004,
0.475161404319072));
#23188=CARTESIAN_POINT('Ctrl Pts',(0.142105130892935,0.134672658944884,
0.475857848996619));
#23189=CARTESIAN_POINT('Ctrl Pts',(0.13339748282169,0.143297838203064,0.476554293674167));
#23190=CARTESIAN_POINT('Ctrl Pts',(0.12399521810552,0.151017700575014,0.477250738351715));
#23191=CARTESIAN_POINT('Ctrl Pts',(0.120926512693726,0.153537304537915,
0.477478043539935));
#23192=CARTESIAN_POINT('Ctrl Pts',(0.117784066586514,0.155960800658072,
0.477705348728155));
#23193=CARTESIAN_POINT('Ctrl Pts',(0.114574619856465,0.158283974187997,
0.477932653916375));
#23194=CARTESIAN_POINT('Ctrl Pts',(0.104741142258005,0.165401984482409,
0.478629098090211));
#23195=CARTESIAN_POINT('Ctrl Pts',(0.0942070042923155,0.17162532032016,
0.479325542264046));
#23196=CARTESIAN_POINT('Ctrl Pts',(0.0831592018979891,0.176821116215483,
0.480021986437881));
#23197=CARTESIAN_POINT('Ctrl Pts',(0.0721345867220473,0.182006007131716,
0.480716968908965));
#23198=CARTESIAN_POINT('Ctrl Pts',(0.060599199670287,0.186167202174279,
0.48141195138005));
#23199=CARTESIAN_POINT('Ctrl Pts',(0.0487658073344321,0.189216954935389,
0.482106933851134));
#23200=CARTESIAN_POINT('Ctrl Pts',(0.0369340823740317,0.192266277973327,
0.482801818396224));
#23201=CARTESIAN_POINT('Ctrl Pts',(0.0248052706711634,0.194204206772151,
0.483496702941313));
#23202=CARTESIAN_POINT('Ctrl Pts',(0.0126071809498785,0.194992869070889,
0.484191587486403));
#23203=CARTESIAN_POINT('Ctrl Pts',(0.000409816335766259,0.195781484488132,
0.484886430724552));
#23204=CARTESIAN_POINT('Ctrl Pts',(-0.0118559424614858,0.19542093921384,
0.485581273962701));
#23205=CARTESIAN_POINT('Ctrl Pts',(-0.0239600872508721,0.193925434688002,
0.48627611720085));
#23206=CARTESIAN_POINT('Ctrl Pts',(-0.0360921290583036,0.192426483399302,
0.486972561878398));
#23207=CARTESIAN_POINT('Ctrl Pts',(-0.0480609526199101,0.189787522482648,
0.487669006555946));
#23208=CARTESIAN_POINT('Ctrl Pts',(-0.0596458007786993,0.186074013364219,
0.488365451233494));
#23209=CARTESIAN_POINT('Ctrl Pts',(-0.0634268564405725,0.184862000527694,
0.488592756421713));
#23210=CARTESIAN_POINT('Ctrl Pts',(-0.0671671498803667,0.183535913816646,
0.488820061609932));
#23211=CARTESIAN_POINT('Ctrl Pts',(-0.0708594848912776,0.182099130697933,
0.489047366798151));
#23212=CARTESIAN_POINT('Ctrl Pts',(-0.0821724919825079,0.177696946832565,
0.489743810971986));
#23213=CARTESIAN_POINT('Ctrl Pts',(-0.093113742811342,0.172220907942076,
0.490440255145822));
#23214=CARTESIAN_POINT('Ctrl Pts',(-0.10347020046737,0.165756078667547,
0.491136699319657));
#23215=CARTESIAN_POINT('Ctrl Pts',(-0.113804921905028,0.159304817829786,
0.491831681790741));
#23216=CARTESIAN_POINT('Ctrl Pts',(-0.12355651140328,0.151869281475647,
0.492526664261825));
#23217=CARTESIAN_POINT('Ctrl Pts',(-0.132535866386685,0.143580653714666,
0.49322164673291));
#23218=CARTESIAN_POINT('Ctrl Pts',(-0.141513956140674,0.135293193856689,
0.493916531277999));
#23219=CARTESIAN_POINT('Ctrl Pts',(-0.149719353643204,0.126153440403864,
0.494611415823089));
#23220=CARTESIAN_POINT('Ctrl Pts',(-0.156996703673694,0.116332261370587,
0.495306300368179));
#23221=CARTESIAN_POINT('Ctrl Pts',(-0.164273621107045,0.106511666150637,
0.496001143606328));
#23222=CARTESIAN_POINT('Ctrl Pts',(-0.170622100687362,0.0960104453270628,
0.496695986844477));
#23223=CARTESIAN_POINT('Ctrl Pts',(-0.17592934686914,0.0850295531576978,
0.497390830082626));
#23224=CARTESIAN_POINT('Ctrl Pts',(-0.181248824922321,0.0740233527858678,
0.498087274760174));
#23225=CARTESIAN_POINT('Ctrl Pts',(-0.185521956306638,0.0625360902598858,
0.498783719437722));
#23226=CARTESIAN_POINT('Ctrl Pts',(-0.188684030783989,0.0507887440985386,
0.499480164115269));
#23227=CARTESIAN_POINT('Ctrl Pts',(-0.189716066719374,0.0469546524378999,
0.499707469303489));
#23228=CARTESIAN_POINT('Ctrl Pts',(-0.190630153319104,0.0430929498769562,
0.499934774491708));
#23229=CARTESIAN_POINT('Ctrl Pts',(-0.19142522601456,0.0392115141925761,
0.500162079679927));
#23230=CARTESIAN_POINT('Ctrl Pts',(-0.194049700153669,0.0263991919552629,
0.500912396715811));
#23231=CARTESIAN_POINT('Ctrl Pts',(-0.195388255538518,0.0133149283794744,
0.501662713751695));
#23232=CARTESIAN_POINT('Ctrl Pts',(-0.195399922987737,0.000173483101027086,
0.502413030787579));
#23233=CARTESIAN_POINT('',(-0.195079266632945,-5.12429904213991E-7,0.57241303078758));
#23234=CARTESIAN_POINT('Ctrl Pts',(-0.195459766443919,0.000172969825184949,
0.502413063116928));
#23235=CARTESIAN_POINT('Ctrl Pts',(-0.194982758876813,-0.0515913455672025,
0.50536763959852));
#23236=CARTESIAN_POINT('Ctrl Pts',(-0.147284875895773,-0.169042238585059,
0.512027120374039));
#23237=CARTESIAN_POINT('Ctrl Pts',(0.0509580899086067,-0.225267355827217,
0.522391505443478));
#23238=CARTESIAN_POINT('Ctrl Pts',(0.21690320188124,-0.0793417263625358,
0.533506218325257));
#23239=CARTESIAN_POINT('Ctrl Pts',(0.184284130208876,0.139217340448956,
0.544620931207032));
#23240=CARTESIAN_POINT('Ctrl Pts',(-0.0170379737667661,0.230329798285947,
0.555735644088809));
#23241=CARTESIAN_POINT('Ctrl Pts',(-0.17183815729343,0.130524775720848,
0.564999677282324));
#23242=CARTESIAN_POINT('Ctrl Pts',(-0.19507850314188,0.0326461576927833,
0.570558806181915));
#23243=CARTESIAN_POINT('Ctrl Pts',(-0.195079266632945,-5.12429904213991E-7,
0.57241303078758));
#23244=CARTESIAN_POINT('',(-0.195399923222036,-0.000173219001145046,0.64241303078758));
#23245=CARTESIAN_POINT('Ctrl Pts',(-0.195079266632945,-5.12429904213991E-7,
0.57241303078758));
#23246=CARTESIAN_POINT('Ctrl Pts',(-0.195080028664364,-0.0325847684584389,
0.57426371047584));
#23247=CARTESIAN_POINT('Ctrl Pts',(-0.171903476033457,-0.130398931487736,
0.579819294458025));
#23248=CARTESIAN_POINT('Ctrl Pts',(-0.0172578326063497,-0.230313429357155,
0.589079782734138));
#23249=CARTESIAN_POINT('Ctrl Pts',(0.18415115313644,-0.139393189672384,
0.600194495615913));
#23250=CARTESIAN_POINT('Ctrl Pts',(0.216978840527336,0.0791346402780385,
0.61130920849769));
#23251=CARTESIAN_POINT('Ctrl Pts',(0.0511731008232275,0.225218609978527,
0.622423921379466));
#23252=CARTESIAN_POINT('Ctrl Pts',(-0.147191262382175,0.169163591660262,
0.632791851033313));
#23253=CARTESIAN_POINT('Ctrl Pts',(-0.194984294593638,0.0516524436523172,
0.639454876393235));
#23254=CARTESIAN_POINT('Ctrl Pts',(-0.195461647808511,-0.000172689824079368,
0.642412997459232));
#23255=CARTESIAN_POINT('',(-0.195399970524701,0.000107326353575181,0.712413030787581));
#23256=CARTESIAN_POINT('Ctrl Pts',(-0.195399923222036,-0.000173219001145046,
0.64241303078758));
#23257=CARTESIAN_POINT('Ctrl Pts',(-0.195388328972743,-0.0132521272423538,
0.643159802906059));
#23258=CARTESIAN_POINT('Ctrl Pts',(-0.194062470003487,-0.0262744897130095,
0.643906575024539));
#23259=CARTESIAN_POINT('Ctrl Pts',(-0.191462569052284,-0.0390287669789766,
0.644653347143019));
#23260=CARTESIAN_POINT('Ctrl Pts',(-0.189037885771796,-0.0509234827477472,
0.645349791316854));
#23261=CARTESIAN_POINT('Ctrl Pts',(-0.185491931481621,-0.0626334861551503,
0.646046235490689));
#23262=CARTESIAN_POINT('Ctrl Pts',(-0.180872500984137,-0.0739344195063672,
0.646742679664524));
#23263=CARTESIAN_POINT('Ctrl Pts',(-0.176262765785313,-0.0852116343658677,
0.647437662135608));
#23264=CARTESIAN_POINT('Ctrl Pts',(-0.170584285221288,-0.0960806525873972,
0.648132644606691));
#23265=CARTESIAN_POINT('Ctrl Pts',(-0.163934358114472,-0.106332902855118,
0.648827627077775));
#23266=CARTESIAN_POINT('Ctrl Pts',(-0.15728536801075,-0.116583708537047,
0.649522511622864));
#23267=CARTESIAN_POINT('Ctrl Pts',(-0.14966564023064,-0.126217160146402,
0.650217396167953));
#23268=CARTESIAN_POINT('Ctrl Pts',(-0.141217295086143,-0.135051233124889,
0.650912280713043));
#23269=CARTESIAN_POINT('Ctrl Pts',(-0.132769452147797,-0.143884780967896,
0.651607123951191));
#23270=CARTESIAN_POINT('Ctrl Pts',(-0.123493714240925,-0.151918430079598,
0.652301967189339));
#23271=CARTESIAN_POINT('Ctrl Pts',(-0.113569054817426,-0.159007011756955,
0.652996810427488));
#23272=CARTESIAN_POINT('Ctrl Pts',(-0.10362152154304,-0.166111930837277,
0.653693255105035));
#23273=CARTESIAN_POINT('Ctrl Pts',(-0.0930228308847063,-0.172266978237357,
0.654389699782582));
#23274=CARTESIAN_POINT('Ctrl Pts',(-0.0819798273856736,-0.177370989459424,
0.655086144460129));
#23275=CARTESIAN_POINT('Ctrl Pts',(-0.0783756186526551,-0.179036833522736,
0.65531344964835));
#23276=CARTESIAN_POINT('Ctrl Pts',(-0.0747242413317422,-0.18059110011559,
0.655540754836572));
#23277=CARTESIAN_POINT('Ctrl Pts',(-0.0710332795173808,-0.182031407182952,
0.655768060024794));
#23278=CARTESIAN_POINT('Ctrl Pts',(-0.0597244797861847,-0.186444388133568,
0.656464504198629));
#23279=CARTESIAN_POINT('Ctrl Pts',(-0.047962838762106,-0.189815110912198,
0.657160948372464));
#23280=CARTESIAN_POINT('Ctrl Pts',(-0.0359627799780109,-0.192062069280358,
0.6578573925463));
#23281=CARTESIAN_POINT('Ctrl Pts',(-0.0239879070158319,-0.194304311713844,
0.658552375017384));
#23282=CARTESIAN_POINT('Ctrl Pts',(-0.0117764478623286,-0.195427238229025,
0.659247357488468));
#23283=CARTESIAN_POINT('Ctrl Pts',(0.000443592909847119,-0.195399496481773,
0.659942339959553));
#23284=CARTESIAN_POINT('Ctrl Pts',(0.0126619118261549,-0.195371758643451,
0.660637224504643));
#23285=CARTESIAN_POINT('Ctrl Pts',(0.0248879355031087,-0.194193630295803,
0.661332109049732));
#23286=CARTESIAN_POINT('Ctrl Pts',(0.03689165842973,-0.191885813801605,
0.662026993594822));
#23287=CARTESIAN_POINT('Ctrl Pts',(0.0488946678031806,-0.189578134493993,
0.662721836832971));
#23288=CARTESIAN_POINT('Ctrl Pts',(0.060674547700274,-0.186141091960471,
0.663416680071121));
#23289=CARTESIAN_POINT('Ctrl Pts',(0.072012274422929,-0.181646338615555,
0.66411152330927));
#23290=CARTESIAN_POINT('Ctrl Pts',(0.0833761317622014,-0.177141225991453,
0.664807967986818));
#23291=CARTESIAN_POINT('Ctrl Pts',(0.0942950118476686,-0.171573918756561,
0.665504412664366));
#23292=CARTESIAN_POINT('Ctrl Pts',(0.104571749584314,-0.165063349017508,
0.666200857341914));
#23293=CARTESIAN_POINT('Ctrl Pts',(0.107925864966069,-0.162938433245075,
0.666428162530133));
#23294=CARTESIAN_POINT('Ctrl Pts',(0.111211811144147,-0.1607133807298,0.666655467718352));
#23295=CARTESIAN_POINT('Ctrl Pts',(0.11442347405062,-0.15839327190947,0.666882772906571));
#23296=CARTESIAN_POINT('Ctrl Pts',(0.124263741829205,-0.151284651630083,
0.667579217080406));
#23297=CARTESIAN_POINT('Ctrl Pts',(0.133473867314389,-0.14323036332032,
0.668275661254241));
#23298=CARTESIAN_POINT('Ctrl Pts',(0.141869092411777,-0.134366367139469,
0.668972105428076));
#23299=CARTESIAN_POINT('Ctrl Pts',(0.150246697541793,-0.12552097478659,
0.669667087899161));
#23300=CARTESIAN_POINT('Ctrl Pts',(0.15781214669954,-0.115869825753562,
0.670362070370245));
#23301=CARTESIAN_POINT('Ctrl Pts',(0.164415456503192,-0.105587488192717,
0.671057052841329));
#23302=CARTESIAN_POINT('Ctrl Pts',(0.171017835872326,-0.0953065994570916,
0.671751937386419));
#23303=CARTESIAN_POINT('Ctrl Pts',(0.176657833757992,-0.084395409549357,
0.672446821931509));
#23304=CARTESIAN_POINT('Ctrl Pts',(0.18122811815165,-0.0730583957612789,
0.673141706476599));
#23305=CARTESIAN_POINT('Ctrl Pts',(0.18579813086785,-0.0617220558942993,
0.673836549714748));
#23306=CARTESIAN_POINT('Ctrl Pts',(0.189298253693658,-0.0499607646398732,
0.674531392952897));
#23307=CARTESIAN_POINT('Ctrl Pts',(0.191669918078142,-0.0379974012784856,
0.675226236191046));
#23308=CARTESIAN_POINT('Ctrl Pts',(0.194047048554224,-0.0260064653649362,
0.675922680868594));
#23309=CARTESIAN_POINT('Ctrl Pts',(0.195290421868306,-0.0138133986887334,
0.676619125546141));
#23310=CARTESIAN_POINT('Ctrl Pts',(0.195393047293897,-0.00164835348302706,
0.677315570223689));
#23311=CARTESIAN_POINT('Ctrl Pts',(0.195426542117581,0.00232206653642397,
0.677542875411908));
#23312=CARTESIAN_POINT('Ctrl Pts',(0.195338935489874,0.00628951232178161,
0.677770180600127));
#23313=CARTESIAN_POINT('Ctrl Pts',(0.19513118049701,0.0102460918326651,
0.677997485788346));
#23314=CARTESIAN_POINT('Ctrl Pts',(0.194494636494213,0.0223687220737979,
0.678693929962181));
#23315=CARTESIAN_POINT('Ctrl Pts',(0.19272183080269,0.0344747177622865,
0.679390374136016));
#23316=CARTESIAN_POINT('Ctrl Pts',(0.189826807689656,0.0463351171613335,
0.680086818309852));
#23317=CARTESIAN_POINT('Ctrl Pts',(0.186937860674904,0.0581706238567293,
0.680781800780936));
#23318=CARTESIAN_POINT('Ctrl Pts',(0.182931504261327,0.0697606974934034,
0.68147678325202));
#23319=CARTESIAN_POINT('Ctrl Pts',(0.177873078646798,0.0808846579563145,
0.682171765723104));
#23320=CARTESIAN_POINT('Ctrl Pts',(0.172815365786014,0.092007051005748,
0.682866650268194));
#23321=CARTESIAN_POINT('Ctrl Pts',(0.166706197981058,0.102662646253495,
0.683561534813284));
#23322=CARTESIAN_POINT('Ctrl Pts',(0.159659173886027,0.11265038035458,0.684256419358373));
#23323=CARTESIAN_POINT('Ctrl Pts',(0.152612568696564,0.122637520741584,
0.684951262596522));
#23324=CARTESIAN_POINT('Ctrl Pts',(0.144628744630301,0.131956178640988,
0.685646105834671));
#23325=CARTESIAN_POINT('Ctrl Pts',(0.135863204903233,0.140436282895205,
0.686340949072821));
#23326=CARTESIAN_POINT('Ctrl Pts',(0.127077462805474,0.148935931662935,
0.687037393750368));
#23327=CARTESIAN_POINT('Ctrl Pts',(0.117507082402367,0.156592606601072,
0.687733838427916));
#23328=CARTESIAN_POINT('Ctrl Pts',(0.107341647001269,0.163275628368275,
0.688430283105464));
#23329=CARTESIAN_POINT('Ctrl Pts',(0.104023858407757,0.165456828928265,
0.688657588293683));
#23330=CARTESIAN_POINT('Ctrl Pts',(0.100642898521159,0.167534667041848,
0.688884893481903));
#23331=CARTESIAN_POINT('Ctrl Pts',(0.0972059150784287,0.169505663839782,
0.689112198670122));
#23332=CARTESIAN_POINT('Ctrl Pts',(0.086675283934427,0.175544633945664,
0.689808642843958));
#23333=CARTESIAN_POINT('Ctrl Pts',(0.0755424632419164,0.180619895028409,
0.690505087017793));
#23334=CARTESIAN_POINT('Ctrl Pts',(0.0640074427957508,0.184619086951346,
0.691201531191628));
#23335=CARTESIAN_POINT('Ctrl Pts',(0.052496632145219,0.188609885337435,
0.691896513662712));
#23336=CARTESIAN_POINT('Ctrl Pts',(0.0405860918632403,0.19152874278642,
0.692591496133797));
#23337=CARTESIAN_POINT('Ctrl Pts',(0.0284966699988162,0.193310888981916,
0.693286478604881));
#23338=CARTESIAN_POINT('Ctrl Pts',(0.016408951585498,0.195092784065411,
0.69398136314997));
#23339=CARTESIAN_POINT('Ctrl Pts',(0.00414325991087987,0.195738112738375,
0.69467624769506));
#23340=CARTESIAN_POINT('Ctrl Pts',(-0.0080698696734386,0.195233289178495,
0.69537113224015));
#23341=CARTESIAN_POINT('Ctrl Pts',(-0.0202822732565491,0.194728495627508,
0.696065975478299));
#23342=CARTESIAN_POINT('Ctrl Pts',(-0.0324412470448402,0.193073748461682,
0.696760818716448));
#23343=CARTESIAN_POINT('Ctrl Pts',(-0.0443195715802094,0.190307476403179,
0.697455661954597));
#23344=CARTESIAN_POINT('Ctrl Pts',(-0.0562252726745748,0.187534828781357,
0.698152106632145));
#23345=CARTESIAN_POINT('Ctrl Pts',(-0.0678481955474909,0.183645803703173,
0.698848551309693));
#23346=CARTESIAN_POINT('Ctrl Pts',(-0.0789757370253823,0.178728825210982,
0.699544995987241));
#23347=CARTESIAN_POINT('Ctrl Pts',(-0.0826075372122331,0.177124024775759,
0.69977230117546));
#23348=CARTESIAN_POINT('Ctrl Pts',(-0.0861867483306558,0.17541009690366,
0.699999606363679));
#23349=CARTESIAN_POINT('Ctrl Pts',(-0.0897065713936311,0.173591160629795,
0.700226911551899));
#23350=CARTESIAN_POINT('Ctrl Pts',(-0.100491016237783,0.168018091310812,
0.700923355725734));
#23351=CARTESIAN_POINT('Ctrl Pts',(-0.110792303658588,0.161416466578702,
0.701619799899569));
#23352=CARTESIAN_POINT('Ctrl Pts',(-0.120407579127232,0.153893388060434,
0.702316244073404));
#23353=CARTESIAN_POINT('Ctrl Pts',(-0.130002673976764,0.146386099041138,
0.703011226544489));
#23354=CARTESIAN_POINT('Ctrl Pts',(-0.138913885927463,0.137961670266092,
0.703706209015573));
#23355=CARTESIAN_POINT('Ctrl Pts',(-0.14696703457582,0.128770535247741,
0.704401191486657));
#23356=CARTESIAN_POINT('Ctrl Pts',(-0.155019048501184,0.119580695299517,
0.705096076031747));
#23357=CARTESIAN_POINT('Ctrl Pts',(-0.162212628261905,0.109624990825244,
0.705790960576836));
#23358=CARTESIAN_POINT('Ctrl Pts',(-0.168411345553256,0.0990897506755452,
0.706485845121926));
#23359=CARTESIAN_POINT('Ctrl Pts',(-0.17460969436606,0.0885551367860546,
0.707180688360075));
#23360=CARTESIAN_POINT('Ctrl Pts',(-0.179812877054423,0.0774418239730975,
0.707875531598224));
#23361=CARTESIAN_POINT('Ctrl Pts',(-0.18392996612555,0.0659615612387541,
0.708570374836373));
#23362=CARTESIAN_POINT('Ctrl Pts',(-0.18805654405443,0.0544548393780323,
0.709266819513921));
#23363=CARTESIAN_POINT('Ctrl Pts',(-0.191091796750165,0.0425803249356859,
0.709963264191469));
#23364=CARTESIAN_POINT('Ctrl Pts',(-0.192994728892767,0.0305645974880667,
0.710659708869017));
#23365=CARTESIAN_POINT('Ctrl Pts',(-0.193615806722475,0.0266429117072331,
0.710887014057236));
#23366=CARTESIAN_POINT('Ctrl Pts',(-0.194116677820692,0.0227062342853432,
0.711114319245456));
#23367=CARTESIAN_POINT('Ctrl Pts',(-0.194497116087621,0.018762511388367,
0.711341624433675));
#23368=CARTESIAN_POINT('Ctrl Pts',(-0.195094849879869,0.0125662460604494,
0.711698759884977));
#23369=CARTESIAN_POINT('Ctrl Pts',(-0.195396546603586,0.00634096853455841,
0.712055895336279));
#23370=CARTESIAN_POINT('Ctrl Pts',(-0.195399970524701,0.000107326353575181,
0.712413030787581));
#23371=CARTESIAN_POINT('',(-0.195137151677628,0.000105948740446043,0.78241303078758));
#23372=CARTESIAN_POINT('Ctrl Pts',(-0.195646315966217,0.000105752649902963,
0.712413128576354));
#23373=CARTESIAN_POINT('Ctrl Pts',(-0.195258600286138,-0.0584014188700451,
0.715760864822719));
#23374=CARTESIAN_POINT('Ctrl Pts',(-0.136299473324216,-0.18233426378207,
0.72281350536301));
#23375=CARTESIAN_POINT('Ctrl Pts',(0.0744785476940125,-0.218620800615839,
0.733571050197228));
#23376=CARTESIAN_POINT('Ctrl Pts',(0.224073305925668,-0.0559755491269474,
0.744685763079003));
#23377=CARTESIAN_POINT('Ctrl Pts',(0.168540003889559,0.157912556870666,
0.75580047596078));
#23378=CARTESIAN_POINT('Ctrl Pts',(-0.0412833593056294,0.227239505308745,
0.766915188842555));
#23379=CARTESIAN_POINT('Ctrl Pts',(-0.178583972525577,0.116540859079365,
0.77578604045149));
#23380=CARTESIAN_POINT('Ctrl Pts',(-0.195263680442012,0.025810945614826,
0.780951987766498));
#23381=CARTESIAN_POINT('Ctrl Pts',(-0.195137151677628,0.000105948740446043,
0.78241303078758));
#23382=CARTESIAN_POINT('',(-0.195399931100211,-0.000164091537283115,0.852413032945658));
#23383=CARTESIAN_POINT('Ctrl Pts',(-0.195137151677628,0.000105948740446043,
0.78241303078758));
#23384=CARTESIAN_POINT('Ctrl Pts',(-0.194942829545969,-0.0393716341730415,
0.784656892060423));
#23385=CARTESIAN_POINT('Ctrl Pts',(-0.164138066225684,-0.144310627331788,
0.790605657627189));
#23386=CARTESIAN_POINT('Ctrl Pts',(0.00717786579426044,-0.230847540102041,
0.800259327487886));
#23387=CARTESIAN_POINT('Ctrl Pts',(0.197850773711331,-0.119151919289399,
0.811374040369659));
#23388=CARTESIAN_POINT('Ctrl Pts',(0.207401056306211,0.101621407053779,
0.822488753251437));
#23389=CARTESIAN_POINT('Ctrl Pts',(0.0270859008837076,0.229365347212347,
0.833603466133214));
#23390=CARTESIAN_POINT('Ctrl Pts',(-0.156988350126302,0.155570214827098,
0.843578225311926));
#23391=CARTESIAN_POINT('Ctrl Pts',(-0.194901910843352,0.0448913918449987,
0.849848080196716));
#23392=CARTESIAN_POINT('Ctrl Pts',(-0.195259979386646,-0.000163936101596873,
0.85241303078758));
#23393=CARTESIAN_POINT('',(-0.195431382385093,-1.17372835601258E-5,0.922413030787581));
#23394=CARTESIAN_POINT('Ctrl Pts',(-0.195399931100211,-0.000164091537283115,
0.852413032945658));
#23395=CARTESIAN_POINT('Ctrl Pts',(-0.195387601258696,-0.014846446413594,
0.853248290872073));
#23396=CARTESIAN_POINT('Ctrl Pts',(-0.193716398613149,-0.0294560944962259,
0.854083548798487));
#23397=CARTESIAN_POINT('Ctrl Pts',(-0.190458429453141,-0.0436663102430562,
0.854918806724902));
#23398=CARTESIAN_POINT('Ctrl Pts',(-0.189269949741117,-0.0488500772737278,
0.85522350178219));
#23399=CARTESIAN_POINT('Ctrl Pts',(-0.187870778448972,-0.0539808948332623,
0.855528196839478));
#23400=CARTESIAN_POINT('Ctrl Pts',(-0.186265973958097,-0.0590436020703462,
0.855832891896766));
#23401=CARTESIAN_POINT('Ctrl Pts',(-0.182597858210626,-0.0706154765552344,
0.856529336070601));
#23402=CARTESIAN_POINT('Ctrl Pts',(-0.177834270151388,-0.0818851793211283,
0.857225780244437));
#23403=CARTESIAN_POINT('Ctrl Pts',(-0.172046446622527,-0.0926346598448002,
0.857922224418272));
#23404=CARTESIAN_POINT('Ctrl Pts',(-0.166270770625217,-0.103361579270478,
0.858617206889356));
#23405=CARTESIAN_POINT('Ctrl Pts',(-0.159475471208498,-0.113569644927268,
0.859312189360441));
#23406=CARTESIAN_POINT('Ctrl Pts',(-0.151779343759101,-0.123061735759158,
0.860007171831525));
#23407=CARTESIAN_POINT('Ctrl Pts',(-0.144084300726887,-0.132552489114963,
0.860702056376615));
#23408=CARTESIAN_POINT('Ctrl Pts',(-0.135489196498889,-0.14132675972071,
0.861396940921705));
#23409=CARTESIAN_POINT('Ctrl Pts',(-0.126154591561029,-0.149218561271948,
0.862091825466795));
#23410=CARTESIAN_POINT('Ctrl Pts',(-0.11682054151243,-0.157109893700393,
0.862786668704944));
#23411=CARTESIAN_POINT('Ctrl Pts',(-0.106747764067875,-0.164118316227588,
0.863481511943094));
#23412=CARTESIAN_POINT('Ctrl Pts',(-0.0961295716375537,-0.170118386592339,
0.864176355181243));
#23413=CARTESIAN_POINT('Ctrl Pts',(-0.0854869069367005,-0.176132285614475,
0.864872799858791));
#23414=CARTESIAN_POINT('Ctrl Pts',(-0.0742971116057915,-0.181132818848136,
0.865569244536339));
#23415=CARTESIAN_POINT('Ctrl Pts',(-0.0627765628032877,-0.185041247192632,
0.866265689213887));
#23416=CARTESIAN_POINT('Ctrl Pts',(-0.0590164931260377,-0.18631687764703,
0.866492994402105));
#23417=CARTESIAN_POINT('Ctrl Pts',(-0.0552213102693736,-0.187476570738043,
0.866720299590323));
#23418=CARTESIAN_POINT('Ctrl Pts',(-0.0513988075906684,-0.188518759221085,
0.866947604778542));
#23419=CARTESIAN_POINT('Ctrl Pts',(-0.0396869776015631,-0.191711937972271,
0.867644048952377));
#23420=CARTESIAN_POINT('Ctrl Pts',(-0.0276349858024966,-0.193820839417297,
0.868340493126212));
#23421=CARTESIAN_POINT('Ctrl Pts',(-0.0154646684568284,-0.19478707356886,
0.869036937300047));
#23422=CARTESIAN_POINT('Ctrl Pts',(-0.00331989427314309,-0.195751279780251,
0.869731919771132));
#23423=CARTESIAN_POINT('Ctrl Pts',(0.00894185425223248,-0.195577435837087,
0.870426902242216));
#23424=CARTESIAN_POINT('Ctrl Pts',(0.0210905360275125,-0.19425846002188,
0.8711218847133));
#23425=CARTESIAN_POINT('Ctrl Pts',(0.033237506001712,-0.19293967005599,
0.87181676925839));
#23426=CARTESIAN_POINT('Ctrl Pts',(0.045270566630233,-0.190476117080456,
0.872511653803479));
#23427=CARTESIAN_POINT('Ctrl Pts',(0.0569631881244799,-0.186912694054457,
0.873206538348569));
#23428=CARTESIAN_POINT('Ctrl Pts',(0.0686551145587711,-0.183349482853724,
0.873901381586718));
#23429=CARTESIAN_POINT('Ctrl Pts',(0.0800058121102576,-0.178686812281845,
0.874596224824868));
#23430=CARTESIAN_POINT('Ctrl Pts',(0.0908050556088387,-0.173019079514011,
0.875291068063017));
#23431=CARTESIAN_POINT('Ctrl Pts',(0.101629188655255,-0.167338284043603,
0.875987512740565));
#23432=CARTESIAN_POINT('Ctrl Pts',(0.111898585544175,-0.160648266128358,
0.876683957418112));
#23433=CARTESIAN_POINT('Ctrl Pts',(0.121429753732272,-0.153088127915002,
0.87738040209566));
#23434=CARTESIAN_POINT('Ctrl Pts',(0.12454053058044,-0.150620654625375,
0.877607707283879));
#23435=CARTESIAN_POINT('Ctrl Pts',(0.127572937694772,-0.1480608093031,0.877835012472099));
#23436=CARTESIAN_POINT('Ctrl Pts',(0.130521432134136,-0.145414290060001,
0.878062317660318));
#23437=CARTESIAN_POINT('Ctrl Pts',(0.13955537363792,-0.137305575418522,
0.878758761834154));
#23438=CARTESIAN_POINT('Ctrl Pts',(0.147862765089638,-0.128323080280893,
0.879455206007989));
#23439=CARTESIAN_POINT('Ctrl Pts',(0.155274250962847,-0.118621528349313,
0.880151650181824));
#23440=CARTESIAN_POINT('Ctrl Pts',(0.162670181548645,-0.108940338114593,
0.880846632652908));
#23441=CARTESIAN_POINT('Ctrl Pts',(0.169173353157778,-0.0985437301274514,
0.881541615123992));
#23442=CARTESIAN_POINT('Ctrl Pts',(0.174653070267297,-0.0876211449720145,
0.882236597595076));
#23443=CARTESIAN_POINT('Ctrl Pts',(0.180132015261302,-0.0767000988554146,
0.882931482140165));
#23444=CARTESIAN_POINT('Ctrl Pts',(0.18458735875612,-0.0652539835451398,
0.883626366685255));
#23445=CARTESIAN_POINT('Ctrl Pts',(0.18793397850948,-0.053497473973997,
0.884321251230345));
#23446=CARTESIAN_POINT('Ctrl Pts',(0.191280399325297,-0.0417416632605951,
0.885016094468493));
#23447=CARTESIAN_POINT('Ctrl Pts',(0.19351801319233,-0.0296763445350412,
0.885710937706643));
#23448=CARTESIAN_POINT('Ctrl Pts',(0.194612132955479,-0.0175293384506979,
0.886405780944792));
#23449=CARTESIAN_POINT('Ctrl Pts',(0.195708774390279,-0.00535433656377403,
0.887102225622339));
#23450=CARTESIAN_POINT('Ctrl Pts',(0.195656646472601,0.00690185105100441,
0.887798670299887));
#23451=CARTESIAN_POINT('Ctrl Pts',(0.194473119647808,0.0190096221543002,
0.888495114977434));
#23452=CARTESIAN_POINT('Ctrl Pts',(0.194086840886055,0.022961349087221,
0.888722420165654));
#23453=CARTESIAN_POINT('Ctrl Pts',(0.193580453103342,0.0268973206819572,
0.888949725353874));
#23454=CARTESIAN_POINT('Ctrl Pts',(0.192955738064007,0.0308097898106166,
0.889177030542093));
#23455=CARTESIAN_POINT('Ctrl Pts',(0.191041663190223,0.0427972695127193,
0.889873474715929));
#23456=CARTESIAN_POINT('Ctrl Pts',(0.187999447141525,0.0546481299516366,
0.890569918889764));
#23457=CARTESIAN_POINT('Ctrl Pts',(0.183867251760222,0.0661361756540484,
0.891266363063599));
#23458=CARTESIAN_POINT('Ctrl Pts',(0.179743729064517,0.0776001101518047,
0.891961345534684));
#23459=CARTESIAN_POINT('Ctrl Pts',(0.174534990886009,0.0887019003319478,
0.892656328005768));
#23460=CARTESIAN_POINT('Ctrl Pts',(0.168329332575936,0.0992290068202845,
0.893351310476852));
#23461=CARTESIAN_POINT('Ctrl Pts',(0.162124548669588,0.109754629994414,
0.894046195021942));
#23462=CARTESIAN_POINT('Ctrl Pts',(0.15492352779897,0.11970495359588,0.894741079567032));
#23463=CARTESIAN_POINT('Ctrl Pts',(0.146860480482702,0.128892045031453,
0.895435964112122));
#23464=CARTESIAN_POINT('Ctrl Pts',(0.138797912468814,0.138078590346605,
0.896130807350271));
#23465=CARTESIAN_POINT('Ctrl Pts',(0.129874017515357,0.146501352994742,
0.89682565058842));
#23466=CARTESIAN_POINT('Ctrl Pts',(0.120261400861954,0.154007647416355,
0.897520493826569));
#23467=CARTESIAN_POINT('Ctrl Pts',(0.110626629537989,0.161531241964047,
0.898216938504117));
#23468=CARTESIAN_POINT('Ctrl Pts',(0.100300697351395,0.168133663992845,
0.898913383181665));
#23469=CARTESIAN_POINT('Ctrl Pts',(0.0894859359502034,0.173705000696917,
0.899609827859213));
#23470=CARTESIAN_POINT('Ctrl Pts',(0.0859562207336297,0.175523370165416,
0.899837133047432));
#23471=CARTESIAN_POINT('Ctrl Pts',(0.0823746110938788,0.177232280159951,
0.900064438235651));
#23472=CARTESIAN_POINT('Ctrl Pts',(0.0787485823833833,0.178829026650059,
0.900291743423871));
#23473=CARTESIAN_POINT('Ctrl Pts',(0.0676387322767088,0.183721324968634,
0.900988187597706));
#23474=CARTESIAN_POINT('Ctrl Pts',(0.056031907477925,0.187591672462066,
0.901684631771541));
#23475=CARTESIAN_POINT('Ctrl Pts',(0.0441388519136026,0.190349472685766,
0.902381075945376));
#23476=CARTESIAN_POINT('Ctrl Pts',(0.0322707575919605,0.193101484815709,
0.90307605841646));
#23477=CARTESIAN_POINT('Ctrl Pts',(0.0201184525329993,0.194745315819805,
0.903771040887544));
#23478=CARTESIAN_POINT('Ctrl Pts',(0.00790839292281639,0.195239896848411,
0.904466023358628));
#23479=CARTESIAN_POINT('Ctrl Pts',(-0.00429994623788739,0.195734408188442,
0.905160907903718));
#23480=CARTESIAN_POINT('Ctrl Pts',(-0.0165651520216134,0.195079909574438,
0.905855792448807));
#23481=CARTESIAN_POINT('Ctrl Pts',(-0.0286565442593787,0.193287253773006,
0.906550676993897));
#23482=CARTESIAN_POINT('Ctrl Pts',(-0.040747217732531,0.191494704534782,
0.907245520232046));
#23483=CARTESIAN_POINT('Ctrl Pts',(-0.0526632358035508,0.188564287312229,
0.907940363470195));
#23484=CARTESIAN_POINT('Ctrl Pts',(-0.0641827124220688,0.18455822773896,
0.908635206708344));
#23485=CARTESIAN_POINT('Ctrl Pts',(-0.0757287385451317,0.180542935203087,
0.909331651385891));
#23486=CARTESIAN_POINT('Ctrl Pts',(-0.0868755933593291,0.175447399910341,
0.910028096063439));
#23487=CARTESIAN_POINT('Ctrl Pts',(-0.0974212086587235,0.169382018241233,
0.910724540740986));
#23488=CARTESIAN_POINT('Ctrl Pts',(-0.100863080135097,0.167402402678979,
0.910951845929206));
#23489=CARTESIAN_POINT('Ctrl Pts',(-0.104241124651882,0.165319828256848,
0.911179151117426));
#23490=CARTESIAN_POINT('Ctrl Pts',(-0.107549016585019,0.163139109448333,
0.911406456305646));
#23491=CARTESIAN_POINT('Ctrl Pts',(-0.117666821493063,0.156468973933073,
0.91210171165119));
#23492=CARTESIAN_POINT('Ctrl Pts',(-0.127198156063682,0.14882995897731,
0.912796966996734));
#23493=CARTESIAN_POINT('Ctrl Pts',(-0.135952990562336,0.140349365360722,
0.913492222342278));
#23494=CARTESIAN_POINT('Ctrl Pts',(-0.14468945725879,0.131886564183969,
0.914186019029447));
#23495=CARTESIAN_POINT('Ctrl Pts',(-0.152651979732653,0.122586239953042,
0.914879815716616));
#23496=CARTESIAN_POINT('Ctrl Pts',(-0.159683572942223,0.112615791665316,
0.915573612403784));
#23497=CARTESIAN_POINT('Ctrl Pts',(-0.166714187837885,0.102646730577892,
0.916267312562197));
#23498=CARTESIAN_POINT('Ctrl Pts',(-0.172813587453725,0.0920084215366531,
0.916961012720609));
#23499=CARTESIAN_POINT('Ctrl Pts',(-0.177866113483614,0.0808999732647313,
0.917654712879021));
#23500=CARTESIAN_POINT('Ctrl Pts',(-0.182918437048923,0.0697919701300136,
0.918348385239514));
#23501=CARTESIAN_POINT('Ctrl Pts',(-0.186923632136932,0.0582146770278337,
0.919042057600007));
#23502=CARTESIAN_POINT('Ctrl Pts',(-0.189813979213258,0.0463876416217614,
0.9197357299605));
#23503=CARTESIAN_POINT('Ctrl Pts',(-0.192710927053388,0.0345335964950021,
0.920430986479327));
#23504=CARTESIAN_POINT('Ctrl Pts',(-0.194487802582643,0.0224295396783319,
0.921126242998154));
#23505=CARTESIAN_POINT('Ctrl Pts',(-0.195128111370912,0.0103043754211897,
0.921821499516981));
#23506=CARTESIAN_POINT('Ctrl Pts',(-0.195309705099675,0.00686563800316279,
0.922018676607181));
#23507=CARTESIAN_POINT('Ctrl Pts',(-0.195400206064584,0.00342520612777168,
0.922215853697381));
#23508=CARTESIAN_POINT('Ctrl Pts',(-0.195399999647596,-1.17353987651412E-5,
0.922413030787581));
#23509=CARTESIAN_POINT('',(-0.195294337528581,0.000171262189333537,0.99241303078758));
#23510=CARTESIAN_POINT('Ctrl Pts',(-0.195719607651052,-1.17545938899131E-5,
0.922413030787581));
#23511=CARTESIAN_POINT('Ctrl Pts',(-0.195720155584114,-0.000641092913902824,
0.922449076920861));
#23512=CARTESIAN_POINT('Ctrl Pts',(-0.195717382600782,-0.00127042626739718,
0.922485123054142));
#23513=CARTESIAN_POINT('Ctrl Pts',(-0.195083429571586,-0.0665807256656151,
0.926226073481348));
#23514=CARTESIAN_POINT('Ctrl Pts',(-0.123353837031904,-0.19525864748591,
0.933635882069198));
#23515=CARTESIAN_POINT('Ctrl Pts',(0.0971649057626222,-0.209525868609732,
0.944750594950976));
#23516=CARTESIAN_POINT('Ctrl Pts',(0.228733969509715,-0.0319824908481484,
0.955865307832749));
#23517=CARTESIAN_POINT('Ctrl Pts',(0.150908365342008,0.174839279906791,
0.966980020714528));
#23518=CARTESIAN_POINT('Ctrl Pts',(-0.0650664044878207,0.2216043129895,
0.978094733596303));
#23519=CARTESIAN_POINT('Ctrl Pts',(-0.184366805427636,0.102537997645834,
0.986572403620654));
#23520=CARTESIAN_POINT('Ctrl Pts',(-0.195452091727079,0.0189207190229355,
0.99134516935108));
#23521=CARTESIAN_POINT('Ctrl Pts',(-0.195294337528581,0.000171262189333537,
0.99241303078758));
#23522=CARTESIAN_POINT('',(-0.195387463526517,-8.85805956595877E-5,1.06241303507908));
#23523=CARTESIAN_POINT('Ctrl Pts',(-0.195294337528581,0.000171262189333537,
0.99241303078758));
#23524=CARTESIAN_POINT('Ctrl Pts',(-0.194904769586374,-0.0461298022874415,
0.995050073645006));
#23525=CARTESIAN_POINT('Ctrl Pts',(-0.155279374437814,-0.158080892225847,
1.00139202079636));
#23526=CARTESIAN_POINT('Ctrl Pts',(0.0315331778821316,-0.228796344422667,
1.01143887224164));
#23527=CARTESIAN_POINT('Ctrl Pts',(0.209334625055623,-0.0975762434270945,
1.0225535851234));
#23528=CARTESIAN_POINT('Ctrl Pts',(0.19550054738536,0.122970095960548,1.03366829800519));
#23529=CARTESIAN_POINT('Ctrl Pts',(0.0026953606810326,0.230943377387883,
1.04478301088697));
#23530=CARTESIAN_POINT('Ctrl Pts',(-0.165641881126728,0.141768188472822,
1.05436458848109));
#23531=CARTESIAN_POINT('Ctrl Pts',(-0.194962120753271,0.0381301666874187,
1.0602412617813));
#23532=CARTESIAN_POINT('Ctrl Pts',(-0.195118116536412,-8.83829588442778E-5,
1.06241303078758));
#23533=CARTESIAN_POINT('',(-0.195399960265364,-0.000124612576654666,1.13241303078758));
#23534=CARTESIAN_POINT('Ctrl Pts',(-0.195399979917734,-8.85897797224884E-5,
1.0624130352785));
#23535=CARTESIAN_POINT('Ctrl Pts',(-0.195393855063461,-0.01359800819892,
1.06317960217384));
#23536=CARTESIAN_POINT('Ctrl Pts',(-0.193982436345336,-0.0270604850983458,
1.06394616906917));
#23537=CARTESIAN_POINT('Ctrl Pts',(-0.191219944617096,-0.0402006564701958,
1.06471273596451));
#23538=CARTESIAN_POINT('Ctrl Pts',(-0.188457452888856,-0.0533408278420449,
1.06547930285984));
#23539=CARTESIAN_POINT('Ctrl Pts',(-0.184344210097986,-0.066158178502653,
1.06624586975518));
#23540=CARTESIAN_POINT('Ctrl Pts',(-0.178983350055113,-0.0783971963978877,
1.06701243665052));
#23541=CARTESIAN_POINT('Ctrl Pts',(-0.174112881781141,-0.0895166339296635,
1.06770888082435));
#23542=CARTESIAN_POINT('Ctrl Pts',(-0.168185008300444,-0.100219824464572,
1.06840532499819));
#23543=CARTESIAN_POINT('Ctrl Pts',(-0.161293610699711,-0.110297466641124,
1.06910176917202));
#23544=CARTESIAN_POINT('Ctrl Pts',(-0.154416676820853,-0.120353957779523,
1.06979675164311));
#23545=CARTESIAN_POINT('Ctrl Pts',(-0.146580660429029,-0.129786748762222,
1.07049173411419));
#23546=CARTESIAN_POINT('Ctrl Pts',(-0.137924523062689,-0.13841237639001,
1.07118671658528));
#23547=CARTESIAN_POINT('Ctrl Pts',(-0.129269605383025,-0.147036788630075,
1.07188160113037));
#23548=CARTESIAN_POINT('Ctrl Pts',(-0.119795382948273,-0.154853613472036,
1.07257648567545));
#23549=CARTESIAN_POINT('Ctrl Pts',(-0.109679058270219,-0.161714761778132,
1.07327137022054));
#23550=CARTESIAN_POINT('Ctrl Pts',(-0.0995633349502271,-0.168575502227918,
1.07396621345869));
#23551=CARTESIAN_POINT('Ctrl Pts',(-0.0888063249583923,-0.174480209485929,
1.07466105669684));
#23552=CARTESIAN_POINT('Ctrl Pts',(-0.0776135147199785,-0.179324572585052,
1.07535589993499));
#23553=CARTESIAN_POINT('Ctrl Pts',(-0.0663949078610987,-0.184180100726163,
1.07605234461253));
#23554=CARTESIAN_POINT('Ctrl Pts',(-0.0547393245482148,-0.187970117850791,
1.07674878929008));
#23555=CARTESIAN_POINT('Ctrl Pts',(-0.0428702513051903,-0.19063919206981,
1.07744523396763));
#23556=CARTESIAN_POINT('Ctrl Pts',(-0.0389964304340447,-0.19151032288218,
1.07767253915585));
#23557=CARTESIAN_POINT('Ctrl Pts',(-0.035099945031278,-0.19226245484328,
1.07789984434406));
#23558=CARTESIAN_POINT('Ctrl Pts',(-0.0311887104378679,-0.192894853070845,
1.07812714953228));
#23559=CARTESIAN_POINT('Ctrl Pts',(-0.0192050132489323,-0.194832468593762,
1.07882359370612));
#23560=CARTESIAN_POINT('Ctrl Pts',(-0.00699764327111413,-0.195655930708425,
1.07952003787995));
#23561=CARTESIAN_POINT('Ctrl Pts',(0.0052066348891197,-0.195330619599517,
1.08021648205379));
#23562=CARTESIAN_POINT('Ctrl Pts',(0.0173852986101341,-0.195005991256236,
1.08091146452487));
#23563=CARTESIAN_POINT('Ctrl Pts',(0.0295600148048395,-0.193537323766802,
1.08160644699596));
#23564=CARTESIAN_POINT('Ctrl Pts',(0.0415012821371695,-0.190941885349891,
1.08230142946704));
#23565=CARTESIAN_POINT('Ctrl Pts',(0.0534408668939978,-0.188346812641325,
1.08299631401213));
#23566=CARTESIAN_POINT('Ctrl Pts',(0.0651462038917023,-0.184625424846013,
1.08369119855722));
#23567=CARTESIAN_POINT('Ctrl Pts',(0.0763967760151574,-0.179846302754574,
1.08438608310231));
#23568=CARTESIAN_POINT('Ctrl Pts',(0.0876466793559811,-0.175067464754807,
1.08508092634046));
#23569=CARTESIAN_POINT('Ctrl Pts',(0.0984410758960655,-0.169231384297636,
1.08577576957861));
#23570=CARTESIAN_POINT('Ctrl Pts',(0.10858089334579,-0.162454146146629,
1.08647061281676));
#23571=CARTESIAN_POINT('Ctrl Pts',(0.118744080531691,-0.1556612881614,1.08716705749431));
#23572=CARTESIAN_POINT('Ctrl Pts',(0.128248985254343,-0.147923482375403,
1.08786350217186));
#23573=CARTESIAN_POINT('Ctrl Pts',(0.136927842490727,-0.13939844314351,
1.08855994684941));
#23574=CARTESIAN_POINT('Ctrl Pts',(0.139760442611373,-0.136616046049164,
1.08878725203763));
#23575=CARTESIAN_POINT('Ctrl Pts',(0.142505350145887,-0.133750076124693,
1.08901455722585));
#23576=CARTESIAN_POINT('Ctrl Pts',(0.145157655356412,-0.130806785341698,
1.08924186241407));
#23577=CARTESIAN_POINT('Ctrl Pts',(0.153284097720414,-0.121788787407829,
1.0899383065879));
#23578=CARTESIAN_POINT('Ctrl Pts',(0.160595719048788,-0.111978682149472,
1.09063475076174));
#23579=CARTESIAN_POINT('Ctrl Pts',(0.166940463028469,-0.101548224030952,
1.09133119493557));
#23580=CARTESIAN_POINT('Ctrl Pts',(0.173271890607384,-0.0911396574435826,
1.09202617740665));
#23581=CARTESIAN_POINT('Ctrl Pts',(0.17863995438636,-0.0801140241338391,
1.09272115987774));
#23582=CARTESIAN_POINT('Ctrl Pts',(0.182934710385865,-0.0686735155357568,
1.09341614234882));
#23583=CARTESIAN_POINT('Ctrl Pts',(0.187228861235931,-0.0572346189541328,
1.09411102689391));
#23584=CARTESIAN_POINT('Ctrl Pts',(0.190449654083029,-0.0453817655091186,
1.094805911439));
#23585=CARTESIAN_POINT('Ctrl Pts',(0.192535129751674,-0.0333374235883074,
1.09550079598409));
#23586=CARTESIAN_POINT('Ctrl Pts',(0.194620481450631,-0.0212937976352359,
1.09619563922224));
#23587=CARTESIAN_POINT('Ctrl Pts',(0.195570526886726,-0.00905957328563089,
1.09689048246039));
#23588=CARTESIAN_POINT('Ctrl Pts',(0.195374848768871,0.00313503884199943,
1.09758532569853));
#23589=CARTESIAN_POINT('Ctrl Pts',(0.19517871966203,0.0153577564922006,
1.09828177037608));
#23590=CARTESIAN_POINT('Ctrl Pts',(0.193831674303266,0.0275398056207277,
1.09897821505363));
#23591=CARTESIAN_POINT('Ctrl Pts',(0.191375249774799,0.0394547053421153,
1.09967465973118));
#23592=CARTESIAN_POINT('Ctrl Pts',(0.190573523438463,0.0433434830312887,
1.0999019649194));
#23593=CARTESIAN_POINT('Ctrl Pts',(0.189654025635844,0.0472039007252778,
1.10012927010761));
#23594=CARTESIAN_POINT('Ctrl Pts',(0.188619346855062,0.0510284429702684,
1.10035657529583));
#23595=CARTESIAN_POINT('Ctrl Pts',(0.185449177206451,0.0627465220205966,
1.10105301946967));
#23596=CARTESIAN_POINT('Ctrl Pts',(0.181171621168803,0.0742095271228536,
1.1017494636435));
#23597=CARTESIAN_POINT('Ctrl Pts',(0.17584853077764,0.085196562274222,1.10244590781734));
#23598=CARTESIAN_POINT('Ctrl Pts',(0.170536612532301,0.0961605377459927,
1.10314089028842));
#23599=CARTESIAN_POINT('Ctrl Pts',(0.164183826259085,0.106649713365788,
1.10383587275951));
#23600=CARTESIAN_POINT('Ctrl Pts',(0.156900433625811,0.116462070769983,
1.10453085523059));
#23601=CARTESIAN_POINT('Ctrl Pts',(0.149618067253625,0.126273045571166,
1.10522573977568));
#23602=CARTESIAN_POINT('Ctrl Pts',(0.141405838948271,0.135406661920326,
1.10592062432077));
#23603=CARTESIAN_POINT('Ctrl Pts',(0.132417068043232,0.143690222669582,
1.10661550886586));
#23604=CARTESIAN_POINT('Ctrl Pts',(0.123428831469583,0.151973291008187,
1.10731035210401));
#23605=CARTESIAN_POINT('Ctrl Pts',(0.113664806061235,0.15940583025075,1.10800519534216));
#23606=CARTESIAN_POINT('Ctrl Pts',(0.103312766041843,0.165854250391069,
1.10870003858031));
#23607=CARTESIAN_POINT('Ctrl Pts',(0.0929368671664764,0.172317532522561,
1.10939648325786));
#23608=CARTESIAN_POINT('Ctrl Pts',(0.0819710253158985,0.177791759835756,
1.11009292793541));
#23609=CARTESIAN_POINT('Ctrl Pts',(0.0706280545274067,0.18218901699519,
1.11078937261296));
#23610=CARTESIAN_POINT('Ctrl Pts',(0.0669259426538131,0.183624191099465,
1.11101667780118));
#23611=CARTESIAN_POINT('Ctrl Pts',(0.0631837944026711,0.18494503456012,
1.1112439829894));
#23612=CARTESIAN_POINT('Ctrl Pts',(0.0594093290239704,0.186149648468434,
1.11147128817762));
#23613=CARTESIAN_POINT('Ctrl Pts',(0.0478446813230984,0.189840485200924,
1.11216773235145));
#23614=CARTESIAN_POINT('Ctrl Pts',(0.0358938395025882,0.19246257433198,
1.11286417652529));
#23615=CARTESIAN_POINT('Ctrl Pts',(0.0237759414585748,0.193948097716266,
1.11356062069913));
#23616=CARTESIAN_POINT('Ctrl Pts',(0.0116834765584835,0.195430503271876,
1.11425560317021));
#23617=CARTESIAN_POINT('Ctrl Pts',(-0.000574497253568146,0.195780898248486,
1.1149505856413));
#23618=CARTESIAN_POINT('Ctrl Pts',(-0.0127684517811844,0.194982375201226,
1.11564556811238));
#23619=CARTESIAN_POINT('Ctrl Pts',(-0.0249606881285953,0.194183964669268,
1.11634045265747));
#23620=CARTESIAN_POINT('Ctrl Pts',(-0.0370880476003977,0.192236968625343,
1.11703533720257));
#23621=CARTESIAN_POINT('Ctrl Pts',(-0.0489222886422267,0.189176556882735,
1.11773022174766));
#23622=CARTESIAN_POINT('Ctrl Pts',(-0.0607558262056203,0.186116327064228,
1.11842506498581));
#23623=CARTESIAN_POINT('Ctrl Pts',(-0.072295438759328,0.181943058096389,
1.11911990822396));
#23624=CARTESIAN_POINT('Ctrl Pts',(-0.0833270586056728,0.176742075647331,
1.11981475146211));
#23625=CARTESIAN_POINT('Ctrl Pts',(-0.0943841035690545,0.171529106238124,
1.12051119613965));
#23626=CARTESIAN_POINT('Ctrl Pts',(-0.104930054533146,0.16528412661991,
1.1212076408172));
#23627=CARTESIAN_POINT('Ctrl Pts',(-0.11477564126072,0.158138269160854,
1.12190408549475));
#23628=CARTESIAN_POINT('Ctrl Pts',(-0.117989037839574,0.155806008570674,
1.12213139068297));
#23629=CARTESIAN_POINT('Ctrl Pts',(-0.121128084378196,0.153378110753885,
1.12235869587118));
#23630=CARTESIAN_POINT('Ctrl Pts',(-0.124186999457379,0.150860031704136,
1.1225860010594));
#23631=CARTESIAN_POINT('Ctrl Pts',(-0.133433078336889,0.1432487195506,1.12327306874371));
#23632=CARTESIAN_POINT('Ctrl Pts',(-0.142013719396526,0.134753546717402,
1.12396013642802));
#23633=CARTESIAN_POINT('Ctrl Pts',(-0.149755525370193,0.125516702558255,
1.12464720411233));
#23634=CARTESIAN_POINT('Ctrl Pts',(-0.157486281429236,0.116293042188485,
1.12533329114183));
#23635=CARTESIAN_POINT('Ctrl Pts',(-0.164379931087259,0.106330434043949,
1.12601937817133));
#23636=CARTESIAN_POINT('Ctrl Pts',(-0.17029965108117,0.0958080833835636,
1.12670546520084));
#23637=CARTESIAN_POINT('Ctrl Pts',(-0.176213704663528,0.0852958048160153,
1.12739089550139));
#23638=CARTESIAN_POINT('Ctrl Pts',(-0.181155218960983,0.0742256220721924,
1.12807632580195));
#23639=CARTESIAN_POINT('Ctrl Pts',(-0.185032122360298,0.0628034528895012,
1.12876175610251));
#23640=CARTESIAN_POINT('Ctrl Pts',(-0.188916347707919,0.0513597117139882,
1.12944848091178));
#23641=CARTESIAN_POINT('Ctrl Pts',(-0.191731670618013,0.0395635195003829,
1.13013520572105));
#23642=CARTESIAN_POINT('Ctrl Pts',(-0.19343566509094,0.0276369946055204,
1.13082193053031));
#23643=CARTESIAN_POINT('Ctrl Pts',(-0.194751682806556,0.0184259799592059,
1.13135229728274));
#23644=CARTESIAN_POINT('Ctrl Pts',(-0.195405867097655,0.0091376531278688,
1.13188266403516));
#23645=CARTESIAN_POINT('Ctrl Pts',(-0.195399960265364,-0.000124612576654666,
1.13241303078758));
#23646=CARTESIAN_POINT('',(-0.195499582979996,0.000166550639662629,1.20241303078758));
#23647=CARTESIAN_POINT('Ctrl Pts',(-0.195617452784838,-0.000124751278337231,
1.13241303078758));
#23648=CARTESIAN_POINT('Ctrl Pts',(-0.195673257048185,-0.00762911832956361,
1.13284225850544));
#23649=CARTESIAN_POINT('Ctrl Pts',(-0.191874449616845,-0.0798508440029845,
1.13697639051729));
#23650=CARTESIAN_POINT('Ctrl Pts',(-0.102028562826224,-0.207201063935842,
1.14481542682289));
#23651=CARTESIAN_POINT('Ctrl Pts',(0.118763095185579,-0.198084415718343,
1.15593013970476));
#23652=CARTESIAN_POINT('Ctrl Pts',(0.230832996956899,-0.00763125444448434,
1.16704485258647));
#23653=CARTESIAN_POINT('Ctrl Pts',(0.131586674709796,0.189807943899515,
1.17815956546829));
#23654=CARTESIAN_POINT('Ctrl Pts',(-0.0881207583724611,0.213487330941126,
1.18927427835005));
#23655=CARTESIAN_POINT('Ctrl Pts',(-0.18925201110573,0.08855622028932,1.19735876678982));
#23656=CARTESIAN_POINT('Ctrl Pts',(-0.195606518663776,0.011980768958621,
1.20173835093566));
#23657=CARTESIAN_POINT('Ctrl Pts',(-0.195499582979996,0.000166550639662629,
1.20241303078758));
#23658=CARTESIAN_POINT('',(-0.195369097555756,2.13661978956508E-5,1.27241302913566));
#23659=CARTESIAN_POINT('Ctrl Pts',(-0.195499582979996,0.000166550639662629,
1.20241303078758));
#23660=CARTESIAN_POINT('Ctrl Pts',(-0.195019297224031,-0.0528952578782005,
1.20544325522959));
#23661=CARTESIAN_POINT('Ctrl Pts',(-0.145266592861051,-0.171625975326032,
1.21217838396553));
#23662=CARTESIAN_POINT('Ctrl Pts',(0.0555353437883074,-0.224182814057769,
1.22261841699537));
#23663=CARTESIAN_POINT('Ctrl Pts',(0.218474097288274,-0.0749077922687062,
1.23373312987716));
#23664=CARTESIAN_POINT('Ctrl Pts',(0.181410589874887,0.142941618886128,
1.24484784275894));
#23665=CARTESIAN_POINT('Ctrl Pts',(-0.0217253653892236,0.229935027838755,
1.2559625556407));
#23666=CARTESIAN_POINT('Ctrl Pts',(-0.173213681772595,0.127838529215634,
1.26515094597265));
#23667=CARTESIAN_POINT('Ctrl Pts',(-0.195111799500146,0.0313356137564543,
1.27063443201065));
#23668=CARTESIAN_POINT('Ctrl Pts',(-0.195081377439699,2.16055737428584E-5,
1.27241301375474));
#23669=CARTESIAN_POINT('',(-0.195399919414568,-0.000177462052753457,1.34241303078758));
#23670=CARTESIAN_POINT('Ctrl Pts',(-0.195399998834656,2.13404888144855E-5,
1.27241303078758));
#23671=CARTESIAN_POINT('Ctrl Pts',(-0.195401390143229,-0.0127179034900279,
1.27313541813527));
#23672=CARTESIAN_POINT('Ctrl Pts',(-0.194152666432573,-0.0254370179035737,
1.27385780548296));
#23673=CARTESIAN_POINT('Ctrl Pts',(-0.191691147325218,-0.0378901575233157,
1.27458019283064));
#23674=CARTESIAN_POINT('Ctrl Pts',(-0.189219297789346,-0.0503955601006223,
1.27530561187158));
#23675=CARTESIAN_POINT('Ctrl Pts',(-0.185524695317359,-0.0626320086384815,
1.27603103091251));
#23676=CARTESIAN_POINT('Ctrl Pts',(-0.180695285645632,-0.0743664826749485,
1.27675644995344));
#23677=CARTESIAN_POINT('Ctrl Pts',(-0.177509646687822,-0.0821069313386492,
1.27723496043705));
#23678=CARTESIAN_POINT('Ctrl Pts',(-0.173831273018624,-0.0896293197676277,
1.27771347092065));
#23679=CARTESIAN_POINT('Ctrl Pts',(-0.16969625686245,-0.096872805300937,
1.27819198140425));
#23680=CARTESIAN_POINT('Ctrl Pts',(-0.163677981381863,-0.107415277139654,
1.27888842557809));
#23681=CARTESIAN_POINT('Ctrl Pts',(-0.15665220988582,-0.117432088334572,
1.27958486975192));
#23682=CARTESIAN_POINT('Ctrl Pts',(-0.148734416313031,-0.126725030692527,
1.28028131392576));
#23683=CARTESIAN_POINT('Ctrl Pts',(-0.140833240670413,-0.135998468946749,
1.28097629639684));
#23684=CARTESIAN_POINT('Ctrl Pts',(-0.132044264372559,-0.144550345597606,
1.28167127886792));
#23685=CARTESIAN_POINT('Ctrl Pts',(-0.122525058852388,-0.152212909942682,
1.28236626133901));
#23686=CARTESIAN_POINT('Ctrl Pts',(-0.113007194628873,-0.159874394599761,
1.2830611458841));
#23687=CARTESIAN_POINT('Ctrl Pts',(-0.102759957644003,-0.166646231538767,
1.28375603042919));
#23688=CARTESIAN_POINT('Ctrl Pts',(-0.0919752079100879,-0.172399887267643,
1.28445091497428));
#23689=CARTESIAN_POINT('Ctrl Pts',(-0.0811910992683102,-0.178153200974355,
1.28514575821242));
#23690=CARTESIAN_POINT('Ctrl Pts',(-0.0698703265727585,-0.182888065000111,
1.28584060145057));
#23691=CARTESIAN_POINT('Ctrl Pts',(-0.0582282489813947,-0.186522467870658,
1.28653544468872));
#23692=CARTESIAN_POINT('Ctrl Pts',(-0.0465593393209889,-0.190165247128322,
1.28723188936627));
#23693=CARTESIAN_POINT('Ctrl Pts',(-0.0345685011667856,-0.19270230300626,
1.28792833404382));
#23694=CARTESIAN_POINT('Ctrl Pts',(-0.022483827539076,-0.194102131619395,
1.28862477872137));
#23695=CARTESIAN_POINT('Ctrl Pts',(-0.0185396391460514,-0.194559006826641,
1.28885208390959));
#23696=CARTESIAN_POINT('Ctrl Pts',(-0.0145854886936885,-0.194895154385967,
1.28907938909781));
#23697=CARTESIAN_POINT('Ctrl Pts',(-0.0106293248611298,-0.195110680007519,
1.28930669428604));
#23698=CARTESIAN_POINT('Ctrl Pts',(0.00149203177601938,-0.195771032569711,
1.29000313845987));
#23699=CARTESIAN_POINT('Ctrl Pts',(0.0137180672259798,-0.1952998332419,
1.29069958263371));
#23700=CARTESIAN_POINT('Ctrl Pts',(0.0258196281200339,-0.193686620094789,
1.29139602680755));
#23701=CARTESIAN_POINT('Ctrl Pts',(0.0378957901587132,-0.192076792772678,
1.29209100927863));
#23702=CARTESIAN_POINT('Ctrl Pts',(0.0498471270121964,-0.18932974962934,
1.29278599174972));
#23703=CARTESIAN_POINT('Ctrl Pts',(0.0614472473301596,-0.185486915429488,
1.29348097422081));
#23704=CARTESIAN_POINT('Ctrl Pts',(0.0730457331416889,-0.181644622701367,
1.2941758587659));
#23705=CARTESIAN_POINT('Ctrl Pts',(0.0842922561667842,-0.176707076630744,
1.29487074331099));
#23706=CARTESIAN_POINT('Ctrl Pts',(0.0949747815777786,-0.170765777790087,
1.29556562785608));
#23707=CARTESIAN_POINT('Ctrl Pts',(0.105656671973292,-0.16482483212591,
1.29626047109423));
#23708=CARTESIAN_POINT('Ctrl Pts',(0.115773878959235,-0.157880701181627,
1.29695531433238));
#23709=CARTESIAN_POINT('Ctrl Pts',(0.125140712575688,-0.150069857253377,
1.29765015757053));
#23710=CARTESIAN_POINT('Ctrl Pts',(0.134529134394443,-0.142241011288818,
1.29834660224808));
#23711=CARTESIAN_POINT('Ctrl Pts',(0.143163099677314,-0.133542074821454,
1.29904304692563));
#23712=CARTESIAN_POINT('Ctrl Pts',(0.150892449754659,-0.124147608140623,
1.29973949160317));
#23713=CARTESIAN_POINT('Ctrl Pts',(0.153415150308972,-0.121081447846931,
1.29996679679139));
#23714=CARTESIAN_POINT('Ctrl Pts',(0.155841817511163,-0.117941449873993,
1.3001941019796));
#23715=CARTESIAN_POINT('Ctrl Pts',(0.158168229811754,-0.114734350036143,
1.30042140716782));
#23716=CARTESIAN_POINT('Ctrl Pts',(0.165296163430056,-0.104908063119737,
1.30111785134165));
#23717=CARTESIAN_POINT('Ctrl Pts',(0.171530130368159,-0.0943802130142339,
1.30181429551548));
#23718=CARTESIAN_POINT('Ctrl Pts',(0.176737076434546,-0.0833376614344879,
1.30251073968932));
#23719=CARTESIAN_POINT('Ctrl Pts',(0.181933094119773,-0.0723182860526738,
1.3032057221604));
#23720=CARTESIAN_POINT('Ctrl Pts',(0.186105932080036,-0.0607871056285705,
1.30390070463148));
#23721=CARTESIAN_POINT('Ctrl Pts',(0.189167629163193,-0.0489567980649938,
1.30459568710257));
#23722=CARTESIAN_POINT('Ctrl Pts',(0.192228894840173,-0.0371281574422114,
1.30529057164766));
#23723=CARTESIAN_POINT('Ctrl Pts',(0.194179066755089,-0.0250013082696133,
1.30598545619274));
#23724=CARTESIAN_POINT('Ctrl Pts',(0.194980042692081,-0.0128040209229106,
1.30668034073783));
#23725=CARTESIAN_POINT('Ctrl Pts',(0.195780971015601,-0.000607458635683858,
1.30737518397598));
#23726=CARTESIAN_POINT('Ctrl Pts',(0.195432808277455,0.0116586578840071,
1.30807002721413));
#23727=CARTESIAN_POINT('Ctrl Pts',(0.193949523715838,0.0237643062259244,
1.30876487045228));
#23728=CARTESIAN_POINT('Ctrl Pts',(0.192462820555311,0.0358978550511995,
1.30946131512983));
#23729=CARTESIAN_POINT('Ctrl Pts',(0.189835943577989,0.0478693365599423,
1.31015775980737));
#23730=CARTESIAN_POINT('Ctrl Pts',(0.186134131321106,0.059457927623971,
1.31085420448492));
#23731=CARTESIAN_POINT('Ctrl Pts',(0.18492593609909,0.0632402048930077,
1.31108150967314));
#23732=CARTESIAN_POINT('Ctrl Pts',(0.183603625910985,0.0669818351189525,
1.31130881486136));
#23733=CARTESIAN_POINT('Ctrl Pts',(0.182170570957313,0.0706756186890956,
1.31153612004958));
#23734=CARTESIAN_POINT('Ctrl Pts',(0.177779809879307,0.0819930640451269,
1.31223256422342));
#23735=CARTESIAN_POINT('Ctrl Pts',(0.172314819033327,0.0929398373908723,
1.31292900839726));
#23736=CARTESIAN_POINT('Ctrl Pts',(0.16586044795515,0.103302816051243,1.31362545257109));
#23737=CARTESIAN_POINT('Ctrl Pts',(0.159419623363995,0.113644044806901,
1.31432043504218));
#23738=CARTESIAN_POINT('Ctrl Pts',(0.15199393508303,0.123403135551954,1.31501541751326));
#23739=CARTESIAN_POINT('Ctrl Pts',(0.143714376254833,0.132390853376222,
1.31571039998435));
#23740=CARTESIAN_POINT('Ctrl Pts',(0.13543598405179,0.141377304792712,1.31640528452944));
#23741=CARTESIAN_POINT('Ctrl Pts',(0.126304518651016,0.149591924746643,
1.31710016907453));
#23742=CARTESIAN_POINT('Ctrl Pts',(0.116490691147871,0.156879185604373,
1.31779505361962));
#23743=CARTESIAN_POINT('Ctrl Pts',(0.106677447021047,0.164166013275823,
1.31848989685777));
#23744=CARTESIAN_POINT('Ctrl Pts',(0.0961826403741802,0.170525090662696,
1.31918474009592));
#23745=CARTESIAN_POINT('Ctrl Pts',(0.0852071114949725,0.175843419412508,
1.31987958333407));
#23746=CARTESIAN_POINT('Ctrl Pts',(0.074206286774338,0.181174005576264,
1.32057602801161));
#23747=CARTESIAN_POINT('Ctrl Pts',(0.0627233438518345,0.18545873123927,
1.32127247268916));
#23748=CARTESIAN_POINT('Ctrl Pts',(0.0509791958083,0.188632663117338,1.32196891736671));
#23749=CARTESIAN_POINT('Ctrl Pts',(0.0471461479474023,0.189668569063922,
1.32219622255493));
#23750=CARTESIAN_POINT('Ctrl Pts',(0.0432853701297518,0.190586553608311,
1.32242352774315));
#23751=CARTESIAN_POINT('Ctrl Pts',(0.0394047390535147,0.191385544229768,
1.32265083293137));
#23752=CARTESIAN_POINT('Ctrl Pts',(0.0275148084935359,0.193833584978958,
1.3233472771052));
#23753=CARTESIAN_POINT('Ctrl Pts',(0.0153537894493235,0.19517805046233,
1.32404372127904));
#23754=CARTESIAN_POINT('Ctrl Pts',(0.00314675961872812,0.195374660342384,
1.32474016545288));
#23755=CARTESIAN_POINT('Ctrl Pts',(-0.0090346499974204,0.195570857576007,
1.32543514792396));
#23756=CARTESIAN_POINT('Ctrl Pts',(-0.0212610131337285,0.194623892383761,
1.32613013039504));
#23757=CARTESIAN_POINT('Ctrl Pts',(-0.0333023001143408,0.192541208075296,
1.32682511286613));
#23758=CARTESIAN_POINT('Ctrl Pts',(-0.0453418904262554,0.190458817225934,
1.32751999741122));
#23759=CARTESIAN_POINT('Ctrl Pts',(-0.0571955869326572,0.187241128538841,
1.32821488195631));
#23760=CARTESIAN_POINT('Ctrl Pts',(-0.0686401428152857,0.182947235000415,
1.3289097665014));
#23761=CARTESIAN_POINT('Ctrl Pts',(-0.0800840183840454,0.178653596709581,
1.32960460973955));
#23762=CARTESIAN_POINT('Ctrl Pts',(-0.0911179910588212,0.173284213245967,
1.3302994529777));
#23763=CARTESIAN_POINT('Ctrl Pts',(-0.101538208880341,0.16694655473346,
1.33099429621585));
#23764=CARTESIAN_POINT('Ctrl Pts',(-0.111982442690575,0.160594289507551,
1.33169074089339));
#23765=CARTESIAN_POINT('Ctrl Pts',(-0.121809383652032,0.153269804303219,
1.33238718557094));
#23766=CARTESIAN_POINT('Ctrl Pts',(-0.130844679170331,0.145123498899431,
1.33308363024849));
#23767=CARTESIAN_POINT('Ctrl Pts',(-0.13379361339957,0.14246471272045,1.33331093543671));
#23768=CARTESIAN_POINT('Ctrl Pts',(-0.136658507168464,0.139718682007989,
1.33353824062492));
#23769=CARTESIAN_POINT('Ctrl Pts',(-0.139434188009896,0.136891443173125,
1.33376554581314));
#23770=CARTESIAN_POINT('Ctrl Pts',(-0.148233905898102,0.127928271407112,
1.33448616956101));
#23771=CARTESIAN_POINT('Ctrl Pts',(-0.156202650445079,0.118075218915444,
1.33520679330888));
#23772=CARTESIAN_POINT('Ctrl Pts',(-0.16315981320051,0.107517604867179,
1.33592741705675));
#23773=CARTESIAN_POINT('Ctrl Pts',(-0.169780924334577,0.0974699549297682,
1.33661323253761));
#23774=CARTESIAN_POINT('Ctrl Pts',(-0.175485519694319,0.0867851739644082,
1.33729904801846));
#23775=CARTESIAN_POINT('Ctrl Pts',(-0.180158736660967,0.0756570525775642,
1.33798486349931));
#23776=CARTESIAN_POINT('Ctrl Pts',(-0.184827594402669,0.0645393116170316,
1.33867003924442));
#23777=CARTESIAN_POINT('Ctrl Pts',(-0.188466618912098,0.0529798735468401,
1.33935521498952));
#23778=CARTESIAN_POINT('Ctrl Pts',(-0.191008466011499,0.0411937605947046,
1.34004039073463));
#23779=CARTESIAN_POINT('Ctrl Pts',(-0.193552742713279,0.0293963819893101,
1.34072622139899));
#23780=CARTESIAN_POINT('Ctrl Pts',(-0.194997590648736,0.017372783340044,
1.34141205206336));
#23781=CARTESIAN_POINT('Ctrl Pts',(-0.195326811815141,0.005347577594793,
1.34209788272772));
#23782=CARTESIAN_POINT('Ctrl Pts',(-0.195377238943025,0.00350566507571935,
1.34220293208101));
#23783=CARTESIAN_POINT('Ctrl Pts',(-0.195401591571816,0.00166371687160794,
1.34230798143429));
#23784=CARTESIAN_POINT('Ctrl Pts',(-0.195399919414568,-0.000177462052753457,
1.34241303078758));
#23785=CARTESIAN_POINT('',(-0.195672555088735,8.72824817547956E-5,1.41241303078758));
#23786=CARTESIAN_POINT('Ctrl Pts',(-0.195421369810842,-0.000177481533986374,
1.34241303078758));
#23787=CARTESIAN_POINT('Ctrl Pts',(-0.19555443758116,-0.0145933993525209,
1.34323544009003));
#23788=CARTESIAN_POINT('Ctrl Pts',(-0.187517725154066,-0.0938051227660867,
1.34776275368636));
#23789=CARTESIAN_POINT('Ctrl Pts',(-0.0795606509348802,-0.21682299543957,
1.35599497157673));
#23790=CARTESIAN_POINT('Ctrl Pts',(0.139031233645666,-0.184424576994089,
1.36710968445844));
#23791=CARTESIAN_POINT('Ctrl Pts',(0.23034688085148,0.0168054458595032,
1.37822439734026));
#23792=CARTESIAN_POINT('Ctrl Pts',(0.110791319357882,0.202650911874206,
1.38933911022202));
#23793=CARTESIAN_POINT('Ctrl Pts',(-0.110188230774172,0.202979462821721,
1.4004538231038));
#23794=CARTESIAN_POINT('Ctrl Pts',(-0.193301926424826,0.0746222231139512,
1.40814512995899));
#23795=CARTESIAN_POINT('Ctrl Pts',(-0.195699991939521,0.00500518314638453,
1.41213153252024));
#23796=CARTESIAN_POINT('Ctrl Pts',(-0.195672555088735,8.72824817547956E-5,
1.41241303078758));
#23797=CARTESIAN_POINT('',(-0.195399961286389,0.000123001129209823,1.48241303078758));
#23798=CARTESIAN_POINT('Ctrl Pts',(-0.195672555088735,8.72824817547956E-5,
1.41241303078758));
#23799=CARTESIAN_POINT('Ctrl Pts',(-0.195338885254029,-0.0597211523368212,
1.41583643681417));
#23800=CARTESIAN_POINT('Ctrl Pts',(-0.134045287995802,-0.184847342684257,
1.42296474713469));
#23801=CARTESIAN_POINT('Ctrl Pts',(0.0789155585961739,-0.217058616829523,
1.43379796174912));
#23802=CARTESIAN_POINT('Ctrl Pts',(0.225166835685404,-0.0514004342001738,
1.44491267463091));
#23803=CARTESIAN_POINT('Ctrl Pts',(0.165288979944631,0.161312310867416,
1.45602738751267));
#23804=CARTESIAN_POINT('Ctrl Pts',(-0.0459027848741339,0.226351591267424,
1.46714210039446));
#23805=CARTESIAN_POINT('Ctrl Pts',(-0.17976876762693,0.113847497486333,
1.47593728692968));
#23806=CARTESIAN_POINT('Ctrl Pts',(-0.195300781734273,0.0244906930800311,
1.48102756917097));
#23807=CARTESIAN_POINT('Ctrl Pts',(-0.195160815401549,0.0001243221805799,
1.48241294711835));
#23808=CARTESIAN_POINT('',(-0.195399939368468,-0.00015393115033595,1.55241303078758));
#23809=CARTESIAN_POINT('Ctrl Pts',(-0.195399961286389,0.000123001129209823,
1.48241303078758));
#23810=CARTESIAN_POINT('Ctrl Pts',(-0.195407720443864,-0.0122032196137622,
1.48311299720329));
#23811=CARTESIAN_POINT('Ctrl Pts',(-0.194244791461965,-0.0245341129591015,
1.48381296361899));
#23812=CARTESIAN_POINT('Ctrl Pts',(-0.191934714154944,-0.0366363958688599,
1.4845129300347));
#23813=CARTESIAN_POINT('Ctrl Pts',(-0.189623997762733,-0.0487420268872529,
1.48521309009681));
#23814=CARTESIAN_POINT('Ctrl Pts',(-0.186165702326191,-0.0606180869632981,
1.48591325015893));
#23815=CARTESIAN_POINT('Ctrl Pts',(-0.181634190272556,-0.0720429102968012,
1.48661341022104));
#23816=CARTESIAN_POINT('Ctrl Pts',(-0.177090695339426,-0.0834979448003588,
1.48731542174764));
#23817=CARTESIAN_POINT('Ctrl Pts',(-0.171468700646835,-0.0944985906177856,
1.48801743327425));
#23818=CARTESIAN_POINT('Ctrl Pts',(-0.164889693248902,-0.1048453578385,
1.48871944480085));
#23819=CARTESIAN_POINT('Ctrl Pts',(-0.162852666832545,-0.108048977606294,
1.48893680525324));
#23820=CARTESIAN_POINT('Ctrl Pts',(-0.160724203558817,-0.111190127957947,
1.48915416570562));
#23821=CARTESIAN_POINT('Ctrl Pts',(-0.158508702339993,-0.11426351684808,
1.48937152615801));
#23822=CARTESIAN_POINT('Ctrl Pts',(-0.151410019488453,-0.124110955804618,
1.49006797033184));
#23823=CARTESIAN_POINT('Ctrl Pts',(-0.143365032956223,-0.133329207446043,
1.49076441450568));
#23824=CARTESIAN_POINT('Ctrl Pts',(-0.134509516318977,-0.141733376519558,
1.49146085867951));
#23825=CARTESIAN_POINT('Ctrl Pts',(-0.125672585712767,-0.150119906854011,
1.49215584115059));
#23826=CARTESIAN_POINT('Ctrl Pts',(-0.116029078960968,-0.157695095045935,
1.49285082362167));
#23827=CARTESIAN_POINT('Ctrl Pts',(-0.105753412717894,-0.164308781562395,
1.49354580609275));
#23828=CARTESIAN_POINT('Ctrl Pts',(-0.0954791943600241,-0.170921536182214,
1.49424069063784));
#23829=CARTESIAN_POINT('Ctrl Pts',(-0.0845737036217037,-0.17657254610153,
1.49493557518293));
#23830=CARTESIAN_POINT('Ctrl Pts',(-0.0732413093382392,-0.181154272945521,
1.49563045972802));
#23831=CARTESIAN_POINT('Ctrl Pts',(-0.061909588701269,-0.185735727431866,
1.49632530296616));
#23832=CARTESIAN_POINT('Ctrl Pts',(-0.0501518368335319,-0.189247721563803,
1.49702014620431));
#23833=CARTESIAN_POINT('Ctrl Pts',(-0.0381908737766618,-0.191631461822361,
1.49771498944245));
#23834=CARTESIAN_POINT('Ctrl Pts',(-0.0262023436997301,-0.194020696004378,
1.49841143412));
#23835=CARTESIAN_POINT('Ctrl Pts',(-0.014010538428915,-0.195276377654251,
1.49910787879754));
#23836=CARTESIAN_POINT('Ctrl Pts',(-0.0018456030229129,-0.195391283709079,
1.49980432347509));
#23837=CARTESIAN_POINT('Ctrl Pts',(0.00212478116040987,-0.19542878667703,
1.50003162866332));
#23838=CARTESIAN_POINT('Ctrl Pts',(0.00609231336375039,-0.195345185252779,
1.50025893385155));
#23839=CARTESIAN_POINT('Ctrl Pts',(0.0100491005886018,-0.195141424555014,
1.50048623903978));
#23840=CARTESIAN_POINT('Ctrl Pts',(0.0221723672473985,-0.194517118739913,
1.50118268321362));
#23841=CARTESIAN_POINT('Ctrl Pts',(0.0342801464245863,-0.192756535022393,
1.50187912738746));
#23842=CARTESIAN_POINT('Ctrl Pts',(0.0461434623222685,-0.189873486524352,
1.50257557156129));
#23843=CARTESIAN_POINT('Ctrl Pts',(0.0579818793951278,-0.186996488992173,
1.50327055403238));
#23844=CARTESIAN_POINT('Ctrl Pts',(0.0695759915653924,-0.183001834864492,
1.50396553650346));
#23845=CARTESIAN_POINT('Ctrl Pts',(0.080705052869171,-0.177954641528071,
1.50466051897455));
#23846=CARTESIAN_POINT('Ctrl Pts',(0.0918325460407418,-0.172908159362719,
1.50535540351964));
#23847=CARTESIAN_POINT('Ctrl Pts',(0.102494303098156,-0.166809751553959,
1.50605028806473));
#23848=CARTESIAN_POINT('Ctrl Pts',(0.112489146120411,-0.159772813723426,
1.50674517260982));
#23849=CARTESIAN_POINT('Ctrl Pts',(0.122483395006,-0.152736294198892,1.50744001584797));
#23850=CARTESIAN_POINT('Ctrl Pts',(0.131810107872335,-0.144761881438288,
1.50813485908612));
#23851=CARTESIAN_POINT('Ctrl Pts',(0.14029905666712,-0.136004906890584,
1.50882970232427));
#23852=CARTESIAN_POINT('Ctrl Pts',(0.148807570359864,-0.12722774971278,
1.50952614700182));
#23853=CARTESIAN_POINT('Ctrl Pts',(0.156473902749328,-0.117665103642622,
1.51022259167937));
#23854=CARTESIAN_POINT('Ctrl Pts',(0.163167183175346,-0.107506419969335,
1.51091903635692));
#23855=CARTESIAN_POINT('Ctrl Pts',(0.165351731950102,-0.104190835000663,
1.51114634154513));
#23856=CARTESIAN_POINT('Ctrl Pts',(0.167432982102897,-0.100811974426125,
1.51137364673335));
#23857=CARTESIAN_POINT('Ctrl Pts',(0.169407447550582,-0.0973769824670943,
1.51160095192157));
#23858=CARTESIAN_POINT('Ctrl Pts',(0.175457045310609,-0.0868524530632367,
1.5122973960954));
#23859=CARTESIAN_POINT('Ctrl Pts',(0.18054354245229,-0.0757247615480432,
1.51299384026924));
#23860=CARTESIAN_POINT('Ctrl Pts',(0.184554377005386,-0.0641937841862738,
1.51369028444307));
#23861=CARTESIAN_POINT('Ctrl Pts',(0.188556793585986,-0.0526870081344792,
1.51438526691415));
#23862=CARTESIAN_POINT('Ctrl Pts',(0.191487673305,-0.0407794205245224,1.51508024938524));
#23863=CARTESIAN_POINT('Ctrl Pts',(0.193282022931698,-0.0286918039068726,
1.51577523185632));
#23864=CARTESIAN_POINT('Ctrl Pts',(0.195076119726881,-0.0166058904859631,
1.51647011640141));
#23865=CARTESIAN_POINT('Ctrl Pts',(0.195733830355679,-0.00434085652426346,
1.5171650009465));
#23866=CARTESIAN_POINT('Ctrl Pts',(0.195241336275968,0.00787277645905997,
1.51785988549159));
#23867=CARTESIAN_POINT('Ctrl Pts',(0.194748871472234,0.0200856834112485,
1.51855472872974));
#23868=CARTESIAN_POINT('Ctrl Pts',(0.193106399701943,0.0322463214804775,
1.51924957196789));
#23869=CARTESIAN_POINT('Ctrl Pts',(0.190352120288359,0.0441274325304136,
1.51994441520604));
#23870=CARTESIAN_POINT('Ctrl Pts',(0.187591492951492,0.0560359265615691,
1.52064085988358));
#23871=CARTESIAN_POINT('Ctrl Pts',(0.183714203260911,0.0676627695046786,
1.52133730456113));
#23872=CARTESIAN_POINT('Ctrl Pts',(0.178808460589818,0.0787952690299328,
1.52203374923868));
#23873=CARTESIAN_POINT('Ctrl Pts',(0.177207327295025,0.0824286874212366,
1.5222610544269));
#23874=CARTESIAN_POINT('Ctrl Pts',(0.175497013530002,0.0860096269356705,
1.52248835961512));
#23875=CARTESIAN_POINT('Ctrl Pts',(0.173681631464147,0.0895312844314901,
1.52271566480333));
#23876=CARTESIAN_POINT('Ctrl Pts',(0.168119451942595,0.10032134982521,1.52341210897717));
#23877=CARTESIAN_POINT('Ctrl Pts',(0.161528229781885,0.110629296374245,
1.524108553151));
#23878=CARTESIAN_POINT('Ctrl Pts',(0.154014861771623,0.120252161533454,
1.52480499732484));
#23879=CARTESIAN_POINT('Ctrl Pts',(0.146517262879838,0.129854830144247,
1.52549997979592));
#23880=CARTESIAN_POINT('Ctrl Pts',(0.138101834316003,0.138774542062417,
1.52619496226701));
#23881=CARTESIAN_POINT('Ctrl Pts',(0.128918833679812,0.146836965109733,
1.52688994473809));
#23882=CARTESIAN_POINT('Ctrl Pts',(0.119737126967578,0.154898252127254,
1.52758482928318));
#23883=CARTESIAN_POINT('Ctrl Pts',(0.109788689525428,0.162101878562092,
1.52827971382827));
#23884=CARTESIAN_POINT('Ctrl Pts',(0.0992597123839005,0.168311228079012,
1.52897459837336));
#23885=CARTESIAN_POINT('Ctrl Pts',(0.0887313611302768,0.174520208485363,
1.52966944161151));
#23886=CARTESIAN_POINT('Ctrl Pts',(0.0776233066222674,0.179734607474173,
1.53036428484966));
#23887=CARTESIAN_POINT('Ctrl Pts',(0.0661472059622404,0.183863283837173,
1.53105912808781));
#23888=CARTESIAN_POINT('Ctrl Pts',(0.0546446557683793,0.188001475763725,
1.53175557276536));
#23889=CARTESIAN_POINT('Ctrl Pts',(0.042773211481347,0.191048714301895,
1.53245201744291));
#23890=CARTESIAN_POINT('Ctrl Pts',(0.0307594111770352,0.192963775419228,
1.53314846212046));
#23891=CARTESIAN_POINT('Ctrl Pts',(0.0268383543760548,0.193588811896296,
1.53337576730868));
#23892=CARTESIAN_POINT('Ctrl Pts',(0.022902184592286,0.19409365683727,1.5336030724969));
#23893=CARTESIAN_POINT('Ctrl Pts',(0.018958847759401,0.19447807612077,1.53383037768512));
#23894=CARTESIAN_POINT('Ctrl Pts',(0.00687679198126068,0.195655904802991,
1.53452682185895));
#23895=CARTESIAN_POINT('Ctrl Pts',(-0.00535821067313899,0.195707689708688,
1.53522326603279));
#23896=CARTESIAN_POINT('Ctrl Pts',(-0.0175176633930722,0.194613184212291,
1.53591971020662));
#23897=CARTESIAN_POINT('Ctrl Pts',(-0.0296515957537918,0.193520975873016,
1.53661469267771));
#23898=CARTESIAN_POINT('Ctrl Pts',(-0.0417094227996702,0.191287255758967,
1.53730967514879));
#23899=CARTESIAN_POINT('Ctrl Pts',(-0.0534631895223959,0.187943734575251,
1.53800465761987));
#23900=CARTESIAN_POINT('Ctrl Pts',(-0.0652153000892538,0.184600684507931,
1.53869954216496));
#23901=CARTESIAN_POINT('Ctrl Pts',(-0.0766625817815175,0.180148338698035,
1.53939442671005));
#23902=CARTESIAN_POINT('Ctrl Pts',(-0.087589282701494,0.174669051511244,
1.54008931125514));
#23903=CARTESIAN_POINT('Ctrl Pts',(-0.0985153340911449,0.169190090036964,
1.54078415449329));
#23904=CARTESIAN_POINT('Ctrl Pts',(-0.108920095284611,0.162684724845514,
1.54147899773144));
#23905=CARTESIAN_POINT('Ctrl Pts',(-0.118612213038698,0.15528136693777,
1.54217384096959));
#23906=CARTESIAN_POINT('Ctrl Pts',(-0.128326668693444,0.147860946146797,
1.54287028564714));
#23907=CARTESIAN_POINT('Ctrl Pts',(-0.137324545832395,0.139538983688291,
1.54356673032468));
#23908=CARTESIAN_POINT('Ctrl Pts',(-0.145448362112576,0.130483462395696,
1.54426317500223));
#23909=CARTESIAN_POINT('Ctrl Pts',(-0.148099808305136,0.127527926890607,
1.54449048019045));
#23910=CARTESIAN_POINT('Ctrl Pts',(-0.150658464802673,0.124494516613643,
1.54471778537867));
#23911=CARTESIAN_POINT('Ctrl Pts',(-0.153119826017623,0.121389780790364,
1.54494509056688));
#23912=CARTESIAN_POINT('Ctrl Pts',(-0.160650574807049,0.111890571409546,
1.54564055056707));
#23913=CARTESIAN_POINT('Ctrl Pts',(-0.167321842354435,0.101652732245817,
1.54633601056725));
#23914=CARTESIAN_POINT('Ctrl Pts',(-0.172992199724487,0.0908562536894579,
1.54703147056743));
#23915=CARTESIAN_POINT('Ctrl Pts',(-0.178650312965688,0.0800830882095001,
1.54772542884536));
#23916=CARTESIAN_POINT('Ctrl Pts',(-0.183311330666581,0.068754408789931,
1.54841938712329));
#23917=CARTESIAN_POINT('Ctrl Pts',(-0.186877610749096,0.0570781797249134,
1.54911334540122));
#23918=CARTESIAN_POINT('Ctrl Pts',(-0.190442306291453,0.0454071385457058,
1.54980699534533));
#23919=CARTESIAN_POINT('Ctrl Pts',(-0.19291293103831,0.0333896787299648,
1.55050064528944));
#23920=CARTESIAN_POINT('Ctrl Pts',(-0.194240964325203,0.0212510653383588,
1.55119429523355));
#23921=CARTESIAN_POINT('Ctrl Pts',(-0.195018744432406,0.0141419272480706,
1.55160054041823));
#23922=CARTESIAN_POINT('Ctrl Pts',(-0.195405568361647,0.00699150317808594,
1.5520067856029));
#23923=CARTESIAN_POINT('Ctrl Pts',(-0.195399939368468,-0.00015393115033595,
1.55241303078758));
#23924=CARTESIAN_POINT('',(-0.195712283470102,-3.61459064724743E-5,1.62241303078758));
#23925=CARTESIAN_POINT('Ctrl Pts',(-0.195226198903123,-0.000155160406305955,
1.55241310852604));
#23926=CARTESIAN_POINT('Ctrl Pts',(-0.195383351547435,-0.0215168196864403,
1.55362867350025));
#23927=CARTESIAN_POINT('Ctrl Pts',(-0.182302395685712,-0.107798996787892,
1.55854914276838));
#23928=CARTESIAN_POINT('Ctrl Pts',(-0.0562017238658613,-0.224016684117646,
1.56717451633045));
#23929=CARTESIAN_POINT('Ctrl Pts',(0.157742334325191,-0.168699331623246,
1.57828922921221));
#23930=CARTESIAN_POINT('Ctrl Pts',(0.227281065301869,0.0410539387122334,
1.589403942094));
#23931=CARTESIAN_POINT('Ctrl Pts',(0.0887551905086346,0.21322435293907,
1.60051865497576));
#23932=CARTESIAN_POINT('Ctrl Pts',(-0.128813312714937,0.190429758735974,
1.6115216845403));
#23933=CARTESIAN_POINT('Ctrl Pts',(-0.195552549538933,0.0627050974813158,
1.6188198098109));
#23934=CARTESIAN_POINT('Ctrl Pts',(-0.195712283470102,-3.61459064724743E-5,
1.62241303078758));
#23935=CARTESIAN_POINT('',(-0.195399920371161,0.000176405623024491,1.69241303078758));
#23936=CARTESIAN_POINT('Ctrl Pts',(-0.195712283470102,-3.61459064724743E-5,
1.62241303078758));
#23937=CARTESIAN_POINT('Ctrl Pts',(-0.195717248267821,-0.00198624867923799,
1.62252471410483));
#23938=CARTESIAN_POINT('Ctrl Pts',(-0.195690623309908,-0.0039362125300576,
1.62263639742207));
#23939=CARTESIAN_POINT('Ctrl Pts',(-0.193686975727267,-0.0705400096200497,
1.62645298503325));
#23940=CARTESIAN_POINT('Ctrl Pts',(-0.119351590043147,-0.197730388364331,
1.63386279362109));
#23941=CARTESIAN_POINT('Ctrl Pts',(0.101411982740744,-0.207503538006193,
1.64497750650288));
#23942=CARTESIAN_POINT('Ctrl Pts',(0.229337886969936,-0.0273174326888311,
1.65609221938464));
#23943=CARTESIAN_POINT('Ctrl Pts',(0.14731626663462,0.177876434957931,1.66720693226643));
#23944=CARTESIAN_POINT('Ctrl Pts',(-0.069566130158676,0.220233199275866,
1.67832164514821));
#23945=CARTESIAN_POINT('Ctrl Pts',(-0.185374172661697,0.0998458182017167,
1.686723666339));
#23946=CARTESIAN_POINT('Ctrl Pts',(-0.195485375409074,0.0175896061910127,
1.69142078323589));
#23947=CARTESIAN_POINT('Ctrl Pts',(-0.195332205722473,0.000176957812133139,
1.69241299583884));
#23948=CARTESIAN_POINT('',(-0.195379429215978,-6.88592766845772E-5,1.76241303461069));
#23949=CARTESIAN_POINT('Ctrl Pts',(-0.195399920371161,0.000176405623024491,
1.69241303078758));
#23950=CARTESIAN_POINT('Ctrl Pts',(-0.195410833012155,-0.0119112429713591,
1.69310157998606));
#23951=CARTESIAN_POINT('Ctrl Pts',(-0.194295777173492,-0.0240245763136542,
1.69379012918454));
#23952=CARTESIAN_POINT('Ctrl Pts',(-0.192066928524843,-0.0359368191000951,
1.69447867838301));
#23953=CARTESIAN_POINT('Ctrl Pts',(-0.189839819899382,-0.0478397622067734,
1.69516669004317));
#23954=CARTESIAN_POINT('Ctrl Pts',(-0.186500797960111,-0.0595410443737312,
1.69585470170332));
#23955=CARTESIAN_POINT('Ctrl Pts',(-0.182113456174281,-0.0708226593701344,
1.69654271336347));
#23956=CARTESIAN_POINT('Ctrl Pts',(-0.177715401429773,-0.0821318216790538,
1.69723240500226));
#23957=CARTESIAN_POINT('Ctrl Pts',(-0.17226425745159,-0.0930184370182762,
1.69792209664105));
#23958=CARTESIAN_POINT('Ctrl Pts',(-0.165872091364467,-0.103284119332925,
1.69861178827985));
#23959=CARTESIAN_POINT('Ctrl Pts',(-0.159880903430725,-0.112905839290898,
1.69925821582381));
#23960=CARTESIAN_POINT('Ctrl Pts',(-0.153063879326051,-0.121981825796497,
1.69990464336778));
#23961=CARTESIAN_POINT('Ctrl Pts',(-0.14554597808314,-0.130374569083936,
1.70055107091175));
#23962=CARTESIAN_POINT('Ctrl Pts',(-0.137446387388151,-0.139416691777484,
1.70124751508559));
#23963=CARTESIAN_POINT('Ctrl Pts',(-0.128472283185883,-0.147733146875496,
1.70194395925943));
#23964=CARTESIAN_POINT('Ctrl Pts',(-0.118778218134343,-0.155154422743377,
1.70264040343326));
#23965=CARTESIAN_POINT('Ctrl Pts',(-0.109104499066135,-0.162560122776527,
1.70333538590435));
#23966=CARTESIAN_POINT('Ctrl Pts',(-0.0987144613648414,-0.169073786506153,
1.70403036837544));
#23967=CARTESIAN_POINT('Ctrl Pts',(-0.0877974135801952,-0.174564527234568,
1.70472535084652));
#23968=CARTESIAN_POINT('Ctrl Pts',(-0.0768819040541493,-0.180054494294193,
1.70542023539162));
#23969=CARTESIAN_POINT('Ctrl Pts',(-0.0654402922705117,-0.184521390436504,
1.70611511993671));
#23970=CARTESIAN_POINT('Ctrl Pts',(-0.0536871671213206,-0.187879876747052,
1.7068100044818));
#23971=CARTESIAN_POINT('Ctrl Pts',(-0.0419347406286866,-0.191238163414658,
1.70750484771995));
#23972=CARTESIAN_POINT('Ctrl Pts',(-0.0298716869347652,-0.193487956148545,
1.7081996909581));
#23973=CARTESIAN_POINT('Ctrl Pts',(-0.017725791559956,-0.194594337825058,
1.70889453419625));
#23974=CARTESIAN_POINT('Ctrl Pts',(-0.00555190294247328,-0.195703269433858,
1.7095909788738));
#23975=CARTESIAN_POINT('Ctrl Pts',(0.00670433105061121,-0.19566351423298,
1.71028742355135));
#23976=CARTESIAN_POINT('Ctrl Pts',(0.0188132907613911,-0.194492210874182,
1.7109838682289));
#23977=CARTESIAN_POINT('Ctrl Pts',(0.0227654056311449,-0.194109921599805,
1.71121117341711));
#23978=CARTESIAN_POINT('Ctrl Pts',(0.0267018864214747,-0.193607507460575,
1.71143847860533));
#23979=CARTESIAN_POINT('Ctrl Pts',(0.0306149842097358,-0.192986742399155,
1.71166578379354));
#23980=CARTESIAN_POINT('Ctrl Pts',(0.0426043900729254,-0.191084769928805,
1.71236222796737));
#23981=CARTESIAN_POINT('Ctrl Pts',(0.0544583156073996,-0.188054518940477,
1.7130586721412));
#23982=CARTESIAN_POINT('Ctrl Pts',(0.0659505269305032,-0.183933922911433,
1.71375511631504));
#23983=CARTESIAN_POINT('Ctrl Pts',(0.0774186183061158,-0.17982197522317,
1.71445009878612));
#23984=CARTESIAN_POINT('Ctrl Pts',(0.0885256610797746,-0.174624447018356,
1.7151450812572));
#23985=CARTESIAN_POINT('Ctrl Pts',(0.0990590268509342,-0.168429419043544,
1.71584006372829));
#23986=CARTESIAN_POINT('Ctrl Pts',(0.109590908425927,-0.162235263974599,
1.71653494827337));
#23987=CARTESIAN_POINT('Ctrl Pts',(0.119548496428216,-0.155044291680869,
1.71722983281846));
#23988=CARTESIAN_POINT('Ctrl Pts',(0.12874372287406,-0.146990522893577,
1.71792471736355));
#23989=CARTESIAN_POINT('Ctrl Pts',(0.137938402715909,-0.138937232857105,
1.7186195606017));
#23990=CARTESIAN_POINT('Ctrl Pts',(0.146370169794315,-0.130021845277062,
1.71931440383985));
#23991=CARTESIAN_POINT('Ctrl Pts',(0.153886164381613,-0.120416811168189,
1.720009247078));
#23992=CARTESIAN_POINT('Ctrl Pts',(0.161419481451435,-0.110789639864622,
1.72070569175554));
#23993=CARTESIAN_POINT('Ctrl Pts',(0.168032324202524,-0.100470378121775,
1.72140213643309));
#23994=CARTESIAN_POINT('Ctrl Pts',(0.173614575630121,-0.0896612465269868,
1.72209858111064));
#23995=CARTESIAN_POINT('Ctrl Pts',(0.175436507439444,-0.0861333687631246,
1.72232588629886));
#23996=CARTESIAN_POINT('Ctrl Pts',(0.177149032218288,-0.0825534861025725,
1.72255319148708));
#23997=CARTESIAN_POINT('Ctrl Pts',(0.178749438391155,-0.0789290711642203,
1.7227804966753));
#23998=CARTESIAN_POINT('Ctrl Pts',(0.183652949672968,-0.0678241655212152,
1.72347694084914));
#23999=CARTESIAN_POINT('Ctrl Pts',(0.187535012349117,-0.0562212537742335,
1.72417338502297));
#24000=CARTESIAN_POINT('Ctrl Pts',(0.190304817273997,-0.0443309882848414,
1.72486982919681));
#24001=CARTESIAN_POINT('Ctrl Pts',(0.193068808909556,-0.0324656781822966,
1.72556481166789));
#24002=CARTESIAN_POINT('Ctrl Pts',(0.194724906896276,-0.0203150387721786,
1.72625979413898));
#24003=CARTESIAN_POINT('Ctrl Pts',(0.19523181379665,-0.00810548466595916,
1.72695477661007));
#24004=CARTESIAN_POINT('Ctrl Pts',(0.19573864927168,0.00410234906200601,
1.72764966115516));
#24005=CARTESIAN_POINT('Ctrl Pts',(0.195096532785329,0.0163682093160225,
1.72834454570025));
#24006=CARTESIAN_POINT('Ctrl Pts',(0.193316084225746,0.0284614050887209,
1.72903943024534));
#24007=CARTESIAN_POINT('Ctrl Pts',(0.19153574150372,0.0405538819896001,
1.72973427348349));
#24008=CARTESIAN_POINT('Ctrl Pts',(0.188617355061553,0.0524728522614664,
1.73042911672164));
#24009=CARTESIAN_POINT('Ctrl Pts',(0.184622926505938,0.0639963671498853,
1.73112395995979));
#24010=CARTESIAN_POINT('Ctrl Pts',(0.180619291794299,0.0755464408500449,
1.73182040463734));
#24011=CARTESIAN_POINT('Ctrl Pts',(0.175535011910544,0.0866984339558695,
1.73251684931489));
#24012=CARTESIAN_POINT('Ctrl Pts',(0.169480279189942,0.0972501669186187,
1.73321329399243));
#24013=CARTESIAN_POINT('Ctrl Pts',(0.167504139225009,0.100694035074194,
1.73344059918065));
#24014=CARTESIAN_POINT('Ctrl Pts',(0.165424976018988,0.104074180240251,
1.73366790436887));
#24015=CARTESIAN_POINT('Ctrl Pts',(0.163247597657166,0.107384271935717,
1.73389520955709));
#24016=CARTESIAN_POINT('Ctrl Pts',(0.156576291620506,0.117526117329728,
1.73459165373093));
#24017=CARTESIAN_POINT('Ctrl Pts',(0.148932654521822,0.127079796387206,
1.73528809790476));
#24018=CARTESIAN_POINT('Ctrl Pts',(0.140444433246649,0.135854779709907,
1.7359845420786));
#24019=CARTESIAN_POINT('Ctrl Pts',(0.131974027119994,0.144611346025552,
1.73667952454968));
#24020=CARTESIAN_POINT('Ctrl Pts',(0.122663104291756,0.152591785531161,
1.73737450702076));
#24021=CARTESIAN_POINT('Ctrl Pts',(0.112679504054717,0.159638621160367,
1.73806948949185));
#24022=CARTESIAN_POINT('Ctrl Pts',(0.102697310549535,0.166684463860375,
1.73876437403694));
#24023=CARTESIAN_POINT('Ctrl Pts',(0.0920433155485732,0.172796421964969,
1.73945925858203));
#24024=CARTESIAN_POINT('Ctrl Pts',(0.0809171048280429,0.177858320430188,
1.74015414312712));
#24025=CARTESIAN_POINT('Ctrl Pts',(0.0697915554975698,0.182919917994283,
1.74084898636527));
#24026=CARTESIAN_POINT('Ctrl Pts',(0.0581946543876748,0.186931241518287,
1.74154382960342));
#24027=CARTESIAN_POINT('Ctrl Pts',(0.0463465050264075,0.189824027646231,
1.74223867284156));
#24028=CARTESIAN_POINT('Ctrl Pts',(0.0344710486523428,0.192723480920699,
1.74293511751911));
#24029=CARTESIAN_POINT('Ctrl Pts',(0.0223440536103823,0.194499105717973,
1.74363156219666));
#24030=CARTESIAN_POINT('Ctrl Pts',(0.0101951459275736,0.195133848933278,
1.74432800687421));
#24031=CARTESIAN_POINT('Ctrl Pts',(0.00622999286299049,0.19534101603596,
1.74455531206242));
#24032=CARTESIAN_POINT('Ctrl Pts',(0.00226251304281278,0.195427067517,1.74478261725064));
#24033=CARTESIAN_POINT('Ctrl Pts',(-0.00169936735183612,0.195392610276345,
1.74500992243886));
#24034=CARTESIAN_POINT('Ctrl Pts',(-0.0138382390595514,0.195287036159498,
1.7457063666127));
#24035=CARTESIAN_POINT('Ctrl Pts',(-0.0260102031537887,0.194045560538314,
1.74640281078653));
#24036=CARTESIAN_POINT('Ctrl Pts',(-0.0379859026910966,0.191672197245043,
1.74709925496037));
#24037=CARTESIAN_POINT('Ctrl Pts',(-0.0499364675318776,0.18930381518614,
1.74779423743145));
#24038=CARTESIAN_POINT('Ctrl Pts',(-0.0616907205410164,0.185808356015568,
1.74848921990253));
#24039=CARTESIAN_POINT('Ctrl Pts',(-0.0730253342901441,0.181241442699546,
1.74918420237362));
#24040=CARTESIAN_POINT('Ctrl Pts',(-0.0843583509438475,0.176675172881089,
1.7498790869187));
#24041=CARTESIAN_POINT('Ctrl Pts',(-0.0952710174916307,0.17103803263362,
1.75057397146379));
#24042=CARTESIAN_POINT('Ctrl Pts',(-0.105557493203762,0.16443471539957,
1.75126885600888));
#24043=CARTESIAN_POINT('Ctrl Pts',(-0.115843357443317,0.157831790695238,
1.75196369924703));
#24044=CARTESIAN_POINT('Ctrl Pts',(-0.125502382214613,0.150263298623869,
1.75265854248518));
#24045=CARTESIAN_POINT('Ctrl Pts',(-0.134357855992658,0.141877152963598,
1.75335338572333));
#24046=CARTESIAN_POINT('Ctrl Pts',(-0.143233739416826,0.133471679340809,
1.75404983040087));
#24047=CARTESIAN_POINT('Ctrl Pts',(-0.151301783760117,0.12424543890156,
1.75474627507842));
#24048=CARTESIAN_POINT('Ctrl Pts',(-0.158423140606298,0.114382116261403,
1.75544271975596));
#24049=CARTESIAN_POINT('Ctrl Pts',(-0.160747404701511,0.111162931046114,
1.75567002494419));
#24050=CARTESIAN_POINT('Ctrl Pts',(-0.162971169036832,0.107876112955241,
1.75589733013241));
#24051=CARTESIAN_POINT('Ctrl Pts',(-0.165090645363197,0.104528650682782,
1.75612463532063));
#24052=CARTESIAN_POINT('Ctrl Pts',(-0.171745889793215,0.0940174789530729,
1.75683838313136));
#24053=CARTESIAN_POINT('Ctrl Pts',(-0.177414693780258,0.0828351242330211,
1.75755213094209));
#24054=CARTESIAN_POINT('Ctrl Pts',(-0.181971776211685,0.0711859021321252,
1.75826587875282));
#24055=CARTESIAN_POINT('Ctrl Pts',(-0.186516759932967,0.0595676078372813,
1.75897773161695));
#24056=CARTESIAN_POINT('Ctrl Pts',(-0.189955514046892,0.0474856300317684,
1.75968958448107));
#24057=CARTESIAN_POINT('Ctrl Pts',(-0.192209326398065,0.035167241086016,
1.7604014373452));
#24058=CARTESIAN_POINT('Ctrl Pts',(-0.194332309191495,0.0235639113939933,
1.76107196849266));
#24059=CARTESIAN_POINT('Ctrl Pts',(-0.1954041497732,0.0117515712181993,
1.76174249964012));
#24060=CARTESIAN_POINT('Ctrl Pts',(-0.195399987888093,-6.87992227970692E-5,
1.76241303078758));
#24061=CARTESIAN_POINT('',(-0.195583821122648,-0.000140590296505579,1.83241303078758));
#24062=CARTESIAN_POINT('Ctrl Pts',(-0.195102051502741,-6.96695240533898E-5,
1.76241308619214));
#24063=CARTESIAN_POINT('Ctrl Pts',(-0.195191304682355,-0.0283861708385786,
1.76402184019557));
#24064=CARTESIAN_POINT('Ctrl Pts',(-0.17616558588852,-0.121800052143105,
1.76933549849292));
#24065=CARTESIAN_POINT('Ctrl Pts',(-0.0322133827789196,-0.228701566453772,
1.77835406108418));
#24066=CARTESIAN_POINT('Ctrl Pts',(0.174686847974585,-0.151084789682017,
1.78946877396597));
#24067=CARTESIAN_POINT('Ctrl Pts',(0.221669884971711,0.0648426605340514,
1.80058348684773));
#24068=CARTESIAN_POINT('Ctrl Pts',(0.0657250750476474,0.221409853074599,
1.81169819972952));
#24069=CARTESIAN_POINT('Ctrl Pts',(-0.14057127916716,0.177382277682992,
1.82230804770946));
#24070=CARTESIAN_POINT('Ctrl Pts',(-0.195129223210545,0.0558321996894708,
1.82921299139548));
#24071=CARTESIAN_POINT('Ctrl Pts',(-0.195583821122648,-0.000140590296505579,
1.83241303078758));
#24072=CARTESIAN_POINT('',(-0.19539993725538,0.000156590528830125,1.90241303078758));
#24073=CARTESIAN_POINT('Ctrl Pts',(-0.195583821122648,-0.000140590296505579,
1.83241303078758));
#24074=CARTESIAN_POINT('Ctrl Pts',(-0.195655542280467,-0.0089713244403536,
1.83291789568941));
#24075=CARTESIAN_POINT('Ctrl Pts',(-0.191100149777636,-0.0825311564103834,
1.83712766488517));
#24076=CARTESIAN_POINT('Ctrl Pts',(-0.0977875181872751,-0.209236014622781,
1.84504233837484));
#24077=CARTESIAN_POINT('Ctrl Pts',(0.122772674400008,-0.195624586770786,
1.85615705125663));
#24078=CARTESIAN_POINT('Ctrl Pts',(0.23094053872867,-0.00292849794470196,
1.86727176413839));
#24079=CARTESIAN_POINT('Ctrl Pts',(0.127693729850807,0.19244848631601,1.87838647702018));
#24080=CARTESIAN_POINT('Ctrl Pts',(-0.0924503908440486,0.211648372923799,
1.88950118990194));
#24081=CARTESIAN_POINT('Ctrl Pts',(-0.190094138242322,0.0858713855005268,
1.89751004115775));
#24082=CARTESIAN_POINT('Ctrl Pts',(-0.195629876801359,0.0106410776720159,
1.90181398811963));
#24083=CARTESIAN_POINT('Ctrl Pts',(-0.195538264906755,0.000156701382499669,
1.90241303078758));
#24084=CARTESIAN_POINT('',(-0.195372356109538,4.29160852750294E-5,1.9724130286148));
#24085=CARTESIAN_POINT('Ctrl Pts',(-0.19539993725538,0.000156590528830125,
1.90241303078758));
#24086=CARTESIAN_POINT('Ctrl Pts',(-0.195409542393633,-0.0118290859102397,
1.90309834283115));
#24087=CARTESIAN_POINT('Ctrl Pts',(-0.194312055128761,-0.0238549391754707,
1.90378365487473));
#24088=CARTESIAN_POINT('Ctrl Pts',(-0.19211167027849,-0.0356968646075353,
1.90446896691831));
#24089=CARTESIAN_POINT('Ctrl Pts',(-0.189912810686787,-0.0475305814763519,
1.90515380391859));
#24090=CARTESIAN_POINT('Ctrl Pts',(-0.186612662947961,-0.0591797252615298,
1.90583864091887));
#24091=CARTESIAN_POINT('Ctrl Pts',(-0.18226715366032,-0.0704261648577097,
1.90652347791916));
#24092=CARTESIAN_POINT('Ctrl Pts',(-0.177923622048415,-0.0816674861100453,
1.90720800324469));
#24093=CARTESIAN_POINT('Ctrl Pts',(-0.172536007022654,-0.0925056261125338,
1.90789252857022));
#24094=CARTESIAN_POINT('Ctrl Pts',(-0.166208799716543,-0.10274139816445,
1.90857705389576));
#24095=CARTESIAN_POINT('Ctrl Pts',(-0.159867367576225,-0.113000182289999,
1.90926311817186));
#24096=CARTESIAN_POINT('Ctrl Pts',(-0.152582645835605,-0.122653150995453,
1.90994918244796));
#24097=CARTESIAN_POINT('Ctrl Pts',(-0.144502250188905,-0.131530451570513,
1.91063524672406));
#24098=CARTESIAN_POINT('Ctrl Pts',(-0.140201868657935,-0.13625494540807,
1.91100036970454));
#24099=CARTESIAN_POINT('Ctrl Pts',(-0.135676795206366,-0.1407603317352,
1.91136549268502));
#24100=CARTESIAN_POINT('Ctrl Pts',(-0.130953256157671,-0.145025531206417,
1.91173061566551));
#24101=CARTESIAN_POINT('Ctrl Pts',(-0.121943466508167,-0.153161073149159,
1.91242705983934));
#24102=CARTESIAN_POINT('Ctrl Pts',(-0.112140747371382,-0.160482594108263,
1.91312350401317));
#24103=CARTESIAN_POINT('Ctrl Pts',(-0.101716699622421,-0.166837864461046,
1.91381994818701));
#24104=CARTESIAN_POINT('Ctrl Pts',(-0.0913145299504756,-0.173179796320223,
1.91451493065809));
#24105=CARTESIAN_POINT('Ctrl Pts',(-0.0802943213494162,-0.178558987802671,
1.91520991312917));
#24106=CARTESIAN_POINT('Ctrl Pts',(-0.0688581541611845,-0.18286529087149,
1.91590489560026));
#24107=CARTESIAN_POINT('Ctrl Pts',(-0.0574235983776863,-0.187170987163839,
1.91659978014534));
#24108=CARTESIAN_POINT('Ctrl Pts',(-0.0455740023807954,-0.190403743891933,
1.91729466469043));
#24109=CARTESIAN_POINT('Ctrl Pts',(-0.0335317718966106,-0.19250137732877,
1.91798954923552));
#24110=CARTESIAN_POINT('Ctrl Pts',(-0.021490257254648,-0.194598886073211,
1.91868439247367));
#24111=CARTESIAN_POINT('Ctrl Pts',(-0.00925699821522074,-0.195561281543439,
1.91937923571182));
#24112=CARTESIAN_POINT('Ctrl Pts',(0.00293780523678198,-0.195377914054764,
1.92007407894997));
#24113=CARTESIAN_POINT('Ctrl Pts',(0.0151607146523066,-0.195194123950016,
1.92077052362751));
#24114=CARTESIAN_POINT('Ctrl Pts',(0.0273441174233028,-0.193859377124696,
1.92146696830506));
#24115=CARTESIAN_POINT('Ctrl Pts',(0.0392614908477917,-0.191414982006134,
1.9221634129826));
#24116=CARTESIAN_POINT('Ctrl Pts',(0.0431510759027313,-0.190617181821239,
1.92239071817083));
#24117=CARTESIAN_POINT('Ctrl Pts',(0.0470124198678937,-0.189701581600493,
1.92261802335905));
#24118=CARTESIAN_POINT('Ctrl Pts',(0.0508380046781814,-0.188670764243804,
1.92284532854727));
#24119=CARTESIAN_POINT('Ctrl Pts',(0.0625592780616349,-0.185512425677198,
1.92354177272111));
#24120=CARTESIAN_POINT('Ctrl Pts',(0.0740265955397715,-0.18124644378724,
1.92423821689495));
#24121=CARTESIAN_POINT('Ctrl Pts',(0.0850189987823538,-0.175934447582178,
1.92493466106878));
#24122=CARTESIAN_POINT('Ctrl Pts',(0.0959883310787419,-0.170633600238373,
1.92562964353987));
#24123=CARTESIAN_POINT('Ctrl Pts',(0.106483914527211,-0.164291406083945,
1.92632462601095));
#24124=CARTESIAN_POINT('Ctrl Pts',(0.116303619557301,-0.15701792279186,
1.92701960848203));
#24125=CARTESIAN_POINT('Ctrl Pts',(0.12612194094907,-0.149745464364593,
1.92771449302713));
#24126=CARTESIAN_POINT('Ctrl Pts',(0.135263842934809,-0.141542460680806,
1.92840937757222));
#24127=CARTESIAN_POINT('Ctrl Pts',(0.143556473677907,-0.132562056657116,
1.92910426211731));
#24128=CARTESIAN_POINT('Ctrl Pts',(0.151848611471193,-0.123582186467455,
1.92979910535546));
#24129=CARTESIAN_POINT('Ctrl Pts',(0.159291003765012,-0.113825669224495,
1.93049394859361));
#24130=CARTESIAN_POINT('Ctrl Pts',(0.165749871062098,-0.103480144196352,
1.93118879183176));
#24131=CARTESIAN_POINT('Ctrl Pts',(0.172223624428435,-0.0931107753276527,
1.9318852365093));
#24132=CARTESIAN_POINT('Ctrl Pts',(0.177708919031196,-0.0821504653279504,
1.93258168118685));
#24133=CARTESIAN_POINT('Ctrl Pts',(0.182117624742747,-0.0708119393750788,
1.9332781258644));
#24134=CARTESIAN_POINT('Ctrl Pts',(0.183556535418455,-0.0671112782042444,
1.93350543105262));
#24135=CARTESIAN_POINT('Ctrl Pts',(0.18488115592575,-0.0633704652588357,
1.93373273624084));
#24136=CARTESIAN_POINT('Ctrl Pts',(0.186089579564252,-0.0595972178679496,
1.93396004142906));
#24137=CARTESIAN_POINT('Ctrl Pts',(0.18979208899291,-0.0480363019802609,
1.93465648560289));
#24138=CARTESIAN_POINT('Ctrl Pts',(0.192426241229846,-0.0360881132630105,
1.93535292977673));
#24139=CARTESIAN_POINT('Ctrl Pts',(0.193923996943345,-0.023971721037874,
1.93604937395057));
#24140=CARTESIAN_POINT('Ctrl Pts',(0.195418609154853,-0.0118807587962363,
1.93674435642166));
#24141=CARTESIAN_POINT('Ctrl Pts',(0.195781378446354,0.000376855044065903,
1.93743933889274));
#24142=CARTESIAN_POINT('Ctrl Pts',(0.194995165671587,0.0125716094717537,
1.93813432136383));
#24143=CARTESIAN_POINT('Ctrl Pts',(0.194209063677554,0.0247646456065269,
1.93882920590892));
#24144=CARTESIAN_POINT('Ctrl Pts',(0.192274311263242,0.0368939644022763,
1.93952409045401));
#24145=CARTESIAN_POINT('Ctrl Pts',(0.189225847812887,0.0487312889168142,
1.9402189749991));
#24146=CARTESIAN_POINT('Ctrl Pts',(0.186177565576376,0.060567909769619,
1.94091381823725));
#24147=CARTESIAN_POINT('Ctrl Pts',(0.182015948038732,0.0721117293817821,
1.9416086614754));
#24148=CARTESIAN_POINT('Ctrl Pts',(0.176826104722049,0.0831485940279631,
1.94230350471355));
#24149=CARTESIAN_POINT('Ctrl Pts',(0.171624300118122,0.0942108958791325,
1.9429999493911));
#24150=CARTESIAN_POINT('Ctrl Pts',(0.165389969878783,0.104763145811543,
1.94369639406865));
#24151=CARTESIAN_POINT('Ctrl Pts',(0.158254055236014,0.114615941305548,
1.9443928387462));
#24152=CARTESIAN_POINT('Ctrl Pts',(0.155925039776173,0.117831690677135,
1.94462014393441));
#24153=CARTESIAN_POINT('Ctrl Pts',(0.153500312081673,0.120973186592694,
1.94484744912262));
#24154=CARTESIAN_POINT('Ctrl Pts',(0.15098532230701,0.12403464212811,1.94507475431084));
#24155=CARTESIAN_POINT('Ctrl Pts',(0.143279603006913,0.133414687026621,
1.94577119848467));
#24156=CARTESIAN_POINT('Ctrl Pts',(0.134669153546287,0.142107105085762,
1.9464676426585));
#24157=CARTESIAN_POINT('Ctrl Pts',(0.12530114024442,0.149935933829914,1.94716408683234));
#24158=CARTESIAN_POINT('Ctrl Pts',(0.115952788605793,0.157748331364014,
1.94785906930342));
#24159=CARTESIAN_POINT('Ctrl Pts',(0.105850646345792,0.164700123965514,
1.9485540517745));
#24160=CARTESIAN_POINT('Ctrl Pts',(0.0951782547854528,0.170652453296152,
1.94924903424558));
#24161=CARTESIAN_POINT('Ctrl Pts',(0.0845073670106115,0.176603943918196,
1.94994391879067));
#24162=CARTESIAN_POINT('Ctrl Pts',(0.0732671306095171,0.181555784687013,
1.95063880333576));
#24163=CARTESIAN_POINT('Ctrl Pts',(0.0616682909041917,0.185413542916789,
1.95133368788085));
#24164=CARTESIAN_POINT('Ctrl Pts',(0.0500701406840297,0.189271071824742,
1.95202853111899));
#24165=CARTESIAN_POINT('Ctrl Pts',(0.0381142689195054,0.192034396292956,
1.95272337435714));
#24166=CARTESIAN_POINT('Ctrl Pts',(0.0260267605822,0.193658895312343,1.95341821759529));
#24167=CARTESIAN_POINT('Ctrl Pts',(0.0139113935696971,0.195287138394548,
1.95411466227283));
#24168=CARTESIAN_POINT('Ctrl Pts',(0.0016646603449519,0.19577126388408,
1.95481110695038));
#24169=CARTESIAN_POINT('Ctrl Pts',(-0.0104832967402934,0.195118580584871,
1.95550755162792));
#24170=CARTESIAN_POINT('Ctrl Pts',(-0.0144481395495736,0.194905558208562,
1.95573485681615));
#24171=CARTESIAN_POINT('Ctrl Pts',(-0.0184024968294661,0.194571852522418,
1.95596216200438));
#24172=CARTESIAN_POINT('Ctrl Pts',(-0.022338550918238,0.194118904650921,
1.9561894671926));
#24173=CARTESIAN_POINT('Ctrl Pts',(-0.0343982929743568,0.192731110080032,
1.95688591136644));
#24174=CARTESIAN_POINT('Ctrl Pts',(-0.0463709023191962,0.190210277458485,
1.95758235554028));
#24175=CARTESIAN_POINT('Ctrl Pts',(-0.0580287304895212,0.186584636124667,
1.95827879971411));
#24176=CARTESIAN_POINT('Ctrl Pts',(-0.0696620911143581,0.182966604316652,
1.9589737821852));
#24177=CARTESIAN_POINT('Ctrl Pts',(-0.0809811319250672,0.178248552415478,
1.95966876465628));
#24178=CARTESIAN_POINT('Ctrl Pts',(-0.0917696541604555,0.172509392716079,
1.96036374712737));
#24179=CARTESIAN_POINT('Ctrl Pts',(-0.102556656247037,0.166771041688765,
1.96105863167246));
#24180=CARTESIAN_POINT('Ctrl Pts',(-0.112812494578821,0.160012238431858,
1.96175351621755));
#24181=CARTESIAN_POINT('Ctrl Pts',(-0.122343544844339,0.152358842982353,
1.96244840076264));
#24182=CARTESIAN_POINT('Ctrl Pts',(-0.131874028543028,0.144705902483758,
1.96314324400079));
#24183=CARTESIAN_POINT('Ctrl Pts',(-0.140679143598295,0.136159044544678,
1.96383808723894));
#24184=CARTESIAN_POINT('Ctrl Pts',(-0.14859879923003,0.126884029205385,
1.96453293047709));
#24185=CARTESIAN_POINT('Ctrl Pts',(-0.156536707681768,0.117587637281885,
1.96522937515464));
#24186=CARTESIAN_POINT('Ctrl Pts',(-0.163584563634262,0.107560445319938,
1.96592581983219));
#24187=CARTESIAN_POINT('Ctrl Pts',(-0.169623707588393,0.0969997825975262,
1.96662226450974));
#24188=CARTESIAN_POINT('Ctrl Pts',(-0.171594759701241,0.0935529999524722,
1.96684956969795));
#24189=CARTESIAN_POINT('Ctrl Pts',(-0.173458727505659,0.0900495837618375,
1.96707687488617));
#24190=CARTESIAN_POINT('Ctrl Pts',(-0.175212582516426,0.0864968839203154,
1.96730418007439));
#24191=CARTESIAN_POINT('Ctrl Pts',(-0.180970069375756,0.0748342193744243,
1.9680503686853));
#24192=CARTESIAN_POINT('Ctrl Pts',(-0.18557358731148,0.0625657075161415,
1.9687965572962));
#24193=CARTESIAN_POINT('Ctrl Pts',(-0.188913584232968,0.0499281252627537,
1.96954274590711));
#24194=CARTESIAN_POINT('Ctrl Pts',(-0.192235407018057,0.0373593086846153,
1.97028487423476));
#24195=CARTESIAN_POINT('Ctrl Pts',(-0.194307127941387,0.0244260431589578,
1.97102700256241));
#24196=CARTESIAN_POINT('Ctrl Pts',(-0.195068230692454,0.0113818001438891,
1.97176913089005));
#24197=CARTESIAN_POINT('Ctrl Pts',(-0.195288350830162,0.00760924700998056,
1.9719837633946));
#24198=CARTESIAN_POINT('Ctrl Pts',(-0.19539916387975,0.00382750994004229,
1.97219839589914));
#24199=CARTESIAN_POINT('Ctrl Pts',(-0.195399995284978,4.29258736808888E-5,
1.97241302840369));
#24200=CARTESIAN_POINT('',(-0.195381194231368,-0.000178768183475579,2.04241303078758));
#24201=CARTESIAN_POINT('Ctrl Pts',(-0.195087892673083,4.28153426326047E-5,
1.97241303078758));
#24202=CARTESIAN_POINT('Ctrl Pts',(-0.195018847371885,-0.0352009863002633,
1.97441498484377));
#24203=CARTESIAN_POINT('Ctrl Pts',(-0.169041111820685,-0.135763402236124,
1.98012184319391));
#24204=CARTESIAN_POINT('Ctrl Pts',(-0.00786427776343007,-0.230825175541495,
1.98953360583792));
#24205=CARTESIAN_POINT('Ctrl Pts',(0.189675009695224,-0.131778219845546,
2.00064831871973));
#24206=CARTESIAN_POINT('Ctrl Pts',(0.213576180559187,0.0879051968103242,
2.01176303160147));
#24207=CARTESIAN_POINT('Ctrl Pts',(0.041958891709634,0.227115741275293,
2.02287774448327));
#24208=CARTESIAN_POINT('Ctrl Pts',(-0.151099805097311,0.163964067429302,
2.03309441087863));
#24209=CARTESIAN_POINT('Ctrl Pts',(-0.194932378367354,0.0490481979593188,
2.03960617298007));
#24210=CARTESIAN_POINT('Ctrl Pts',(-0.195381194231368,-0.000178768183475579,
2.04241303078758));
#24211=CARTESIAN_POINT('',(-0.19541850016519,6.52473648468253E-5,2.11241303078758));
#24212=CARTESIAN_POINT('Ctrl Pts',(-0.195381194231368,-0.000178768183475579,
2.04241303078758));
#24213=CARTESIAN_POINT('Ctrl Pts',(-0.195524791640772,-0.0159288014993712,
2.04331107727399));
#24214=CARTESIAN_POINT('Ctrl Pts',(-0.186583102676833,-0.0964948299411469,
2.04791402805432));
#24215=CARTESIAN_POINT('Ctrl Pts',(-0.0751283049278637,-0.2183983661272,
2.0562218831286));
#24216=CARTESIAN_POINT('Ctrl Pts',(0.1427584110397,-0.181554797804677,2.06733659601036));
#24217=CARTESIAN_POINT('Ctrl Pts',(0.229956842554754,0.0214932336169986,
2.07845130889215));
#24218=CARTESIAN_POINT('Ctrl Pts',(0.106641126190405,0.204865269707955,
2.08956602177393));
#24219=CARTESIAN_POINT('Ctrl Pts',(-0.114299281647457,0.200693255350358,
2.10068073465569));
#24220=CARTESIAN_POINT('Ctrl Pts',(-0.193990126770331,0.0719485985092084,
2.10829640432692));
#24221=CARTESIAN_POINT('Ctrl Pts',(-0.195709494543343,0.00366078499822498,
2.11220716970421));
#24222=CARTESIAN_POINT('Ctrl Pts',(-0.195693853754418,6.53393013630089E-5,
2.11241303078758));
#24223=CARTESIAN_POINT('',(-0.195399951179357,0.000138127132403044,2.18241302809352));
#24224=CARTESIAN_POINT('Ctrl Pts',(-0.195399989108464,6.52411842770674E-5,
2.11241303078758));
#24225=CARTESIAN_POINT('Ctrl Pts',(-0.195404009954938,-0.0119773568441924,
2.11310358064536));
#24226=CARTESIAN_POINT('Ctrl Pts',(-0.194290431945964,-0.0240652292057775,
2.11379413050314));
#24227=CARTESIAN_POINT('Ctrl Pts',(-0.192060322024632,-0.0359721100825972,
2.11448468036092));
#24228=CARTESIAN_POINT('Ctrl Pts',(-0.189792835897659,-0.0480785479516255,
2.11518680369912));
#24229=CARTESIAN_POINT('Ctrl Pts',(-0.186370972563584,-0.0599969165405934,
2.11588892703731));
#24230=CARTESIAN_POINT('Ctrl Pts',(-0.181851010938754,-0.0714938446340174,
2.1165910503755));
#24231=CARTESIAN_POINT('Ctrl Pts',(-0.177414767965862,-0.0827778268218566,
2.11728016899723));
#24232=CARTESIAN_POINT('Ctrl Pts',(-0.171921179356806,-0.093655022735873,
2.11796928761896));
#24233=CARTESIAN_POINT('Ctrl Pts',(-0.165473021615391,-0.103922274404827,
2.11865840624069));
#24234=CARTESIAN_POINT('Ctrl Pts',(-0.158842334058695,-0.114480164055317,
2.11936703193712));
#24235=CARTESIAN_POINT('Ctrl Pts',(-0.151202616365141,-0.124392135141495,
2.12007565763354));
#24236=CARTESIAN_POINT('Ctrl Pts',(-0.142713033203458,-0.133469660050023,
2.12078428332997));
#24237=CARTESIAN_POINT('Ctrl Pts',(-0.134223450041775,-0.14254718495855,
2.1214929090264));
#24238=CARTESIAN_POINT('Ctrl Pts',(-0.124884795392853,-0.150789626260811,
2.12220153472282));
#24239=CARTESIAN_POINT('Ctrl Pts',(-0.114893963288023,-0.15805232424729,
2.12291016041925));
#24240=CARTESIAN_POINT('Ctrl Pts',(-0.10507487705743,-0.165190173932654,
2.12360660459381));
#24241=CARTESIAN_POINT('Ctrl Pts',(-0.0945533255298709,-0.171434765623136,
2.12430304876837));
#24242=CARTESIAN_POINT('Ctrl Pts',(-0.0835160360064994,-0.176652856557037,
2.12499949294294));
#24243=CARTESIAN_POINT('Ctrl Pts',(-0.0725019116369707,-0.181859995718858,
2.12569447541475));
#24244=CARTESIAN_POINT('Ctrl Pts',(-0.0609749495797634,-0.186044472344931,
2.12638945788656));
#24245=CARTESIAN_POINT('Ctrl Pts',(-0.0491477388324685,-0.189118110628399,
2.12708444035837));
#24246=CARTESIAN_POINT('Ctrl Pts',(-0.0373221945897685,-0.192191315823083,
2.12777932490418));
#24247=CARTESIAN_POINT('Ctrl Pts',(-0.025197320293739,-0.194153728862889,
2.12847420944999));
#24248=CARTESIAN_POINT('Ctrl Pts',(-0.0130008477400179,-0.194967017615906,
2.1291690939958));
#24249=CARTESIAN_POINT('Ctrl Pts',(-0.00080510019741124,-0.195780258023519,
2.12986393723466));
#24250=CARTESIAN_POINT('Ctrl Pts',(0.0114613615557843,-0.195444478168219,
2.13055878047352));
#24251=CARTESIAN_POINT('Ctrl Pts',(0.023568501124126,-0.193973415072174,
2.13125362371239));
#24252=CARTESIAN_POINT('Ctrl Pts',(0.0357035446123529,-0.192498961544679,
2.13195006839063));
#24253=CARTESIAN_POINT('Ctrl Pts',(0.0476776718778061,-0.189884171171409,
2.13264651306887));
#24254=CARTESIAN_POINT('Ctrl Pts',(0.0592699940457487,-0.186194059534178,
2.13334295774711));
#24255=CARTESIAN_POINT('Ctrl Pts',(0.0630534890067612,-0.184989683173448,
2.13357026293175));
#24256=CARTESIAN_POINT('Ctrl Pts',(0.0667964521463349,-0.183671150874965,
2.13379756811639));
#24257=CARTESIAN_POINT('Ctrl Pts',(0.0704916804535371,-0.182241825569314,
2.13402487330102));
#24258=CARTESIAN_POINT('Ctrl Pts',(0.081813552527267,-0.177862491759065,
2.13472131747394));
#24259=CARTESIAN_POINT('Ctrl Pts',(0.0927658372219972,-0.172408554535117,
2.13541776164686));
#24260=CARTESIAN_POINT('Ctrl Pts',(0.103135326315513,-0.165964648241102,
2.13611420581978));
#24261=CARTESIAN_POINT('Ctrl Pts',(0.11348305184025,-0.159534266470481,
2.13680918828995));
#24262=CARTESIAN_POINT('Ctrl Pts',(0.123249633878203,-0.152118433842278,
2.13750417076013));
#24263=CARTESIAN_POINT('Ctrl Pts',(0.132245705377629,-0.143847952398264,
2.1381991532303));
#24264=CARTESIAN_POINT('Ctrl Pts',(0.141240509292515,-0.135578636300082,
2.13889403777451));
#24265=CARTESIAN_POINT('Ctrl Pts',(0.149464343322348,-0.126455468272226,
2.13958892231871));
#24266=CARTESIAN_POINT('Ctrl Pts',(0.156761507579238,-0.116649002316713,
2.14028380686291));
#24267=CARTESIAN_POINT('Ctrl Pts',(0.164058238061282,-0.106843119299737,
2.14097865010019));
#24268=CARTESIAN_POINT('Ctrl Pts',(0.170427906774986,-0.0963547375420952,
2.14167349333747));
#24269=CARTESIAN_POINT('Ctrl Pts',(0.175757312676377,-0.0853845831563189,
2.14236833657474));
#24270=CARTESIAN_POINT('Ctrl Pts',(0.181099001522049,-0.074389145315392,
2.14306478125145));
#24271=CARTESIAN_POINT('Ctrl Pts',(0.185395317103463,-0.0629105337170144,
2.14376122592816));
#24272=CARTESIAN_POINT('Ctrl Pts',(0.188581103156866,-0.0511695957785429,
2.14445767060487));
#24273=CARTESIAN_POINT('Ctrl Pts',(0.18962087808345,-0.0473375955505419,
2.14468497579752));
#24274=CARTESIAN_POINT('Ctrl Pts',(0.190542759656903,-0.0434777463364903,
2.14491228099016));
#24275=CARTESIAN_POINT('Ctrl Pts',(0.191345667405416,-0.0395979237482983,
2.14513958618281));
#24276=CARTESIAN_POINT('Ctrl Pts',(0.193805709855286,-0.0277104705725173,
2.1458360303559));
#24277=CARTESIAN_POINT('Ctrl Pts',(0.195162451269964,-0.0155508149849334,
2.14653247452899));
#24278=CARTESIAN_POINT('Ctrl Pts',(0.195371384116943,-0.00334398986690795,
2.14722891870209));
#24279=CARTESIAN_POINT('Ctrl Pts',(0.195579878453941,0.00883721546595823,
2.14792390117241));
#24280=CARTESIAN_POINT('Ctrl Pts',(0.194645256331035,0.0210645283257843,
2.14861888364273));
#24281=CARTESIAN_POINT('Ctrl Pts',(0.192574728837452,0.0331079116402994,
2.14931386611306));
#24282=CARTESIAN_POINT('Ctrl Pts',(0.190504493090074,0.0451495979904483,
2.15000875065737));
#24283=CARTESIAN_POINT('Ctrl Pts',(0.187298772424921,0.057006536720609,
2.15070363520168));
#24284=CARTESIAN_POINT('Ctrl Pts',(0.18301643442899,0.0684554214719283,
2.15139851974599));
#24285=CARTESIAN_POINT('Ctrl Pts',(0.178734350993801,0.0799036256518854,
2.15209336298335));
#24286=CARTESIAN_POINT('Ctrl Pts',(0.173376109136668,0.0909430131191398,
2.15278820622072));
#24287=CARTESIAN_POINT('Ctrl Pts',(0.167048973136666,0.1013696235269,2.15348304945808));
#24288=CARTESIAN_POINT('Ctrl Pts',(0.160707254675002,0.111820264656703,
2.15417949413484));
#24289=CARTESIAN_POINT('Ctrl Pts',(0.153392693571326,0.121654594715726,
2.1548759388116));
#24290=CARTESIAN_POINT('Ctrl Pts',(0.145255513517713,0.130698109369284,
2.15557238348836));
#24291=CARTESIAN_POINT('Ctrl Pts',(0.14259970561691,0.133649726208252,2.15579968868043));
#24292=CARTESIAN_POINT('Ctrl Pts',(0.139856568384743,0.136517390700739,
2.1560269938725));
#24293=CARTESIAN_POINT('Ctrl Pts',(0.137032133007897,0.139295924288208,
2.15625429906457));
#24294=CARTESIAN_POINT('Ctrl Pts',(0.128378298230296,0.147809119805824,
2.15695074324326));
#24295=CARTESIAN_POINT('Ctrl Pts',(0.118897466433838,0.155542928834054,
2.15764718742195));
#24296=CARTESIAN_POINT('Ctrl Pts',(0.108754575230515,0.162337926457222,
2.15834363160064));
#24297=CARTESIAN_POINT('Ctrl Pts',(0.0986329720101885,0.169118662683814,
2.15903861407659));
#24298=CARTESIAN_POINT('Ctrl Pts',(0.0878527460907765,0.174963953922716,
2.15973359655254));
#24299=CARTESIAN_POINT('Ctrl Pts',(0.0766110853095108,0.179755115664892,
2.16042857902849));
#24300=CARTESIAN_POINT('Ctrl Pts',(0.0653710085270541,0.184545602311579,
2.16112346357839));
#24301=CARTESIAN_POINT('Ctrl Pts',(0.0536704122311272,0.188281869105566,
2.16181834812829));
#24302=CARTESIAN_POINT('Ctrl Pts',(0.0417288411143926,0.1908922832889,2.16251323267819));
#24303=CARTESIAN_POINT('Ctrl Pts',(0.02978797985669,0.193502542297839,2.16320807592113));
#24304=CARTESIAN_POINT('Ctrl Pts',(0.0176070334827736,0.194986920660723,
2.16390291916406));
#24305=CARTESIAN_POINT('Ctrl Pts',(0.00541553644085428,0.195324939434415,
2.164597762407));
#24306=CARTESIAN_POINT('Ctrl Pts',(-0.00680405894173796,0.195663737256539,
2.16529420708921));
#24307=CARTESIAN_POINT('Ctrl Pts',(-0.0190333768825485,0.194850941551038,
2.16599065177142));
#24308=CARTESIAN_POINT('Ctrl Pts',(-0.0310443361113374,0.192918141177563,
2.16668709645363));
#24309=CARTESIAN_POINT('Ctrl Pts',(-0.0349644652041019,0.192287315043677,
2.16691440161787));
#24310=CARTESIAN_POINT('Ctrl Pts',(-0.0388614139166113,0.191537589492705,
2.16714170678211));
#24311=CARTESIAN_POINT('Ctrl Pts',(-0.0427275606604851,0.190671223733432,
2.16736901194636));
#24312=CARTESIAN_POINT('Ctrl Pts',(-0.0545731135566909,0.188016750918818,
2.16806545611286));
#24313=CARTESIAN_POINT('Ctrl Pts',(-0.0662122844687849,0.184244792641138,
2.16876190027937));
#24314=CARTESIAN_POINT('Ctrl Pts',(-0.0774216828963899,0.179407477596367,
2.16945834444588));
#24315=CARTESIAN_POINT('Ctrl Pts',(-0.0886075549469531,0.17458031514795,
2.17015332690968));
#24316=CARTESIAN_POINT('Ctrl Pts',(-0.0993646193415472,0.168692508981423,
2.17084830937347));
#24317=CARTESIAN_POINT('Ctrl Pts',(-0.109486227241,0.161845376963731,2.17154329183727));
#24318=CARTESIAN_POINT('Ctrl Pts',(-0.119606408965187,0.154999209734482,
2.17223817637524));
#24319=CARTESIAN_POINT('Ctrl Pts',(-0.12909056190635,0.147194436732592,
2.17293306091322));
#24320=CARTESIAN_POINT('Ctrl Pts',(-0.137759446610311,0.138576675056161,
2.17362794545119));
#24321=CARTESIAN_POINT('Ctrl Pts',(-0.146427815999421,0.129959425655613,
2.17432278868231));
#24322=CARTESIAN_POINT('Ctrl Pts',(-0.1542804111314,0.120529919908332,2.17501763191344));
#24323=CARTESIAN_POINT('Ctrl Pts',(-0.161175554861648,0.110469907735273,
2.17571247514456));
#24324=CARTESIAN_POINT('Ctrl Pts',(-0.168086590171654,0.100386709753177,
2.17640891981534));
#24325=CARTESIAN_POINT('Ctrl Pts',(-0.174035327454208,0.089670862891376,
2.17710536448613));
#24326=CARTESIAN_POINT('Ctrl Pts',(-0.178924625021148,0.0785311311585511,
2.17780180915691));
#24327=CARTESIAN_POINT('Ctrl Pts',(-0.180520391237771,0.0748953517202774,
2.17802911438065));
#24328=CARTESIAN_POINT('Ctrl Pts',(-0.182003687820427,0.0712145723022263,
2.17825641960439));
#24329=CARTESIAN_POINT('Ctrl Pts',(-0.183372279963377,0.0674964216905826,
2.17848372482813));
#24330=CARTESIAN_POINT('Ctrl Pts',(-0.188182590555252,0.0544279123019244,
2.17928265439306));
#24331=CARTESIAN_POINT('Ctrl Pts',(-0.191600390049941,0.040820586561108,
2.180081583958));
#24332=CARTESIAN_POINT('Ctrl Pts',(-0.19353130983678,0.0269590821961754,
2.18088051352294));
#24333=CARTESIAN_POINT('Ctrl Pts',(-0.19476594629612,0.0180959907374373,
2.18139135171313));
#24334=CARTESIAN_POINT('Ctrl Pts',(-0.195393595265852,0.00912944670203462,
2.18190218990332));
#24335=CARTESIAN_POINT('Ctrl Pts',(-0.195399951179357,0.000138127132403044,
2.18241302809352));
#24336=CARTESIAN_POINT('',(-0.195399948757862,-0.000141511218596957,2.25241303346085));
#24337=CARTESIAN_POINT('Ctrl Pts',(-0.19518796491764,0.000137929913403057,
2.18241303078758));
#24338=CARTESIAN_POINT('Ctrl Pts',(-0.194913552398402,-0.0419735976389966,
2.18480816642835));
#24339=CARTESIAN_POINT('Ctrl Pts',(-0.16086256744259,-0.149629643335042,
2.19090820636306));
#24340=CARTESIAN_POINT('Ctrl Pts',(0.0165728994326759,-0.230363729251873,
2.20071315059169));
#24341=CARTESIAN_POINT('Ctrl Pts',(0.202538966804153,-0.110995839031369,
2.21182786347345));
#24342=CARTESIAN_POINT('Ctrl Pts',(0.203090589989405,0.109983263613663,
2.22294257635524));
#24343=CARTESIAN_POINT('Ctrl Pts',(0.0177228121885867,0.230278120197377,
2.23405728923701));
#24344=CARTESIAN_POINT('Ctrl Pts',(-0.160449819017681,0.150279904486619,
2.24388077404779));
#24345=CARTESIAN_POINT('Ctrl Pts',(-0.194911113219737,0.0422922816017406,
2.24999935456465));
#24346=CARTESIAN_POINT('Ctrl Pts',(-0.195195111391083,-0.000141315875587933,
2.25241303078758));
#24347=CARTESIAN_POINT('',(-0.195423887338554,-5.94508832628922E-5,2.32241303078758));
#24348=CARTESIAN_POINT('Ctrl Pts',(-0.195399948757862,-0.000141511218596957,
2.25241303346085));
#24349=CARTESIAN_POINT('Ctrl Pts',(-0.19538972200811,-0.0142626981980689,
2.25321542657059));
#24350=CARTESIAN_POINT('Ctrl Pts',(-0.193844609223536,-0.028321132308972,
2.25401781968034));
#24351=CARTESIAN_POINT('Ctrl Pts',(-0.190829150317375,-0.0420166084917452,
2.25482021279009));
#24352=CARTESIAN_POINT('Ctrl Pts',(-0.18899207191704,-0.0503601688786147,
2.25530904686025));
#24353=CARTESIAN_POINT('Ctrl Pts',(-0.186610260799985,-0.0585693700250536,
2.25579788093041));
#24354=CARTESIAN_POINT('Ctrl Pts',(-0.1837069757175,-0.0665800801496189,
2.25628671500057));
#24355=CARTESIAN_POINT('Ctrl Pts',(-0.179570644684268,-0.0779929961895826,
2.25698316039847));
#24356=CARTESIAN_POINT('Ctrl Pts',(-0.174352052153745,-0.0890593770579522,
2.25767960579638));
#24357=CARTESIAN_POINT('Ctrl Pts',(-0.168131256433172,-0.0995642536767232,
2.25837605119428));
#24358=CARTESIAN_POINT('Ctrl Pts',(-0.161923516865908,-0.110047082749524,
2.25907103489849));
#24359=CARTESIAN_POINT('Ctrl Pts',(-0.15471812658239,-0.119969962728062,
2.2597660186027));
#24360=CARTESIAN_POINT('Ctrl Pts',(-0.146641810605223,-0.129140773508687,
2.2604610023069));
#24361=CARTESIAN_POINT('Ctrl Pts',(-0.13856663267905,-0.138310292010708,
2.26115588807947));
#24362=CARTESIAN_POINT('Ctrl Pts',(-0.12962131595782,-0.146727265055829,
2.26185077385203));
#24363=CARTESIAN_POINT('Ctrl Pts',(-0.119973047942276,-0.154232382356755,
2.2625456596246));
#24364=CARTESIAN_POINT('Ctrl Pts',(-0.110325353488193,-0.161737053500295,
2.26324050408822));
#24365=CARTESIAN_POINT('Ctrl Pts',(-0.0999754983665426,-0.168329459918655,
2.26393534855185));
#24366=CARTESIAN_POINT('Ctrl Pts',(-0.089121743707153,-0.173892135528311,
2.26463019301547));
#24367=CARTESIAN_POINT('Ctrl Pts',(-0.0782429743078843,-0.179467631483348,
2.26532663889299));
#24368=CARTESIAN_POINT('Ctrl Pts',(-0.0668587953570758,-0.184008317362891,
2.26602308477051));
#24369=CARTESIAN_POINT('Ctrl Pts',(-0.0551886116770029,-0.187444330778941,
2.26671953064803));
#24370=CARTESIAN_POINT('Ctrl Pts',(-0.0513798132084584,-0.18856574266034,
2.26694682972613));
#24371=CARTESIAN_POINT('Ctrl Pts',(-0.0475406538048195,-0.1895698896982,
2.26717412880423));
#24372=CARTESIAN_POINT('Ctrl Pts',(-0.0436789835309181,-0.190455523410863,
2.26740142788233));
#24373=CARTESIAN_POINT('Ctrl Pts',(-0.0318468808551804,-0.193169092482813,
2.26809786901775));
#24374=CARTESIAN_POINT('Ctrl Pts',(-0.0197190546916775,-0.194785440763548,
2.26879431015317));
#24375=CARTESIAN_POINT('Ctrl Pts',(-0.00751953334359756,-0.19525526015525,
2.26949075128859));
#24376=CARTESIAN_POINT('Ctrl Pts',(0.00465438351031375,-0.195724093484669,
2.27018573072543));
#24377=CARTESIAN_POINT('Ctrl Pts',(0.0168988334777028,-0.195051066224396,
2.27088071016227));
#24378=CARTESIAN_POINT('Ctrl Pts',(0.0289836795020654,-0.193238470089477,
2.27157568959911));
#24379=CARTESIAN_POINT('Ctrl Pts',(0.0410668236085626,-0.191426129223821,
2.27227057116148));
#24380=CARTESIAN_POINT('Ctrl Pts',(0.0529895368640161,-0.188474622183162,
2.27296545272385));
#24381=CARTESIAN_POINT('Ctrl Pts',(0.0645273070894692,-0.184438029266693,
2.27366033428623));
#24382=CARTESIAN_POINT('Ctrl Pts',(0.0760643919002142,-0.180401676148737,
2.27435517456835));
#24383=CARTESIAN_POINT('Ctrl Pts',(0.08721576127461,-0.175280679575768,
2.27505001485047));
#24384=CARTESIAN_POINT('Ctrl Pts',(0.0977752101557561,-0.1691779190054,
2.27574485513259));
#24385=CARTESIAN_POINT('Ctrl Pts',(0.108358997437004,-0.163061092224744,
2.27644129694723));
#24386=CARTESIAN_POINT('Ctrl Pts',(0.11834741527388,-0.155958478066104,
2.27713773876187));
#24387=CARTESIAN_POINT('Ctrl Pts',(0.127562789698037,-0.148016535172441,
2.27783418057652));
#24388=CARTESIAN_POINT('Ctrl Pts',(0.130570707152647,-0.145424268428428,
2.27806150063905));
#24389=CARTESIAN_POINT('Ctrl Pts',(0.133496547523929,-0.1427428860611,2.27828882070159));
#24390=CARTESIAN_POINT('Ctrl Pts',(0.136335003486585,-0.139978308406385,
2.27851614076412));
#24391=CARTESIAN_POINT('Ctrl Pts',(0.145031250161049,-0.131508404503551,
2.27921258677698));
#24392=CARTESIAN_POINT('Ctrl Pts',(0.15296596216631,-0.122195029690922,
2.27990903278983));
#24393=CARTESIAN_POINT('Ctrl Pts',(0.159976224875834,-0.112199676802015,
2.28060547880269));
#24394=CARTESIAN_POINT('Ctrl Pts',(0.166971774010696,-0.102225302780391,
2.28130046307141));
#24395=CARTESIAN_POINT('Ctrl Pts',(0.173046166156125,-0.0915724586430868,
2.28199544734013));
#24396=CARTESIAN_POINT('Ctrl Pts',(0.178076528417178,-0.080435750925108,
2.28269043160885));
#24397=CARTESIAN_POINT('Ctrl Pts',(0.183106181259049,-0.0693006137886638,
2.2833853178657));
#24398=CARTESIAN_POINT('Ctrl Pts',(0.187091694573998,-0.0576825263938266,
2.28408020412256));
#24399=CARTESIAN_POINT('Ctrl Pts',(0.189956758562106,-0.0457994527978004,
2.28477509037942));
#24400=CARTESIAN_POINT('Ctrl Pts',(0.192821652041564,-0.0339170863995334,
2.28546993528149));
#24401=CARTESIAN_POINT('Ctrl Pts',(0.194566049299117,-0.0217706227331317,
2.28616478018355));
#24402=CARTESIAN_POINT('Ctrl Pts',(0.195164569092226,-0.00958910689510555,
2.28685962508562));
#24403=CARTESIAN_POINT('Ctrl Pts',(0.195764468234045,0.00262048246421898,
2.28755607132724));
#24404=CARTESIAN_POINT('Ctrl Pts',(0.195213239780637,0.0148644079464561,
2.28825251756887));
#24405=CARTESIAN_POINT('Ctrl Pts',(0.193537589456231,0.0269139641723655,
2.28894896381049));
#24406=CARTESIAN_POINT('Ctrl Pts',(0.192990713590533,0.030846533752276,
2.28917626042229));
#24407=CARTESIAN_POINT('Ctrl Pts',(0.192324478908695,0.0347584713101603,
2.28940355703409));
#24408=CARTESIAN_POINT('Ctrl Pts',(0.191540980908215,0.0386421095790456,
2.28963085364589));
#24409=CARTESIAN_POINT('Ctrl Pts',(0.189140292853597,0.0505418259725163,
2.29032730502224));
#24410=CARTESIAN_POINT('Ctrl Pts',(0.185617940255705,0.0622590833852615,
2.2910237563986));
#24411=CARTESIAN_POINT('Ctrl Pts',(0.181021268785419,0.073569424677084,
2.29172020777495));
#24412=CARTESIAN_POINT('Ctrl Pts',(0.176434244283268,0.0848560291187227,
2.29241519751884));
#24413=CARTESIAN_POINT('Ctrl Pts',(0.170777633329243,0.0957365812876027,
2.29311018726273));
#24414=CARTESIAN_POINT('Ctrl Pts',(0.164148317176213,0.106002311145642,
2.29380517700663));
#24415=CARTESIAN_POINT('Ctrl Pts',(0.157519935201171,0.11626659439612,2.29450006881521));
#24416=CARTESIAN_POINT('Ctrl Pts',(0.149919555733696,0.125915467828864,
2.29519496062379));
#24417=CARTESIAN_POINT('Ctrl Pts',(0.141488934767856,0.13476661804118,2.29588985243238));
#24418=CARTESIAN_POINT('Ctrl Pts',(0.133058814923699,0.143617242135276,
2.29658470293613));
#24419=CARTESIAN_POINT('Ctrl Pts',(0.123799174908022,0.151669621464244,
2.29727955343989));
#24420=CARTESIAN_POINT('Ctrl Pts',(0.113888698061204,0.158778224117553,
2.29797440394364));
#24421=CARTESIAN_POINT('Ctrl Pts',(0.103955382158895,0.165903208805044,
2.29867085575574));
#24422=CARTESIAN_POINT('Ctrl Pts',(0.0933689840818892,0.172079617408341,
2.29936730756783));
#24423=CARTESIAN_POINT('Ctrl Pts',(0.0823361470535406,0.177205865840772,
2.30006375937993));
#24424=CARTESIAN_POINT('Ctrl Pts',(0.0787358658303617,0.178878684530037,
2.30029102842917));
#24425=CARTESIAN_POINT('Ctrl Pts',(0.0750882063564142,0.180440056483083,
2.30051829747842));
#24426=CARTESIAN_POINT('Ctrl Pts',(0.071400744166959,0.181887585426836,
2.30074556652767));
#24427=CARTESIAN_POINT('Ctrl Pts',(0.0601012195165049,0.186323261819383,
2.30144198918702));
#24428=CARTESIAN_POINT('Ctrl Pts',(0.0483467618574154,0.189717665048775,
2.30213841184638));
#24429=CARTESIAN_POINT('Ctrl Pts',(0.0363516163698731,0.191988853810052,
2.30283483450573));
#24430=CARTESIAN_POINT('Ctrl Pts',(0.024381647087459,0.194255275650062,
2.30352979546713));
#24431=CARTESIAN_POINT('Ctrl Pts',(0.0121728306059993,0.195402927618314,
2.30422475642852));
#24432=CARTESIAN_POINT('Ctrl Pts',(-4.69041769829161E-5,0.195399994370517,
2.30491971738991));
#24433=CARTESIAN_POINT('Ctrl Pts',(-0.0122649228945991,0.195397061534648,
2.30561458075521));
#24434=CARTESIAN_POINT('Ctrl Pts',(-0.0244929824437572,0.194243818350495,
2.3063094441205));
#24435=CARTESIAN_POINT('Ctrl Pts',(-0.0365010469752692,0.191960500024638,
2.3070043074858));
#24436=CARTESIAN_POINT('Ctrl Pts',(-0.0485084005892147,0.189677316878861,
2.30769912971286));
#24437=CARTESIAN_POINT('Ctrl Pts',(-0.0602949296388099,0.186264381307076,
2.30839395193992));
#24438=CARTESIAN_POINT('Ctrl Pts',(-0.0716414773323995,0.181792900646949,
2.30908877416698));
#24439=CARTESIAN_POINT('Ctrl Pts',(-0.0830141870764818,0.17731110996954,
2.30978519846497));
#24440=CARTESIAN_POINT('Ctrl Pts',(-0.0939440996977907,0.17176628294015,
2.31048162276295));
#24441=CARTESIAN_POINT('Ctrl Pts',(-0.104233822067019,0.165276950411426,
2.31117804706094));
#24442=CARTESIAN_POINT('Ctrl Pts',(-0.107593833809719,0.1631579201095,2.31140545784378));
#24443=CARTESIAN_POINT('Ctrl Pts',(-0.110885816438744,0.160938522031444,
2.31163286862661));
#24444=CARTESIAN_POINT('Ctrl Pts',(-0.114103637106889,0.15862383174977,
2.31186027940945));
#24445=CARTESIAN_POINT('Ctrl Pts',(-0.12388277810694,0.151589355633677,
2.31255139378145));
#24446=CARTESIAN_POINT('Ctrl Pts',(-0.133046136579518,0.143620245172889,
2.31324250815345));
#24447=CARTESIAN_POINT('Ctrl Pts',(-0.141410229922725,0.13484920049152,
2.31393362252545));
#24448=CARTESIAN_POINT('Ctrl Pts',(-0.149961945465167,0.125881404934092,
2.31464023988062));
#24449=CARTESIAN_POINT('Ctrl Pts',(-0.157677242816501,0.116075733836457,
2.3153468572358));
#24450=CARTESIAN_POINT('Ctrl Pts',(-0.164396399278085,0.105617157244457,
2.31605347459098));
#24451=CARTESIAN_POINT('Ctrl Pts',(-0.170953214755027,0.0954112694582027,
2.31674301942257));
#24452=CARTESIAN_POINT('Ctrl Pts',(-0.176561081723516,0.0845845189451643,
2.31743256425415));
#24453=CARTESIAN_POINT('Ctrl Pts',(-0.181114728188128,0.0733390430353466,
2.31812210908574));
#24454=CARTESIAN_POINT('Ctrl Pts',(-0.185837491075197,0.0616759249854399,
2.31883726270271));
#24455=CARTESIAN_POINT('Ctrl Pts',(-0.189425605345656,0.049563234804578,
2.31955241631969));
#24456=CARTESIAN_POINT('Ctrl Pts',(-0.191817193500518,0.0372468022464341,
2.32026756993666));
#24457=CARTESIAN_POINT('Ctrl Pts',(-0.19420878165538,0.0249303696882902,
2.32098272355363));
#24458=CARTESIAN_POINT('Ctrl Pts',(-0.19540378473205,0.0124112548288328,
2.32169787717061));
#24459=CARTESIAN_POINT('Ctrl Pts',(-0.19539999095818,-5.94436136248776E-5,
2.32241303078758));
#24460=CARTESIAN_POINT('',(-0.195373072924931,0.000178337447204722,2.39241301734378));
#24461=CARTESIAN_POINT('Ctrl Pts',(-0.195697752751996,-5.95341972371984E-5,
2.32241303078758));
#24462=CARTESIAN_POINT('Ctrl Pts',(-0.195710914677712,-0.00333097164176583,
2.32260035128879));
#24463=CARTESIAN_POINT('Ctrl Pts',(-0.194154341293038,-0.0712935330070171,
2.32649257608402));
#24464=CARTESIAN_POINT('Ctrl Pts',(-0.115302964228223,-0.200121413881382,
2.33408970517291));
#24465=CARTESIAN_POINT('Ctrl Pts',(0.105622948018936,-0.205392642805891,
2.34520441805482));
#24466=CARTESIAN_POINT('Ctrl Pts',(0.229835338308407,-0.0226457751156926,
2.35631913093652));
#24467=CARTESIAN_POINT('Ctrl Pts',(0.143684619655393,0.180848806972626,
2.36743384381834));
#24468=CARTESIAN_POINT('Ctrl Pts',(-0.0740780534647926,0.218753590559664,
2.3785485567001));
#24469=CARTESIAN_POINT('Ctrl Pts',(-0.186300605867557,0.0971745928305562,
2.38687494787525));
#24470=CARTESIAN_POINT('Ctrl Pts',(-0.195509800817246,0.0162592722445891,
2.39149643475648));
#24471=CARTESIAN_POINT('Ctrl Pts',(-0.195373072924931,0.000178337447204722,
2.39241301734378));
#24472=CARTESIAN_POINT('',(-0.151810369570276,-0.123111383537865,2.39999996557186));
#24473=CARTESIAN_POINT('Ctrl Pts',(-0.195399918810391,0.000178126057700033,
2.39241303078758));
#24474=CARTESIAN_POINT('Ctrl Pts',(-0.195410720541781,-0.0116711084889103,
2.39308832752325));
#24475=CARTESIAN_POINT('Ctrl Pts',(-0.194339373404496,-0.0235537033023695,
2.39376362425893));
#24476=CARTESIAN_POINT('Ctrl Pts',(-0.192194137897985,-0.0352501540088856,
2.3944389209946));
#24477=CARTESIAN_POINT('Ctrl Pts',(-0.190050922889026,-0.0469355883724696,
2.39511358169969));
#24478=CARTESIAN_POINT('Ctrl Pts',(-0.186835972891341,-0.0584343092701696,
2.39578824240477));
#24479=CARTESIAN_POINT('Ctrl Pts',(-0.182609043029114,-0.0695348646650817,
2.39646290310986));
#24480=CARTESIAN_POINT('Ctrl Pts',(-0.178373466969652,-0.0806581262780969,
2.39713894383536));
#24481=CARTESIAN_POINT('Ctrl Pts',(-0.173122133999952,-0.0913807328435216,
2.39781498456087));
#24482=CARTESIAN_POINT('Ctrl Pts',(-0.166963196588413,-0.101510841711508,
2.39849102528638));
#24483=CARTESIAN_POINT('Ctrl Pts',(-0.162380916207106,-0.109047693610556,
2.39899400298309));
#24484=CARTESIAN_POINT('Ctrl Pts',(-0.157297305620373,-0.11625696509648,
2.3994969806798));
#24485=CARTESIAN_POINT('Ctrl Pts',(-0.151771747278466,-0.123071104358584,
2.39999995837652));
#24486=CARTESIAN_POINT('',(-0.190155688860645,0.0449663651403318,2.4));
#24487=CARTESIAN_POINT('Origin',(0.,0.,2.4));
#24488=CARTESIAN_POINT('',(-0.195465158332937,-7.38788922412424E-5,2.33258696921242));
#24489=CARTESIAN_POINT('Ctrl Pts',(-0.190155688860645,0.0449663651403318,
2.4));
#24490=CARTESIAN_POINT('Ctrl Pts',(-0.175202059751608,0.108202911730688,
2.39629509570607));
#24491=CARTESIAN_POINT('Ctrl Pts',(-0.0775128162224373,0.217492107202676,
2.38888528711823));
#24492=CARTESIAN_POINT('Ctrl Pts',(0.141144990674223,0.183006228893533,
2.37777057423644));
#24493=CARTESIAN_POINT('Ctrl Pts',(0.230080867601978,-0.0193251643494339,
2.36665586135468));
#24494=CARTESIAN_POINT('Ctrl Pts',(0.108644616799767,-0.203806378129402,
2.35554114847289));
#24495=CARTESIAN_POINT('Ctrl Pts',(-0.112383257382277,-0.20179584998626,
2.34442643559113));
#24496=CARTESIAN_POINT('Ctrl Pts',(-0.193667652393877,-0.0732104317508976,
2.3367750425043));
#24497=CARTESIAN_POINT('Ctrl Pts',(-0.195702355486801,-0.0042939273868865,
2.3328285537114));
#24498=CARTESIAN_POINT('Ctrl Pts',(-0.195681353759257,-7.39606064390219E-5,
2.33258696921242));
#24499=CARTESIAN_POINT('',(-0.195399955977075,-0.000131164618793305,2.26258696921762));
#24500=CARTESIAN_POINT('Ctrl Pts',(-0.195399986042856,-7.38542594287352E-5,
2.33258696921242));
#24501=CARTESIAN_POINT('Ctrl Pts',(-0.195404534495383,0.011960218888881,
2.33189704962616));
#24502=CARTESIAN_POINT('Ctrl Pts',(-0.194293060880465,0.024039361424141,
2.3312071300399));
#24503=CARTESIAN_POINT('Ctrl Pts',(-0.192066782359531,0.0359376002823843,
2.33051721045363));
#24504=CARTESIAN_POINT('Ctrl Pts',(-0.189829434182476,0.047895000387246,
2.32982386040146));
#24505=CARTESIAN_POINT('Ctrl Pts',(-0.186466168721113,0.0596687783725439,
2.32913051034929));
#24506=CARTESIAN_POINT('Ctrl Pts',(-0.182031165904908,0.0710338978185751,
2.32843716029712));
#24507=CARTESIAN_POINT('Ctrl Pts',(-0.177626922118394,0.0823201943053074,
2.32774861898481));
#24508=CARTESIAN_POINT('Ctrl Pts',(-0.17216610444674,0.0932026472019881,
2.3270600776725));
#24509=CARTESIAN_POINT('Ctrl Pts',(-0.165751051963725,0.103478252656868,
2.32637153636019));
#24510=CARTESIAN_POINT('Ctrl Pts',(-0.159268795847343,0.11386150462336,
2.32567578193809));
#24511=CARTESIAN_POINT('Ctrl Pts',(-0.151812660159517,0.123624316111712,
2.32498002751599));
#24512=CARTESIAN_POINT('Ctrl Pts',(-0.143532878472785,0.132587604237036,
2.32428427309388));
#24513=CARTESIAN_POINT('Ctrl Pts',(-0.135253096786052,0.14155089236236,
2.32358851867178));
#24514=CARTESIAN_POINT('Ctrl Pts',(-0.126150395337392,0.149714068944035,
2.32289276424968));
#24515=CARTESIAN_POINT('Ctrl Pts',(-0.116410373116421,0.156938793900347,
2.32219700982757));
#24516=CARTESIAN_POINT('Ctrl Pts',(-0.10666267899715,0.16416920953722,2.32150070738237));
#24517=CARTESIAN_POINT('Ctrl Pts',(-0.0962041275241309,0.170513681286887,
2.32080440493716));
#24518=CARTESIAN_POINT('Ctrl Pts',(-0.0852200357042007,0.175837156240013,
2.32010810249196));
#24519=CARTESIAN_POINT('Ctrl Pts',(-0.0742590544158008,0.181149430600703,
2.31941326506725));
#24520=CARTESIAN_POINT('Ctrl Pts',(-0.0627754752192831,0.185444526224622,
2.31871842764254));
#24521=CARTESIAN_POINT('Ctrl Pts',(-0.0509809272286206,0.188632195181284,
2.31802359021783));
#24522=CARTESIAN_POINT('Ctrl Pts',(-0.0391880861055844,0.191819402829132,
2.31732885334767));
#24523=CARTESIAN_POINT('Ctrl Pts',(-0.0270851978963677,0.193899229028121,
2.31663411647752));
#24524=CARTESIAN_POINT('Ctrl Pts',(-0.0148995281149728,0.194831116770271,
2.31593937960736));
#24525=CARTESIAN_POINT('Ctrl Pts',(-0.00271461230998617,0.195762946852778,
2.31524468572337));
#24526=CARTESIAN_POINT('Ctrl Pts',(0.00955219924219646,0.19554693927595,
2.31454999183938));
#24527=CARTESIAN_POINT('Ctrl Pts',(0.0216708253165105,0.194194581103854,
2.31385529795539));
#24528=CARTESIAN_POINT('Ctrl Pts',(0.033817392293072,0.192839104912664,
2.31315900237383));
#24529=CARTESIAN_POINT('Ctrl Pts',(0.0458142287108722,0.190342209310646,
2.31246270679227));
#24530=CARTESIAN_POINT('Ctrl Pts',(0.0574399014123331,0.186766746841458,
2.31176641121071));
#24531=CARTESIAN_POINT('Ctrl Pts',(0.0612473306827593,0.185595776282586,
2.3115383731224));
#24532=CARTESIAN_POINT('Ctrl Pts',(0.0650150862563916,0.184309516170192,
2.3113103350341));
#24533=CARTESIAN_POINT('Ctrl Pts',(0.0687358611679654,0.182911293772414,
2.31108229694579));
#24534=CARTESIAN_POINT('Ctrl Pts',(0.0801000235662201,0.178640778416109,
2.31038581249562));
#24535=CARTESIAN_POINT('Ctrl Pts',(0.0911048671551245,0.173292037415153,
2.30968932804546));
#24536=CARTESIAN_POINT('Ctrl Pts',(0.101536364443804,0.166947676520325,
2.30899284359529));
#24537=CARTESIAN_POINT('Ctrl Pts',(0.111945975994884,0.160616626372165,
2.30829782039996));
#24538=CARTESIAN_POINT('Ctrl Pts',(0.121783849507209,0.153294489116926,
2.30760279720464));
#24539=CARTESIAN_POINT('Ctrl Pts',(0.130859357472746,0.145110263461342,
2.30690777400931));
#24540=CARTESIAN_POINT('Ctrl Pts',(0.139933587031676,0.136927190663337,
2.30621284871729));
#24541=CARTESIAN_POINT('Ctrl Pts',(0.148244984148803,0.127882821814845,
2.30551792342527));
#24542=CARTESIAN_POINT('Ctrl Pts',(0.155636206910171,0.118146227610595,
2.30482299813326));
#24543=CARTESIAN_POINT('Ctrl Pts',(0.163026990914559,0.108410211389013,
2.30412811409332));
#24544=CARTESIAN_POINT('Ctrl Pts',(0.169497200848164,0.0979827649999601,
2.30343323005338));
#24545=CARTESIAN_POINT('Ctrl Pts',(0.174931702176024,0.0870635375676792,
2.30273834601344));
#24546=CARTESIAN_POINT('Ctrl Pts',(0.180378722645977,0.0761191561513398,
2.30204186120988));
#24547=CARTESIAN_POINT('Ctrl Pts',(0.184784939522097,0.0646815443369111,
2.30134537640632));
#24548=CARTESIAN_POINT('Ctrl Pts',(0.188083067286571,0.052970933539775,
2.30064889160276));
#24549=CARTESIAN_POINT('Ctrl Pts',(0.189158486447766,0.0491524595024168,
2.30042178908985));
#24550=CARTESIAN_POINT('Ctrl Pts',(0.190116494591209,0.0453050584863319,
2.30019468657693));
#24551=CARTESIAN_POINT('Ctrl Pts',(0.190955938265016,0.0414365737160732,
2.29996758406401));
#24552=CARTESIAN_POINT('Ctrl Pts',(0.193530279104264,0.0295730042583024,
2.29927112366776));
#24553=CARTESIAN_POINT('Ctrl Pts',(0.195003921748024,0.0174266432872976,
2.2985746632715));
#24554=CARTESIAN_POINT('Ctrl Pts',(0.19533020681641,0.00522209776415546,
2.29787820287524));
#24555=CARTESIAN_POINT('Ctrl Pts',(0.195655807402106,-0.00695684499329843,
2.2971832035176));
#24556=CARTESIAN_POINT('Ctrl Pts',(0.194838730104721,-0.0191928654653601,
2.29648820415997));
#24557=CARTESIAN_POINT('Ctrl Pts',(0.192883984062965,-0.0312558585228103,
2.29579320480233));
#24558=CARTESIAN_POINT('Ctrl Pts',(0.190929511434308,-0.0433171643123228,
2.29509830265523));
#24559=CARTESIAN_POINT('Ctrl Pts',(0.187837780341885,-0.0552046203101992,
2.29440340050814));
#24560=CARTESIAN_POINT('Ctrl Pts',(0.183665518511083,-0.0666943574079165,
2.29370849836105));
#24561=CARTESIAN_POINT('Ctrl Pts',(0.179493502089677,-0.078183418687684,
2.29301363708759));
#24562=CARTESIAN_POINT('Ctrl Pts',(0.174241405162099,-0.0892739935231876,
2.29231877581414));
#24563=CARTESIAN_POINT('Ctrl Pts',(0.168014535251855,-0.0997610943409465,
2.29162391454068));
#24564=CARTESIAN_POINT('Ctrl Pts',(0.161773311531892,-0.110272369399023,
2.29092745151439));
#24565=CARTESIAN_POINT('Ctrl Pts',(0.154553331620299,-0.120176673950064,
2.29023098848811));
#24566=CARTESIAN_POINT('Ctrl Pts',(0.146503142947681,-0.129298063042148,
2.28953452546182));
#24567=CARTESIAN_POINT('Ctrl Pts',(0.143876803212438,-0.132273877347549,
2.28930730736863));
#24568=CARTESIAN_POINT('Ctrl Pts',(0.141162400596626,-0.135166646046722,
2.28908008927543));
#24569=CARTESIAN_POINT('Ctrl Pts',(0.138365909076259,-0.13797113903096,
2.28885287118223));
#24570=CARTESIAN_POINT('Ctrl Pts',(0.129794658348867,-0.146566914257183,
2.28815644738391));
#24571=CARTESIAN_POINT('Ctrl Pts',(0.120388986389258,-0.154391364591959,
2.28746002358559));
#24572=CARTESIAN_POINT('Ctrl Pts',(0.110312271898818,-0.161283485417824,
2.28676359978727));
#24573=CARTESIAN_POINT('Ctrl Pts',(0.10025671438214,-0.16816113561245,2.28606863819373));
#24574=CARTESIAN_POINT('Ctrl Pts',(0.0895335842429653,-0.174109790576425,
2.28537367660018));
#24575=CARTESIAN_POINT('Ctrl Pts',(0.0783389032088239,-0.179008871970186,
2.28467871500663));
#24576=CARTESIAN_POINT('Ctrl Pts',(0.0671458062673354,-0.183907260124111,
2.28398385175296));
#24577=CARTESIAN_POINT('Ctrl Pts',(0.0554820734628567,-0.187755976720076,
2.2832889884993));
#24578=CARTESIAN_POINT('Ctrl Pts',(0.0435665370192763,-0.19048127690707,
2.28259412524562));
#24579=CARTESIAN_POINT('Ctrl Pts',(0.0316517134033498,-0.193206414057399,
2.28189930356102));
#24580=CARTESIAN_POINT('Ctrl Pts',(0.0194859757854752,-0.19480809900496,
2.28120448187642));
#24581=CARTESIAN_POINT('Ctrl Pts',(0.0072986392893096,-0.195263641942182,
2.28050966019182));
#24582=CARTESIAN_POINT('Ctrl Pts',(-0.00491678697174241,-0.195720234829407,
2.27981323705987));
#24583=CARTESIAN_POINT('Ctrl Pts',(-0.0171530344283273,-0.195025444127289,
2.27911681392791));
#24584=CARTESIAN_POINT('Ctrl Pts',(-0.0291817392893931,-0.19320865946444,
2.27842039079596));
#24585=CARTESIAN_POINT('Ctrl Pts',(-0.0331096067779737,-0.192615404455411,
2.27819297996413));
#24586=CARTESIAN_POINT('Ctrl Pts',(-0.0370154202602093,-0.191902920682419,
2.2779655691323));
#24587=CARTESIAN_POINT('Ctrl Pts',(-0.0408915258148231,-0.191073397197348,
2.27773815830047));
#24588=CARTESIAN_POINT('Ctrl Pts',(-0.0527621951405048,-0.188532960965564,
2.27704170699188));
#24589=CARTESIAN_POINT('Ctrl Pts',(-0.0644372291389193,-0.184873082766647,
2.27634525568329));
#24590=CARTESIAN_POINT('Ctrl Pts',(-0.0756927429004167,-0.180143744471495,
2.2756488043747));
#24591=CARTESIAN_POINT('Ctrl Pts',(-0.0869246354015522,-0.175424331350225,
2.274953814666));
#24592=CARTESIAN_POINT('Ctrl Pts',(-0.0977379270613595,-0.169640179971889,
2.27425882495731));
#24593=CARTESIAN_POINT('Ctrl Pts',(-0.107925001512165,-0.162890619891383,
2.27356383524861));
#24594=CARTESIAN_POINT('Ctrl Pts',(-0.118110641138565,-0.156142010469831,
2.27286894342751));
#24595=CARTESIAN_POINT('Ctrl Pts',(-0.127669484326053,-0.148428706780985,
2.2721740516064));
#24596=CARTESIAN_POINT('Ctrl Pts',(-0.13642089721442,-0.139894598906508,
2.2714791597853));
#24597=CARTESIAN_POINT('Ctrl Pts',(-0.145171790261192,-0.131360997965518,
2.27078430924138));
#24598=CARTESIAN_POINT('Ctrl Pts',(-0.15311473991902,-0.122007320184588,
2.27008945869746));
#24599=CARTESIAN_POINT('Ctrl Pts',(-0.160106325535196,-0.112013947897652,
2.26939460815353));
#24600=CARTESIAN_POINT('Ctrl Pts',(-0.167114023916195,-0.10199754494696,
2.26869815626136));
#24601=CARTESIAN_POINT('Ctrl Pts',(-0.173165532670347,-0.0913392586629627,
2.26800170436919));
#24602=CARTESIAN_POINT('Ctrl Pts',(-0.178161704725289,-0.0802469125224081,
2.26730525247702));
#24603=CARTESIAN_POINT('Ctrl Pts',(-0.179792075949294,-0.0766272129293224,
2.26707798345757));
#24604=CARTESIAN_POINT('Ctrl Pts',(-0.181310451134443,-0.0729614488210793,
2.26685071443813));
#24605=CARTESIAN_POINT('Ctrl Pts',(-0.1827145232587,-0.0692572233802802,
2.26662344541869));
#24606=CARTESIAN_POINT('Ctrl Pts',(-0.187610819374939,-0.0563398067275817,
2.26583091033589));
#24607=CARTESIAN_POINT('Ctrl Pts',(-0.19114228617701,-0.0428779645722903,
2.2650383752531));
#24608=CARTESIAN_POINT('Ctrl Pts',(-0.1932133790389,-0.029150474445028,
2.2642458401703));
#24609=CARTESIAN_POINT('Ctrl Pts',(-0.194658394266399,-0.0195727135274749,
2.26369288318608));
#24610=CARTESIAN_POINT('Ctrl Pts',(-0.195393421250955,-0.00986614656641785,
2.26313992620185));
#24611=CARTESIAN_POINT('Ctrl Pts',(-0.195399955977075,-0.000131164618793936,
2.26258696921762));
#24612=CARTESIAN_POINT('',(-0.195399944228081,0.000147633542831837,2.19258696921242));
#24613=CARTESIAN_POINT('Ctrl Pts',(-0.195399955977136,-0.000131164527281134,
2.26258696921242));
#24614=CARTESIAN_POINT('Ctrl Pts',(-0.195408209090474,0.0121637601469669,
2.26188860484918));
#24615=CARTESIAN_POINT('Ctrl Pts',(-0.194251688243831,0.0244657020173597,
2.26119024048593));
#24616=CARTESIAN_POINT('Ctrl Pts',(-0.191952657528546,0.0365422668663097,
2.26049187612269));
#24617=CARTESIAN_POINT('Ctrl Pts',(-0.189653287505934,0.0486206140607155,
2.25979340868985));
#24618=CARTESIAN_POINT('Ctrl Pts',(-0.18621126803752,0.06047267665518,2.25909494125702));
#24619=CARTESIAN_POINT('Ctrl Pts',(-0.181699758673365,0.0718773795991548,
2.25839647382419));
#24620=CARTESIAN_POINT('Ctrl Pts',(-0.177176507344299,0.0833117652082813,
2.25769618851193));
#24621=CARTESIAN_POINT('Ctrl Pts',(-0.171578588528802,0.0942956888981793,
2.25699590319966));
#24622=CARTESIAN_POINT('Ctrl Pts',(-0.165026426292338,0.104630008244192,
2.2562956178874));
#24623=CARTESIAN_POINT('Ctrl Pts',(-0.162572283489123,0.108500775562497,
2.25603332277057));
#24624=CARTESIAN_POINT('Ctrl Pts',(-0.159984704674147,0.112280704945645,
2.25577102765374));
#24625=CARTESIAN_POINT('Ctrl Pts',(-0.157271491326974,0.115960501964201,
2.25550873253691));
#24626=CARTESIAN_POINT('Ctrl Pts',(-0.150067415690632,0.12573103330693,
2.25481229122586));
#24627=CARTESIAN_POINT('Ctrl Pts',(-0.141923859667923,0.134862252170482,
2.2541158499148));
#24628=CARTESIAN_POINT('Ctrl Pts',(-0.132978573695544,0.143170733524344,
2.25341940860375));
#24629=CARTESIAN_POINT('Ctrl Pts',(-0.124052063191857,0.151461776013532,
2.25272442906955));
#24630=CARTESIAN_POINT('Ctrl Pts',(-0.114327747182382,0.158932863893428,
2.25202944953536));
#24631=CARTESIAN_POINT('Ctrl Pts',(-0.103981643917688,0.165435720834937,
2.25133447000116));
#24632=CARTESIAN_POINT('Ctrl Pts',(-0.0936369994124027,0.171937660899482,
2.25063958845632));
#24633=CARTESIAN_POINT('Ctrl Pts',(-0.0826714574396618,0.177471136713466,
2.24994470691147));
#24634=CARTESIAN_POINT('Ctrl Pts',(-0.0712905288926859,0.18193081237163,
2.24924982536663));
#24635=CARTESIAN_POINT('Ctrl Pts',(-0.0599102775329535,0.186390222670473,
2.24855498516858));
#24636=CARTESIAN_POINT('Ctrl Pts',(-0.0481155138222969,0.189775665035088,
2.24786014497053));
#24637=CARTESIAN_POINT('Ctrl Pts',(-0.0361296751148883,0.192030743830493,
2.24716530477248));
#24638=CARTESIAN_POINT('Ctrl Pts',(-0.0241162119893341,0.194291020029361,
2.24646886313821));
#24639=CARTESIAN_POINT('Ctrl Pts',(-0.0119116668126163,0.195415633644518,
2.24577242150395));
#24640=CARTESIAN_POINT('Ctrl Pts',(0.000253752594602635,0.195399835234375,
2.24507597986968));
#24641=CARTESIAN_POINT('Ctrl Pts',(0.00422457207697346,0.195394678598776,
2.24484865979816));
#24642=CARTESIAN_POINT('Ctrl Pts',(0.00819123791521547,0.19526843924573,
2.24462133972665));
#24643=CARTESIAN_POINT('Ctrl Pts',(0.0121458661306949,0.195022147295981,
2.24439401965513));
#24644=CARTESIAN_POINT('Ctrl Pts',(0.0242617453322618,0.194267577372112,
2.24369757428113));
#24645=CARTESIAN_POINT('Ctrl Pts',(0.0363499239593466,0.192376957475244,
2.24300112890712));
#24646=CARTESIAN_POINT('Ctrl Pts',(0.0481815872380622,0.189366561597398,
2.24230468353311));
#24647=CARTESIAN_POINT('Ctrl Pts',(0.0599884185091095,0.18636248386534,
2.24160969984175));
#24648=CARTESIAN_POINT('Ctrl Pts',(0.0715389444731538,0.182243436301947,
2.24091471615039));
#24649=CARTESIAN_POINT('Ctrl Pts',(0.0826131312729343,0.177076905725396,
2.24021973245903));
#24650=CARTESIAN_POINT('Ctrl Pts',(0.0936857578434941,0.171911103055293,
2.23952484668311));
#24651=CARTESIAN_POINT('Ctrl Pts',(0.10428136662625,0.165698438236002,2.23882996090718));
#24652=CARTESIAN_POINT('Ctrl Pts',(0.114200009660928,0.158554463177307,
2.23813507513126));
#24653=CARTESIAN_POINT('Ctrl Pts',(0.124118063195132,0.151410912710632,
2.23744023065489));
#24654=CARTESIAN_POINT('Ctrl Pts',(0.133358535866462,0.143336695417527,
2.23674538617851));
#24655=CARTESIAN_POINT('Ctrl Pts',(0.141752878559905,0.134488963933777,
2.23605054170214));
#24656=CARTESIAN_POINT('Ctrl Pts',(0.150166567929309,0.125620840836263,
2.2353540957983));
#24657=CARTESIAN_POINT('Ctrl Pts',(0.157729678906863,0.115976324109947,
2.23465764989447));
#24658=CARTESIAN_POINT('Ctrl Pts',(0.164313384223064,0.105746261234919,
2.23396120399063));
#24659=CARTESIAN_POINT('Ctrl Pts',(0.166462108342548,0.102407475279642,
2.23373390491821));
#24660=CARTESIAN_POINT('Ctrl Pts',(0.168506865290859,0.0990065310496776,
2.23350660584578));
#24661=CARTESIAN_POINT('Ctrl Pts',(0.170444246243508,0.0955506092208851,
2.23327930677336));
#24662=CARTESIAN_POINT('Ctrl Pts',(0.176380380824278,0.0849616659114767,
2.23258286249266));
#24663=CARTESIAN_POINT('Ctrl Pts',(0.181346987238524,0.0737799464835854,
2.23188641821197));
#24664=CARTESIAN_POINT('Ctrl Pts',(0.185233658322928,0.0622065255765414,
2.23118997393128));
#24665=CARTESIAN_POINT('Ctrl Pts',(0.189112172081714,0.0506573949067717,
2.23049499134432));
#24666=CARTESIAN_POINT('Ctrl Pts',(0.191914902566601,0.0387189925502746,
2.22980000875736));
#24667=CARTESIAN_POINT('Ctrl Pts',(0.193579233316941,0.0266127869345781,
2.22910502617041));
#24668=CARTESIAN_POINT('Ctrl Pts',(0.195243329583537,0.0145082869344427,
2.22841014149795));
#24669=CARTESIAN_POINT('Ctrl Pts',(0.195769179760362,0.00223689053688691,
2.2277152568255));
#24670=CARTESIAN_POINT('Ctrl Pts',(0.195145443797342,-0.00997074546552755,
2.22702037215304));
#24671=CARTESIAN_POINT('Ctrl Pts',(0.194521744905773,-0.0221776559128915,
2.22632552878073));
#24672=CARTESIAN_POINT('Ctrl Pts',(0.192748666911091,-0.0343199402350793,
2.22563068540842));
#24673=CARTESIAN_POINT('Ctrl Pts',(0.189866849548342,-0.046170763937663,
2.2249358420361));
#24674=CARTESIAN_POINT('Ctrl Pts',(0.186978390288739,-0.0580489009424982,
2.22423939721671));
#24675=CARTESIAN_POINT('Ctrl Pts',(0.182976360035834,-0.0696334011972714,
2.22354295239731));
#24676=CARTESIAN_POINT('Ctrl Pts',(0.177951249129385,-0.080712532690355,
2.22284650757792));
#24677=CARTESIAN_POINT('Ctrl Pts',(0.176311161354537,-0.0843285221592478,
2.2226192030158));
#24678=CARTESIAN_POINT('Ctrl Pts',(0.174562464071665,-0.0878908626194418,
2.22239189845369));
#24679=CARTESIAN_POINT('Ctrl Pts',(0.172709342296327,-0.0913927955780434,
2.22216459389158));
#24680=CARTESIAN_POINT('Ctrl Pts',(0.167031519007738,-0.102122450138284,
2.22146815011032));
#24681=CARTESIAN_POINT('Ctrl Pts',(0.160329895247707,-0.112358954932852,
2.22077170632906));
#24682=CARTESIAN_POINT('Ctrl Pts',(0.152713542682258,-0.121900508126234,
2.2200752625478));
#24683=CARTESIAN_POINT('Ctrl Pts',(0.145113175506104,-0.131422035271589,
2.21938028047998));
#24684=CARTESIAN_POINT('Ctrl Pts',(0.136602372643736,-0.140250781795649,
2.21868529841216));
#24685=CARTESIAN_POINT('Ctrl Pts',(0.127333256389287,-0.148214040553856,
2.21799031634435));
#24686=CARTESIAN_POINT('Ctrl Pts',(0.11806544631989,-0.1561761771458,2.217295432212));
#24687=CARTESIAN_POINT('Ctrl Pts',(0.108040168168097,-0.163272463345915,
2.21660054807964));
#24688=CARTESIAN_POINT('Ctrl Pts',(0.0974450702572235,-0.169368291845212,
2.21590566394729));
#24689=CARTESIAN_POINT('Ctrl Pts',(0.0868506022553824,-0.175463757929978,
2.2152108211278));
#24690=CARTESIAN_POINT('Ctrl Pts',(0.0756871541742055,-0.180558470837561,
2.2145159783083));
#24691=CARTESIAN_POINT('Ctrl Pts',(0.0641673502122027,-0.18456356944626,
2.21382113548881));
#24692=CARTESIAN_POINT('Ctrl Pts',(0.0526209959931669,-0.188577898802102,
2.213124691231));
#24693=CARTESIAN_POINT('Ctrl Pts',(0.040717494220899,-0.191497374290718,
2.21242824697319));
#24694=CARTESIAN_POINT('Ctrl Pts',(0.0286838127307998,-0.193283209015228,
2.21173180271538));
#24695=CARTESIAN_POINT('Ctrl Pts',(0.024756229384345,-0.193866074261352,
2.21150449548019));
#24696=CARTESIAN_POINT('Ctrl Pts',(0.0208148254210547,-0.194328590304711,
2.211277188245));
#24697=CARTESIAN_POINT('Ctrl Pts',(0.0168675490533827,-0.194670608436229,
2.21104988100981));
#24698=CARTESIAN_POINT('Ctrl Pts',(0.00477352840614477,-0.195718514374155,
2.21035343664169));
#24699=CARTESIAN_POINT('Ctrl Pts',(-0.00746132769261978,-0.195638797031868,
2.20965699227356));
#24700=CARTESIAN_POINT('Ctrl Pts',(-0.0196083179009098,-0.194413666878378,
2.20896054790544));
#24701=CARTESIAN_POINT('Ctrl Pts',(-0.0317298139764309,-0.193191108031051,
2.20826556523646));
#24702=CARTESIAN_POINT('Ctrl Pts',(-0.0437629401733625,-0.190827920682833,
2.20757058256749));
#24703=CARTESIAN_POINT('Ctrl Pts',(-0.0554800953712026,-0.187358263809212,
2.20687559989851));
#24704=CARTESIAN_POINT('Ctrl Pts',(-0.0671955996098305,-0.183889095813811,
2.2061807151533));
#24705=CARTESIAN_POINT('Ctrl Pts',(-0.0785943697721386,-0.17931397184433,
2.2054858304081));
#24706=CARTESIAN_POINT('Ctrl Pts',(-0.0894615514669536,-0.173717560451227,
2.20479094566289));
#24707=CARTESIAN_POINT('Ctrl Pts',(-0.100328087193093,-0.168121481720864,
2.20409610222313));
#24708=CARTESIAN_POINT('Ctrl Pts',(-0.110662330845803,-0.161504660815807,
2.20340125878337));
#24709=CARTESIAN_POINT('Ctrl Pts',(-0.120274320293943,-0.153997558025541,
2.20270641534361));
#24710=CARTESIAN_POINT('Ctrl Pts',(-0.129908462939838,-0.146473153267398,
2.20200997046596));
#24711=CARTESIAN_POINT('Ctrl Pts',(-0.138816378390958,-0.138054960174133,
2.20131352558831));
#24712=CARTESIAN_POINT('Ctrl Pts',(-0.146842398771829,-0.128912644542478,
2.20061708071065));
#24713=CARTESIAN_POINT('Ctrl Pts',(-0.14946191419064,-0.125928795059882,
2.20038977651645));
#24714=CARTESIAN_POINT('Ctrl Pts',(-0.151987809105506,-0.122868073272702,
2.20016247232224));
#24715=CARTESIAN_POINT('Ctrl Pts',(-0.154415648637008,-0.119737076363222,
2.19993516812803));
#24716=CARTESIAN_POINT('Ctrl Pts',(-0.161858322763002,-0.110138835052628,
2.19923835475837));
#24717=CARTESIAN_POINT('Ctrl Pts',(-0.168429868223669,-0.0998089199701452,
2.1985415413887));
#24718=CARTESIAN_POINT('Ctrl Pts',(-0.17399049677386,-0.088929562196074,
2.19784472801903));
#24719=CARTESIAN_POINT('Ctrl Pts',(-0.179538968532555,-0.0780739891583648,
2.19714943804097));
#24720=CARTESIAN_POINT('Ctrl Pts',(-0.18408044524445,-0.0666720904675441,
2.19645414806291));
#24721=CARTESIAN_POINT('Ctrl Pts',(-0.187519231564517,-0.0549335761939177,
2.19575885808484));
#24722=CARTESIAN_POINT('Ctrl Pts',(-0.190956001269814,-0.0432019457621682,
2.19506397584716));
#24723=CARTESIAN_POINT('Ctrl Pts',(-0.193291077571079,-0.0311349154882965,
2.19436909360947));
#24724=CARTESIAN_POINT('Ctrl Pts',(-0.194478068348997,-0.0189589274813421,
2.19367421137179));
#24725=CARTESIAN_POINT('Ctrl Pts',(-0.19509714035216,-0.0126085720900598,
2.19331179731867));
#24726=CARTESIAN_POINT('Ctrl Pts',(-0.195404761902858,-0.0062287858313775,
2.19294938326554));
#24727=CARTESIAN_POINT('Ctrl Pts',(-0.195399944228081,0.000147633542831837,
2.19258696921242));
#24728=CARTESIAN_POINT('',(-0.195424404543861,4.85723203800092E-5,2.12258697393042));
#24729=CARTESIAN_POINT('Ctrl Pts',(-0.19520943667287,0.00014891838008839,
2.19258688792652));
#24730=CARTESIAN_POINT('Ctrl Pts',(-0.195364193218957,0.02221674989384,
2.19133141036643));
#24731=CARTESIAN_POINT('Ctrl Pts',(-0.181722525948205,0.109220630806636,
2.1863710285124));
#24732=CARTESIAN_POINT('Ctrl Pts',(-0.0537908007947809,0.224607784190422,
2.17770574236448));
#24733=CARTESIAN_POINT('Ctrl Pts',(0.159546357810677,0.166994209782184,
2.1665910294827));
#24734=CARTESIAN_POINT('Ctrl Pts',(0.226826697041784,-0.0434943260391223,
2.15547631660093));
#24735=CARTESIAN_POINT('Ctrl Pts',(0.0864583809916583,-0.214165952291804,
2.14436160371914));
#24736=CARTESIAN_POINT('Ctrl Pts',(-0.130063871440271,-0.189125514256134,
2.13339850761495));
#24737=CARTESIAN_POINT('Ctrl Pts',(-0.195497536487265,-0.0620019008509531,
2.12614031580466));
#24738=CARTESIAN_POINT('Ctrl Pts',(-0.195705648609306,4.76931131101887E-5,
2.1225870282883));
#24739=CARTESIAN_POINT('',(-0.195399918942337,-0.000177981257815075,2.05258697083887));
#24740=CARTESIAN_POINT('Ctrl Pts',(-0.195399993943988,4.86486312413049E-5,
2.12258696921242));
#24741=CARTESIAN_POINT('Ctrl Pts',(-0.195399335882766,0.00269178895453019,
2.12243537212681));
#24742=CARTESIAN_POINT('Ctrl Pts',(-0.19534505029102,0.00533419421920633,
2.12228377504121));
#24743=CARTESIAN_POINT('Ctrl Pts',(-0.195237212099404,0.00797439725949685,
2.1221321779556));
#24744=CARTESIAN_POINT('Ctrl Pts',(-0.194741798352652,0.0201036147544585,
2.1214357337826));
#24745=CARTESIAN_POINT('Ctrl Pts',(-0.193110006278211,0.0322294230105758,
2.12073928960961));
#24746=CARTESIAN_POINT('Ctrl Pts',(-0.190353214459758,0.044122712346788,
2.12004284543661));
#24747=CARTESIAN_POINT('Ctrl Pts',(-0.187602208618729,0.0559910399491707,
2.11934786296639));
#24748=CARTESIAN_POINT('Ctrl Pts',(-0.183731012630555,0.0676269558939791,
2.11865288049617));
#24749=CARTESIAN_POINT('Ctrl Pts',(-0.178802393919666,0.0788090345620136,
2.11795789802595));
#24750=CARTESIAN_POINT('Ctrl Pts',(-0.173874469672371,0.089989537627024,
2.11726301348176));
#24751=CARTESIAN_POINT('Ctrl Pts',(-0.167889728949696,0.100715511684815,
2.11656812893756));
#24752=CARTESIAN_POINT('Ctrl Pts',(-0.160959422670306,0.110784584909823,
2.11587324439336));
#24753=CARTESIAN_POINT('Ctrl Pts',(-0.154029528358444,0.120853059585353,
2.11517840115613));
#24754=CARTESIAN_POINT('Ctrl Pts',(-0.146154698628647,0.130264004710846,
2.11448355791889));
#24755=CARTESIAN_POINT('Ctrl Pts',(-0.137488446820663,0.138845550850006,
2.11378871468165));
#24756=CARTESIAN_POINT('Ctrl Pts',(-0.128802221475821,0.147446875300703,
2.11309227000502));
#24757=CARTESIAN_POINT('Ctrl Pts',(-0.119321600162659,0.155214414894748,
2.11239582532839));
#24758=CARTESIAN_POINT('Ctrl Pts',(-0.109234632459035,0.162015292708866,
2.11169938065176));
#24759=CARTESIAN_POINT('Ctrl Pts',(-0.105942454036197,0.164234959099585,
2.11147207545912));
#24760=CARTESIAN_POINT('Ctrl Pts',(-0.102585905630071,0.166352005248618,
2.11124477026647));
#24761=CARTESIAN_POINT('Ctrl Pts',(-0.0991720940057208,0.168362869334424,
2.11101746507382));
#24762=CARTESIAN_POINT('Ctrl Pts',(-0.0887124595775196,0.174523989377577,
2.11032102089929));
#24763=CARTESIAN_POINT('Ctrl Pts',(-0.0776394604237156,0.179728474144029,
2.10962457672476));
#24764=CARTESIAN_POINT('Ctrl Pts',(-0.0661517651108088,0.18386164356038,
2.10892813255023));
#24765=CARTESIAN_POINT('Ctrl Pts',(-0.0546881802668738,0.187986138246923,
2.10823315007844));
#24766=CARTESIAN_POINT('Ctrl Pts',(-0.0428124172643358,0.191043416778346,
2.10753816760664));
#24767=CARTESIAN_POINT('Ctrl Pts',(-0.0307445553769932,0.192966142923237,
2.10684318513485));
#24768=CARTESIAN_POINT('Ctrl Pts',(-0.0186783939026507,0.194888598147847,
2.10614830058904));
#24769=CARTESIAN_POINT('Ctrl Pts',(-0.00642104348885204,0.195676635247699,
2.10545341604322));
#24770=CARTESIAN_POINT('Ctrl Pts',(0.00579713424226331,0.195313986274862,
2.10475853149741));
#24771=CARTESIAN_POINT('Ctrl Pts',(0.0180145856722261,0.194951358859445,
2.10406368825853));
#24772=CARTESIAN_POINT('Ctrl Pts',(0.0301919944621731,0.193438233877237,
2.10336884501965));
#24773=CARTESIAN_POINT('Ctrl Pts',(0.0421017092966201,0.190810392993419,
2.10267400178077));
#24774=CARTESIAN_POINT('Ctrl Pts',(0.0540388730367656,0.188176495595434,
2.10197755710249));
#24775=CARTESIAN_POINT('Ctrl Pts',(0.0657062704727992,0.184423005283176,
2.10128111242421));
#24776=CARTESIAN_POINT('Ctrl Pts',(0.0768902837219441,0.17963586576505,
2.10058466774594));
#24777=CARTESIAN_POINT('Ctrl Pts',(0.0805405150695424,0.178073442121128,
2.10035736256131));
#24778=CARTESIAN_POINT('Ctrl Pts',(0.084139430972879,0.176401286385976,
2.10013005737668));
#24779=CARTESIAN_POINT('Ctrl Pts',(0.0876801849670647,0.174623438186692,
2.09990275219204));
#24780=CARTESIAN_POINT('Ctrl Pts',(0.0985287606106727,0.169176259222985,
2.09920630801837));
#24781=CARTESIAN_POINT('Ctrl Pts',(0.108906182219367,0.162694971363788,
2.0985098638447));
#24782=CARTESIAN_POINT('Ctrl Pts',(0.118608362519414,0.155284308094743,
2.09781341967103));
#24783=CARTESIAN_POINT('Ctrl Pts',(0.128290179803753,0.14788919838664,2.09711843720011));
#24784=CARTESIAN_POINT('Ctrl Pts',(0.137298834480476,0.139569051785541,
2.09642345472919));
#24785=CARTESIAN_POINT('Ctrl Pts',(0.145458407148424,0.130472264446676,
2.09572847225827));
#24786=CARTESIAN_POINT('Ctrl Pts',(0.153616830097789,0.121376758883937,
2.09503358771335));
#24787=CARTESIAN_POINT('Ctrl Pts',(0.160925790405014,0.111505449927463,
2.09433870316842));
#24788=CARTESIAN_POINT('Ctrl Pts',(0.167246700449144,0.101043066010856,
2.0936438186235));
#24789=CARTESIAN_POINT('Ctrl Pts',(0.173567234751064,0.0905813040235646,
2.09294897538551));
#24790=CARTESIAN_POINT('Ctrl Pts',(0.17889940541699,0.0795293002373924,
2.09225413214753));
#24791=CARTESIAN_POINT('Ctrl Pts',(0.183149826708185,0.0680977310691177,
2.09155928890955));
#24792=CARTESIAN_POINT('Ctrl Pts',(0.187410044154482,0.0566398150008621,
2.09086284423216));
#24793=CARTESIAN_POINT('Ctrl Pts',(0.190583290771611,0.0448014300600738,
2.09016639955477));
#24794=CARTESIAN_POINT('Ctrl Pts',(0.192625937008771,0.0328086633603517,
2.08946995487739));
#24795=CARTESIAN_POINT('Ctrl Pts',(0.193292614641838,0.0288944714793296,
2.08924264968835));
#24796=CARTESIAN_POINT('Ctrl Pts',(0.193839268161496,0.024963889967138,
2.08901534449931));
#24797=CARTESIAN_POINT('Ctrl Pts',(0.194265579003178,0.0210248618202367,
2.08878803931026));
#24798=CARTESIAN_POINT('Ctrl Pts',(0.195571759927345,0.00895600754258418,
2.08809159513653));
#24799=CARTESIAN_POINT('Ctrl Pts',(0.195753586338233,-0.00327775356099378,
2.08739515096279));
#24800=CARTESIAN_POINT('Ctrl Pts',(0.194788384087688,-0.0154481527862555,
2.08669870678906));
#24801=CARTESIAN_POINT('Ctrl Pts',(0.193825207611557,-0.0275930086776184,
2.08600372431807));
#24802=CARTESIAN_POINT('Ctrl Pts',(0.191719774928313,-0.0396738965501845,
2.08530874184709));
#24803=CARTESIAN_POINT('Ctrl Pts',(0.188501372044258,-0.0514625372230354,
2.08461375937611));
#24804=CARTESIAN_POINT('Ctrl Pts',(0.185283422646914,-0.063249516826069,
2.08391887483113));
#24805=CARTESIAN_POINT('Ctrl Pts',(0.180953000178471,-0.0747434753502994,
2.08322399028614));
#24806=CARTESIAN_POINT('Ctrl Pts',(0.175590161150493,-0.0857277977504609,
2.08252910574116));
#24807=CARTESIAN_POINT('Ctrl Pts',(0.170227640912861,-0.0967114671949902,
2.08183426250312));
#24808=CARTESIAN_POINT('Ctrl Pts',(0.163833234204669,-0.107184785416907,
2.08113941926508));
#24809=CARTESIAN_POINT('Ctrl Pts',(0.156533310901506,-0.116955045116543,
2.08044457602704));
#24810=CARTESIAN_POINT('Ctrl Pts',(0.149216563105947,-0.126747822814408,
2.0797481313496));
#24811=CARTESIAN_POINT('Ctrl Pts',(0.140990708139181,-0.135833644857258,
2.07905168667216));
#24812=CARTESIAN_POINT('Ctrl Pts',(0.132022045483914,-0.144053252327892,
2.07835524199472));
#24813=CARTESIAN_POINT('Ctrl Pts',(0.129094858840565,-0.146735962797271,
2.07812793680598));
#24814=CARTESIAN_POINT('Ctrl Pts',(0.126088815573014,-0.149326716534686,
2.07790063161724));
#24815=CARTESIAN_POINT('Ctrl Pts',(0.123010416647546,-0.151820938596088,
2.0776733264285));
#24816=CARTESIAN_POINT('Ctrl Pts',(0.113578458633071,-0.159463027334912,
2.07697688225456));
#24817=CARTESIAN_POINT('Ctrl Pts',(0.10339823673046,-0.166249856763262,
2.07628043808062));
#24818=CARTESIAN_POINT('Ctrl Pts',(0.0926492469816981,-0.172038591698852,
2.07558399390668));
#24819=CARTESIAN_POINT('Ctrl Pts',(0.0819228173008448,-0.177815177190047,
2.0748890114355));
#24820=CARTESIAN_POINT('Ctrl Pts',(0.0706307170348819,-0.182597349316079,
2.07419402896431));
#24821=CARTESIAN_POINT('Ctrl Pts',(0.0589806277033746,-0.186285924201792,
2.07349904649312));
#24822=CARTESIAN_POINT('Ctrl Pts',(0.0473321799191163,-0.189973979351581,
2.07280416194792));
#24823=CARTESIAN_POINT('Ctrl Pts',(0.0353266628643546,-0.192568435295037,
2.07210927740272));
#24824=CARTESIAN_POINT('Ctrl Pts',(0.02318948939539,-0.194019090765783,
2.07141439285753));
#24825=CARTESIAN_POINT('Ctrl Pts',(0.0110530374124521,-0.195469660003301,
2.07071954961927));
#24826=CARTESIAN_POINT('Ctrl Pts',(-0.0012141827041594,-0.195776486369715,
2.07002470638101));
#24827=CARTESIAN_POINT('Ctrl Pts',(-0.0133817308529137,-0.194941245711061,
2.06932986314276));
#24828=CARTESIAN_POINT('Ctrl Pts',(-0.0255773221485489,-0.194104080032166,
2.0686334184651));
#24829=CARTESIAN_POINT('Ctrl Pts',(-0.037671914178917,-0.192119717205115,
2.06793697378745));
#24830=CARTESIAN_POINT('Ctrl Pts',(-0.0494415174021831,-0.189041520193236,
2.06724052910979));
#24831=CARTESIAN_POINT('Ctrl Pts',(-0.0532828732996088,-0.188036860136247,
2.0670132239221));
#24832=CARTESIAN_POINT('Ctrl Pts',(-0.057089728982391,-0.186916078838091,
2.0667859187344));
#24833=CARTESIAN_POINT('Ctrl Pts',(-0.0608547152675041,-0.185682157542697,
2.06655861354671));
#24834=CARTESIAN_POINT('Ctrl Pts',(-0.0723903198409249,-0.181901525407417,
2.06586216937291));
#24835=CARTESIAN_POINT('Ctrl Pts',(-0.083613098991688,-0.177028415543164,
2.0651657251991));
#24836=CARTESIAN_POINT('Ctrl Pts',(-0.0943057062615288,-0.171136184854385,
2.0644692810253));
#24837=CARTESIAN_POINT('Ctrl Pts',(-0.104975871799426,-0.165256320827762,
2.06377429855425));
#24838=CARTESIAN_POINT('Ctrl Pts',(-0.115117278778348,-0.158361934481534,
2.06307931608319));
#24839=CARTESIAN_POINT('Ctrl Pts',(-0.124533972353925,-0.15057373519227,
2.06238433361214));
#24840=CARTESIAN_POINT('Ctrl Pts',(-0.133949339077209,-0.142786633293507,
2.06168944906708));
#24841=CARTESIAN_POINT('Ctrl Pts',(-0.142639491963759,-0.134106490198566,
2.06099456452202));
#24842=CARTESIAN_POINT('Ctrl Pts',(-0.15044001616525,-0.12469547520339,
2.06029967997696));
#24843=CARTESIAN_POINT('Ctrl Pts',(-0.158240076669868,-0.115285019639621,
2.05960483673885));
#24844=CARTESIAN_POINT('Ctrl Pts',(-0.16515007519435,-0.10514446974595,
2.05890999350073));
#24845=CARTESIAN_POINT('Ctrl Pts',(-0.171046457958986,-0.0944683503597094,
2.05821515026261));
#24846=CARTESIAN_POINT('Ctrl Pts',(-0.1769564304071,-0.0837676251958226,
2.0575187055851));
#24847=CARTESIAN_POINT('Ctrl Pts',(-0.181847756999623,-0.0725296638005962,
2.05682226090758));
#24848=CARTESIAN_POINT('Ctrl Pts',(-0.185643809514086,-0.0609715998568009,
2.05612581623006));
#24849=CARTESIAN_POINT('Ctrl Pts',(-0.186882762814667,-0.0571992860078933,
2.05589851104169));
#24850=CARTESIAN_POINT('Ctrl Pts',(-0.188005442306769,-0.0533929896767407,
2.05567120585331));
#24851=CARTESIAN_POINT('Ctrl Pts',(-0.189010356714131,-0.0495605191134747,
2.05544390066494));
#24852=CARTESIAN_POINT('Ctrl Pts',(-0.192954623393621,-0.0345181574634848,
2.05455173286038));
#24853=CARTESIAN_POINT('Ctrl Pts',(-0.195103729759499,-0.0189863514340268,
2.05365956505583));
#24854=CARTESIAN_POINT('Ctrl Pts',(-0.195371401502571,-0.00334297396360765,
2.05276739725128));
#24855=CARTESIAN_POINT('Ctrl Pts',(-0.195389445586527,-0.00228843449970702,
2.05270725511381));
#24856=CARTESIAN_POINT('Ctrl Pts',(-0.195398957610215,-0.00123339698559899,
2.05264711297634));
#24857=CARTESIAN_POINT('Ctrl Pts',(-0.195399918942337,-0.000177981257815075,
2.05258697083887));
#24858=CARTESIAN_POINT('',(-0.195095239123403,5.78821923055833E-5,1.98258696921242));
#24859=CARTESIAN_POINT('Ctrl Pts',(-0.195352761517788,-0.000177909769055379,
2.05258696921242));
#24860=CARTESIAN_POINT('Ctrl Pts',(-0.194920193265683,0.0481152823703308,
2.04983437540267));
#24861=CARTESIAN_POINT('Ctrl Pts',(-0.152459071887738,0.162089108104644,
2.043376877299));
#24862=CARTESIAN_POINT('Ctrl Pts',(0.0386358748098384,0.227704580377005,
2.03321447490137));
#24863=CARTESIAN_POINT('Ctrl Pts',(0.212268936067669,0.0910165123910808,
2.02209976201962));
#24864=CARTESIAN_POINT('Ctrl Pts',(0.191580255470213,-0.128992683750082,
2.01098504913783));
#24865=CARTESIAN_POINT('Ctrl Pts',(-0.00449070026177847,-0.230915439843693,
1.99987033625606));
#24866=CARTESIAN_POINT('Ctrl Pts',(-0.167976517319539,-0.137684430050128,
1.99040430961426));
#24867=CARTESIAN_POINT('Ctrl Pts',(-0.194999162430299,-0.0361378162802388,
1.98464318726638));
#24868=CARTESIAN_POINT('Ctrl Pts',(-0.195095239123403,5.78821923055833E-5,
1.98258696921242));
#24869=CARTESIAN_POINT('',(-0.195399944102376,0.000147799825339807,1.91258696921242));
#24870=CARTESIAN_POINT('Ctrl Pts',(-0.195095239123403,5.78821923055833E-5,
1.98258696921242));
#24871=CARTESIAN_POINT('Ctrl Pts',(-0.19517227391142,0.0290797798957806,
1.98093828297245));
#24872=CARTESIAN_POINT('Ctrl Pts',(-0.175488771239349,0.123219939451178,
1.97558469243856));
#24873=CARTESIAN_POINT('Ctrl Pts',(-0.0297534949941362,0.229034574426429,
1.96652619761072));
#24874=CARTESIAN_POINT('Ctrl Pts',(0.176300576512053,0.149198570598455,
1.95541148472896));
#24875=CARTESIAN_POINT('Ctrl Pts',(0.220960165374942,-0.0672213661311054,
1.94429677184717));
#24876=CARTESIAN_POINT('Ctrl Pts',(0.0633416206041068,-0.222103457529017,
1.93318205896541));
#24877=CARTESIAN_POINT('Ctrl Pts',(-0.14169482387435,-0.176035287593829,
1.92261215264593));
#24878=CARTESIAN_POINT('Ctrl Pts',(-0.19509928885621,-0.0551416107203375,
1.9157471506204));
#24879=CARTESIAN_POINT('Ctrl Pts',(-0.195564927186827,0.000146460652338079,
1.91258705288877));
#24880=CARTESIAN_POINT('',(-0.195399942226119,-0.000150259872500694,1.84258696921242));
#24881=CARTESIAN_POINT('Ctrl Pts',(-0.195399944102376,0.000147799825339807,
1.91258696921242));
#24882=CARTESIAN_POINT('Ctrl Pts',(-0.195392740812671,0.009670966733785,
1.91204219054223));
#24883=CARTESIAN_POINT('Ctrl Pts',(-0.194689255056053,0.0191682791699718,
1.91149741187204));
#24884=CARTESIAN_POINT('Ctrl Pts',(-0.193301244059132,0.0285620210277918,
1.91095263320185));
#24885=CARTESIAN_POINT('Ctrl Pts',(-0.191526813038009,0.0405709654770123,
1.91025618902801));
#24886=CARTESIAN_POINT('Ctrl Pts',(-0.188622727228528,0.0524564295926097,
1.90955974485417));
#24887=CARTESIAN_POINT('Ctrl Pts',(-0.184624513351351,0.0639917890809184,
1.90886330068033));
#24888=CARTESIAN_POINT('Ctrl Pts',(-0.180634690958291,0.0755029380620095,
1.90816831820924));
#24889=CARTESIAN_POINT('Ctrl Pts',(-0.175555511827247,0.0866645973460532,
1.90747333573815));
#24890=CARTESIAN_POINT('Ctrl Pts',(-0.169472791726541,0.0972632143434115,
1.90677835326706));
#24891=CARTESIAN_POINT('Ctrl Pts',(-0.163390928707041,0.107860337950431,
1.90608346872197));
#24892=CARTESIAN_POINT('Ctrl Pts',(-0.156306200671082,0.117893795480693,
1.90538858417687));
#24893=CARTESIAN_POINT('Ctrl Pts',(-0.148350621826422,0.127174105083204,
1.90469369963178));
#24894=CARTESIAN_POINT('Ctrl Pts',(-0.140395515895752,0.136453863024004,
1.90399885639362));
#24895=CARTESIAN_POINT('Ctrl Pts',(-0.131570252208174,0.144979914432134,
1.90330401315547));
#24896=CARTESIAN_POINT('Ctrl Pts',(-0.122045647308596,0.152597575252773,
1.90260916991731));
#24897=CARTESIAN_POINT('Ctrl Pts',(-0.112499090583478,0.160232792871109,
1.90191272523976));
#24898=CARTESIAN_POINT('Ctrl Pts',(-0.102250698898779,0.166954944315969,
1.90121628056221));
#24899=CARTESIAN_POINT('Ctrl Pts',(-0.0915015109978395,0.172651769423636,
1.90051983588465));
#24900=CARTESIAN_POINT('Ctrl Pts',(-0.0879931976206115,0.174511095720389,
1.90029253069646));
#24901=CARTESIAN_POINT('Ctrl Pts',(-0.0844317194096779,0.176261573920934,
1.90006522550827));
#24902=CARTESIAN_POINT('Ctrl Pts',(-0.0808245197407886,0.177900413177347,
1.89983792032007));
#24903=CARTESIAN_POINT('Ctrl Pts',(-0.0697723602489291,0.182921680228243,
1.89914147614624));
#24904=CARTESIAN_POINT('Ctrl Pts',(-0.058211365925296,0.186926849622628,
1.8984450319724));
#24905=CARTESIAN_POINT('Ctrl Pts',(-0.0463512120321626,0.189822878344918,
1.89774858779857));
#24906=CARTESIAN_POINT('Ctrl Pts',(-0.0345159503274129,0.192712828858344,
1.89705360532749));
#24907=CARTESIAN_POINT('Ctrl Pts',(-0.022383599759184,0.194497981038102,
1.89635862285641));
#24908=CARTESIAN_POINT('Ctrl Pts',(-0.0101801232035018,0.195134633244746,
1.89566364038532));
#24909=CARTESIAN_POINT('Ctrl Pts',(0.00202163383028259,0.195771195744378,
1.89496875584024));
#24910=CARTESIAN_POINT('Ctrl Pts',(0.0142936261900098,0.195259487942096,
1.89427387129515));
#24911=CARTESIAN_POINT('Ctrl Pts',(0.0264050630220646,0.193607677138074,
1.89357898675006));
#24912=CARTESIAN_POINT('Ctrl Pts',(0.038515779897971,0.191955964524826,
1.89288414351191));
#24913=CARTESIAN_POINT('Ctrl Pts',(0.0504650960812098,0.189164428295551,
1.89218930027376));
#24914=CARTESIAN_POINT('Ctrl Pts',(0.0620304163469142,0.185292707486907,
1.89149445703562));
#24915=CARTESIAN_POINT('Ctrl Pts',(0.0736223917752728,0.181412063332819,
1.89079801235807));
#24916=CARTESIAN_POINT('Ctrl Pts',(0.0848277951488816,0.176446603897648,
1.89010156768052));
#24917=CARTESIAN_POINT('Ctrl Pts',(0.0954432871181529,0.170504366349023,
1.88940512300298));
#24918=CARTESIAN_POINT('Ctrl Pts',(0.098907964899463,0.168564942489481,
1.88917781781475));
#24919=CARTESIAN_POINT('Ctrl Pts',(0.102310018312978,0.166521823904143,
1.88895051262652));
#24920=CARTESIAN_POINT('Ctrl Pts',(0.105643066130638,0.164379751120744,
1.88872320743829));
#24921=CARTESIAN_POINT('Ctrl Pts',(0.115855247171571,0.157816618437492,
1.88802676326446));
#24922=CARTESIAN_POINT('Ctrl Pts',(0.125489629894986,0.150274958065372,
1.88733031909062));
#24923=CARTESIAN_POINT('Ctrl Pts',(0.134354337858408,0.141880484558761,
1.88663387491679));
#24924=CARTESIAN_POINT('Ctrl Pts',(0.143200440499962,0.133503629442078,
1.8859388924457));
#24925=CARTESIAN_POINT('Ctrl Pts',(0.151279393928429,0.124278055740848,
1.88524390997462));
#24926=CARTESIAN_POINT('Ctrl Pts',(0.158431946028575,0.114369919461363,
1.88454892750353));
#24927=CARTESIAN_POINT('Ctrl Pts',(0.165583490303622,0.104463179280541,
1.88385404295844));
#24928=CARTESIAN_POINT('Ctrl Pts',(0.171808343237217,0.0938747494012774,
1.88315915841336));
#24929=CARTESIAN_POINT('Ctrl Pts',(0.17698821497375,0.0828029695144176,
1.88246427386827));
#24930=CARTESIAN_POINT('Ctrl Pts',(0.18216777879632,0.071731847782006,1.88176943063012));
#24931=CARTESIAN_POINT('Ctrl Pts',(0.186302137850502,0.0601782376545026,
1.88107458739197));
#24932=CARTESIAN_POINT('Ctrl Pts',(0.189320693181421,0.0483615046633797,
1.88037974415382));
#24933=CARTESIAN_POINT('Ctrl Pts',(0.192346205525331,0.0365175370663244,
1.87968329947627));
#24934=CARTESIAN_POINT('Ctrl Pts',(0.194250626450532,0.0244100999672413,
1.87898685479872));
#24935=CARTESIAN_POINT('Ctrl Pts',(0.195014463147026,0.0122686251665398,
1.87829041012118));
#24936=CARTESIAN_POINT('Ctrl Pts',(0.195263763701203,0.0083058980414455,
1.87806310493295));
#24937=CARTESIAN_POINT('Ctrl Pts',(0.195391980206155,0.00433955696823603,
1.87783579974473));
#24938=CARTESIAN_POINT('Ctrl Pts',(0.195399635281082,0.000377534130968309,
1.87760849455651));
#24939=CARTESIAN_POINT('Ctrl Pts',(0.195423089793383,-0.0117617740089863,
1.87691205038268));
#24940=CARTESIAN_POINT('Ctrl Pts',(0.194311058701514,-0.0239462460320362,
1.87621560620884));
#24941=CARTESIAN_POINT('Ctrl Pts',(0.192065117802532,-0.0359464952881283,
1.87551916203501));
#24942=CARTESIAN_POINT('Ctrl Pts',(0.189823890702752,-0.0479215583225406,
1.87482417956392));
#24943=CARTESIAN_POINT('Ctrl Pts',(0.186453563582058,-0.0597123001870613,
1.87412919709284));
#24944=CARTESIAN_POINT('Ctrl Pts',(0.182007382543185,-0.0710948148586,1.87343421462176));
#24945=CARTESIAN_POINT('Ctrl Pts',(0.177561827990185,-0.082475725685272,
1.87273933007667));
#24946=CARTESIAN_POINT('Ctrl Pts',(0.172040995646972,-0.0934476923089527,
1.87204444553158));
#24947=CARTESIAN_POINT('Ctrl Pts',(0.165547385184692,-0.103803772852971,
1.87134956098649));
#24948=CARTESIAN_POINT('Ctrl Pts',(0.159054160730682,-0.114159237786806,
1.87065471774834));
#24949=CARTESIAN_POINT('Ctrl Pts',(0.15158876084847,-0.123898161565435,
1.86995987451019));
#24950=CARTESIAN_POINT('Ctrl Pts',(0.14329721271442,-0.132842270487515,
1.86926503127204));
#24951=CARTESIAN_POINT('Ctrl Pts',(0.134986554641424,-0.141806993337497,
1.86856858659449));
#24952=CARTESIAN_POINT('Ctrl Pts',(0.125846589687305,-0.149972646575667,
1.86787214191694));
#24953=CARTESIAN_POINT('Ctrl Pts',(0.116059516287823,-0.157198437266522,
1.86717569723939));
#24954=CARTESIAN_POINT('Ctrl Pts',(0.112865217253207,-0.159556786416059,
1.86694839205118));
#24955=CARTESIAN_POINT('Ctrl Pts',(0.10960222096313,-0.161815360344783,
1.86672108686296));
#24956=CARTESIAN_POINT('Ctrl Pts',(0.106277475451947,-0.1639702967356,1.86649378167475));
#24957=CARTESIAN_POINT('Ctrl Pts',(0.0960907319863873,-0.170572842441436,
1.86579733750091));
#24958=CARTESIAN_POINT('Ctrl Pts',(0.085250296698416,-0.176245842917108,
1.86510089332707));
#24959=CARTESIAN_POINT('Ctrl Pts',(0.0739497550601322,-0.180866231581648,
1.86440444915324));
#24960=CARTESIAN_POINT('Ctrl Pts',(0.062672931091436,-0.185476922936518,
1.86370946668215));
#24961=CARTESIAN_POINT('Ctrl Pts',(0.0509386916758748,-0.189038990307366,
1.86301448421107));
#24962=CARTESIAN_POINT('Ctrl Pts',(0.0389640369531972,-0.191475752575385,
1.86231950173999));
#24963=CARTESIAN_POINT('Ctrl Pts',(0.0269910695104469,-0.193912171493206,
1.8616246171949));
#24964=CARTESIAN_POINT('Ctrl Pts',(0.0147786016129055,-0.195223380555294,
1.86092973264981));
#24965=CARTESIAN_POINT('Ctrl Pts',(0.00255608906482942,-0.195383280780861,
1.86023484810472));
#24966=CARTESIAN_POINT('Ctrl Pts',(-0.00966569692427573,-0.195543171501267,
1.85954000486657));
#24967=CARTESIAN_POINT('Ctrl Pts',(-0.0218966503446213,-0.194551904535922,
1.85884516162842));
#24968=CARTESIAN_POINT('Ctrl Pts',(-0.0339077985664993,-0.192435498794723,
1.85815031839027));
#24969=CARTESIAN_POINT('Ctrl Pts',(-0.045946629472656,-0.19031421526908,
1.85745387371272));
#24970=CARTESIAN_POINT('Ctrl Pts',(-0.0577637931741429,-0.187062831837246,
1.85675742903517));
#24971=CARTESIAN_POINT('Ctrl Pts',(-0.0691421936713439,-0.182758083417162,
1.85606098435762));
#24972=CARTESIAN_POINT('Ctrl Pts',(-0.0728558690716212,-0.181353102258696,
1.8558336791694));
#24973=CARTESIAN_POINT('Ctrl Pts',(-0.0765229659843777,-0.179836296004219,
1.85560637398118));
#24974=CARTESIAN_POINT('Ctrl Pts',(-0.0801364715428752,-0.178211407964412,
1.85537906879296));
#24975=CARTESIAN_POINT('Ctrl Pts',(-0.0912079517543113,-0.173232886280332,
1.85468262461913));
#24976=CARTESIAN_POINT('Ctrl Pts',(-0.101852907383098,-0.16720106306582,
1.85398618044529));
#24977=CARTESIAN_POINT('Ctrl Pts',(-0.111862961234152,-0.160211853194221,
1.85328973627146));
#24978=CARTESIAN_POINT('Ctrl Pts',(-0.121852005901985,-0.153237312333693,
1.85259475380037));
#24979=CARTESIAN_POINT('Ctrl Pts',(-0.131208040160781,-0.145309808214192,
1.85189977132929));
#24980=CARTESIAN_POINT('Ctrl Pts',(-0.139748962759259,-0.136570082403545,
1.8512047888582));
#24981=CARTESIAN_POINT('Ctrl Pts',(-0.148288681905313,-0.127831588057544,
1.85050990431311));
#24982=CARTESIAN_POINT('Ctrl Pts',(-0.156012873316546,-0.118281692330579,
1.84981501976802));
#24983=CARTESIAN_POINT('Ctrl Pts',(-0.162775180527617,-0.108099031467454,
1.84912013522293));
#24984=CARTESIAN_POINT('Ctrl Pts',(-0.169537085757921,-0.0979169759057006,
1.84842529198478));
#24985=CARTESIAN_POINT('Ctrl Pts',(-0.175336758091339,-0.0871029742137949,
1.84773044874663));
#24986=CARTESIAN_POINT('Ctrl Pts',(-0.180071892594372,-0.0758635188841185,
1.84703560550848));
#24987=CARTESIAN_POINT('Ctrl Pts',(-0.184817940394873,-0.0645981594287393,
1.84633916083093));
#24988=CARTESIAN_POINT('Ctrl Pts',(-0.188494272298144,-0.0529062205003197,
1.84564271615338));
#24989=CARTESIAN_POINT('Ctrl Pts',(-0.191047635421175,-0.0410117178374409,
1.84494627147583));
#24990=CARTESIAN_POINT('Ctrl Pts',(-0.19188100051674,-0.0371295973278517,
1.84471896628762));
#24991=CARTESIAN_POINT('Ctrl Pts',(-0.192595151689876,-0.0332259722072379,
1.8444916610994));
#24992=CARTESIAN_POINT('Ctrl Pts',(-0.193189431175088,-0.0293087645977445,
1.84426435591119));
#24993=CARTESIAN_POINT('Ctrl Pts',(-0.194651249258628,-0.0196731553212535,
1.8437052270116));
#24994=CARTESIAN_POINT('Ctrl Pts',(-0.195392425178056,-0.00992552942978188,
1.84314609811201));
#24995=CARTESIAN_POINT('Ctrl Pts',(-0.195399942226119,-0.000150259872500694,
1.84258696921242));
#24996=CARTESIAN_POINT('',(-0.195093080635393,-5.39352580709168E-5,1.77258696921242));
#24997=CARTESIAN_POINT('Ctrl Pts',(-0.195557977360755,-0.000148962866409501,
1.84258688814036));
#24998=CARTESIAN_POINT('Ctrl Pts',(-0.195089261513762,0.0548931456497789,
1.83944113977005));
#24999=CARTESIAN_POINT('Ctrl Pts',(-0.142095896418624,0.175550050373891,
1.83259048710581));
#25000=CARTESIAN_POINT('Ctrl Pts',(0.062482893039627,0.2223465646789,1.82203493014763));
#25001=CARTESIAN_POINT('Ctrl Pts',(0.220698758115634,0.0680747009781973,
1.81092021726587));
#25002=CARTESIAN_POINT('Ctrl Pts',(0.176875795011213,-0.148516194020201,
1.79980550438408));
#25003=CARTESIAN_POINT('Ctrl Pts',(-0.0288682349025461,-0.229147838219507,
1.78869079150232));
#25004=CARTESIAN_POINT('Ctrl Pts',(-0.175242829187112,-0.123730409759538,
1.77961794644509));
#25005=CARTESIAN_POINT('Ctrl Pts',(-0.195165441948141,-0.0293292493376349,
1.77425000568179));
#25006=CARTESIAN_POINT('Ctrl Pts',(-0.195093080635393,-5.39352580709168E-5,
1.77258696921242));
#25007=CARTESIAN_POINT('',(-0.195399918614881,0.00017834039939344,1.70258696783654));
#25008=CARTESIAN_POINT('Ctrl Pts',(-0.195093080635393,-5.39352580709168E-5,
1.77258696921242));
#25009=CARTESIAN_POINT('Ctrl Pts',(-0.195004235779033,0.0358901483346491,
1.77054510138787));
#25010=CARTESIAN_POINT('Ctrl Pts',(-0.168260013010392,0.137176597591161,
1.76479832926938));
#25011=CARTESIAN_POINT('Ctrl Pts',(-0.00538297274404453,0.230896362794104,
1.75534665285699));
#25012=CARTESIAN_POINT('Ctrl Pts',(0.191080370151619,0.129732027232178,
1.7442319399752));
#25013=CARTESIAN_POINT('Ctrl Pts',(0.21261905826749,-0.0901955808703668,
1.73311722709344));
#25014=CARTESIAN_POINT('Ctrl Pts',(0.0395154849224769,-0.227553583136816,
1.72200251421165));
#25015=CARTESIAN_POINT('Ctrl Pts',(-0.152101786416837,-0.162585420427312,
1.71182576158465));
#25016=CARTESIAN_POINT('Ctrl Pts',(-0.194923096983834,-0.0483619519122345,
1.70535391325157));
#25017=CARTESIAN_POINT('Ctrl Pts',(-0.19536023340508,0.000178280042280071,
1.70258696921242));
#25018=CARTESIAN_POINT('',(-0.19542299523852,-5.30184440618641E-5,1.6325869643989));
#25019=CARTESIAN_POINT('Ctrl Pts',(-0.195399918614881,0.00017834039939344,
1.70258696783654));
#25020=CARTESIAN_POINT('Ctrl Pts',(-0.195384897736442,0.0166360719863644,
1.7016490080404));
#25021=CARTESIAN_POINT('Ctrl Pts',(-0.193286029281731,0.0329994316677939,
1.70071104824424));
#25022=CARTESIAN_POINT('Ctrl Pts',(-0.189200457854557,0.048829773167875,
1.69977308844809));
#25023=CARTESIAN_POINT('Ctrl Pts',(-0.186166881757879,0.0605839540536817,
1.69907664427426));
#25024=CARTESIAN_POINT('Ctrl Pts',(-0.182023025638628,0.0720959663926433,
1.69838020010042));
#25025=CARTESIAN_POINT('Ctrl Pts',(-0.176828166483167,0.0831442092884478,
1.69768375592658));
#25026=CARTESIAN_POINT('Ctrl Pts',(-0.171644210340761,0.094169264041337,
1.6969887734555));
#25027=CARTESIAN_POINT('Ctrl Pts',(-0.165413930789739,0.104731665062508,
1.69629379098442));
#25028=CARTESIAN_POINT('Ctrl Pts',(-0.158245230874246,0.114628124409137,
1.69559880851333));
#25029=CARTESIAN_POINT('Ctrl Pts',(-0.151077541059146,0.124523189302436,
1.69490392396824));
#25030=CARTESIAN_POINT('Ctrl Pts',(-0.142972168968596,0.133751763657475,
1.69420903942316));
#25031=CARTESIAN_POINT('Ctrl Pts',(-0.134080413646127,0.1421393776421,1.69351415487807));
#25032=CARTESIAN_POINT('Ctrl Pts',(-0.125189186888024,0.150526493030699,
1.69281931163992));
#25033=CARTESIAN_POINT('Ctrl Pts',(-0.115512325101232,0.158072165812252,
1.69212446840178));
#25034=CARTESIAN_POINT('Ctrl Pts',(-0.105236035027638,0.164640629650344,
1.69142962516363));
#25035=CARTESIAN_POINT('Ctrl Pts',(-0.094936060682695,0.171224232150226,
1.69073318048609));
#25036=CARTESIAN_POINT('Ctrl Pts',(-0.0840346723739042,0.176825712767813,
1.69003673580854));
#25037=CARTESIAN_POINT('Ctrl Pts',(-0.07274364653769,0.181354685322436,
1.68934029113099));
#25038=CARTESIAN_POINT('Ctrl Pts',(-0.0690584884258506,0.182832848616902,
1.68911298594277));
#25039=CARTESIAN_POINT('Ctrl Pts',(-0.0653319660305362,0.184197154967573,
1.68888568075455));
#25040=CARTESIAN_POINT('Ctrl Pts',(-0.0615717759788079,0.185445615755174,
1.68865837556633));
#25041=CARTESIAN_POINT('Ctrl Pts',(-0.0500508666914383,0.18927079567558,
1.6879619313925));
#25042=CARTESIAN_POINT('Ctrl Pts',(-0.0381313510056416,0.192031795032008,
1.68726548721866));
#25043=CARTESIAN_POINT('Ctrl Pts',(-0.0260315626860645,0.193658249873641,
1.68656904304482));
#25044=CARTESIAN_POINT('Ctrl Pts',(-0.013957169501573,0.195281291098496,
1.68587406057374));
#25045=CARTESIAN_POINT('Ctrl Pts',(-0.00170410390458325,0.195774324659698,
1.68517907810265));
#25046=CARTESIAN_POINT('Ctrl Pts',(0.0104983182282932,0.195117772933112,
1.68448409563156));
#25047=CARTESIAN_POINT('Ctrl Pts',(0.0226990209878445,0.194461313717464,
1.68378921108647));
#25048=CARTESIAN_POINT('Ctrl Pts',(0.0348482188803095,0.192655591722484,
1.68309432654138));
#25049=CARTESIAN_POINT('Ctrl Pts',(0.0467172764917712,0.189733118029487,
1.68239944199629));
#25050=CARTESIAN_POINT('Ctrl Pts',(0.0585856285551509,0.186810818060958,
1.68170459875814));
#25051=CARTESIAN_POINT('Ctrl Pts',(0.0701730294300375,0.18277213353102,
1.68100975551999));
#25052=CARTESIAN_POINT('Ctrl Pts',(0.0812644328689661,0.177699892938868,
1.68031491228184));
#25053=CARTESIAN_POINT('Ctrl Pts',(0.0923813992111206,0.17261596210426,
1.67961846760428));
#25054=CARTESIAN_POINT('Ctrl Pts',(0.102999317042159,0.166494142676805,
1.67892202292674));
#25055=CARTESIAN_POINT('Ctrl Pts',(0.112927402782206,0.159463355354343,
1.67822557824919));
#25056=CARTESIAN_POINT('Ctrl Pts',(0.116167725338327,0.157168651285021,
1.67799827306097));
#25057=CARTESIAN_POINT('Ctrl Pts',(0.11933481594715,0.15477745115624,1.67777096787276));
#25058=CARTESIAN_POINT('Ctrl Pts',(0.122422830082389,0.152295143306077,
1.67754366268454));
#25059=CARTESIAN_POINT('Ctrl Pts',(0.131884248319679,0.144689558702015,
1.67684721851071));
#25060=CARTESIAN_POINT('Ctrl Pts',(0.140667694832778,0.136171986337727,
1.67615077433687));
#25061=CARTESIAN_POINT('Ctrl Pts',(0.148595652872058,0.126887713934513,
1.67545433016304));
#25062=CARTESIAN_POINT('Ctrl Pts',(0.156506971647905,0.117622927438457,
1.67475934769195));
#25063=CARTESIAN_POINT('Ctrl Pts',(0.163565746058623,0.107595245630855,
1.67406436522087));
#25064=CARTESIAN_POINT('Ctrl Pts',(0.1696311747703,0.0969867235555868,1.67336938274979));
#25065=CARTESIAN_POINT('Ctrl Pts',(0.175695748837201,0.0863796962663287,
1.6726744982047));
#25066=CARTESIAN_POINT('Ctrl Pts',(0.180766781060075,0.0751927273494488,
1.67197961365961));
#25067=CARTESIAN_POINT('Ctrl Pts',(0.18474760409975,0.0636355465082373,
1.67128472911452));
#25068=CARTESIAN_POINT('Ctrl Pts',(0.188728190502099,0.0520790526758044,
1.67058988587638));
#25069=CARTESIAN_POINT('Ctrl Pts',(0.191618436455313,0.0401532273334309,
1.66989504263823));
#25070=CARTESIAN_POINT('Ctrl Pts',(0.193371320439812,0.0280836684100158,
1.66920019940008));
#25071=CARTESIAN_POINT('Ctrl Pts',(0.195128244382275,0.0159862921803006,
1.66850375472253));
#25072=CARTESIAN_POINT('Ctrl Pts',(0.19574251163749,0.00374539646522498,
1.66780731004499));
#25073=CARTESIAN_POINT('Ctrl Pts',(0.195218984440051,-0.00840881169936014,
1.66711086536744));
#25074=CARTESIAN_POINT('Ctrl Pts',(0.195048115953308,-0.0123756947319901,
1.66688356017922));
#25075=CARTESIAN_POINT('Ctrl Pts',(0.194756459524436,-0.016333375556504,
1.666656254991));
#25076=CARTESIAN_POINT('Ctrl Pts',(0.194345373103489,-0.0202740216352289,
1.66642894980278));
#25077=CARTESIAN_POINT('Ctrl Pts',(0.193085838532137,-0.032347833166574,
1.66573250562894));
#25078=CARTESIAN_POINT('Ctrl Pts',(0.19069240378987,-0.0443465598391951,
1.66503606145511));
#25079=CARTESIAN_POINT('Ctrl Pts',(0.187190876971227,-0.0560422660029291,
1.66433961728127));
#25080=CARTESIAN_POINT('Ctrl Pts',(0.183696699185824,-0.0677134251225244,
1.66364463481019));
#25081=CARTESIAN_POINT('Ctrl Pts',(0.179099222576406,-0.0790819741698788,
1.6629496523391));
#25082=CARTESIAN_POINT('Ctrl Pts',(0.173475057028626,-0.0899308878468068,
1.66225466986802));
#25083=CARTESIAN_POINT('Ctrl Pts',(0.167851683949762,-0.100778272865523,
1.66155978532293));
#25084=CARTESIAN_POINT('Ctrl Pts',(0.161202270606598,-0.111105370402818,
1.66086490077784));
#25085=CARTESIAN_POINT('Ctrl Pts',(0.153650611916079,-0.120717229332911,
1.66017001623275));
#25086=CARTESIAN_POINT('Ctrl Pts',(0.146099402128791,-0.130328516892565,
1.6594751729946));
#25087=CARTESIAN_POINT('Ctrl Pts',(0.137646615537259,-0.139223978128796,
1.65878032975645));
#25088=CARTESIAN_POINT('Ctrl Pts',(0.128456301231854,-0.147241769460405,
1.6580854865183));
#25089=CARTESIAN_POINT('Ctrl Pts',(0.119244805556886,-0.155278039790189,
1.65738904184075));
#25090=CARTESIAN_POINT('Ctrl Pts',(0.10929309085982,-0.162432075487393,
1.6566925971632));
#25091=CARTESIAN_POINT('Ctrl Pts',(0.0987972140537528,-0.168583126365651,
1.65599615248565));
#25092=CARTESIAN_POINT('Ctrl Pts',(0.0953715761964439,-0.170590702592023,
1.65576884729743));
#25093=CARTESIAN_POINT('Ctrl Pts',(0.0918881698059328,-0.172491802510378,
1.65554154210921));
#25094=CARTESIAN_POINT('Ctrl Pts',(0.0883543121723104,-0.174283319685384,
1.65531423692099));
#25095=CARTESIAN_POINT('Ctrl Pts',(0.0775268665720683,-0.179772379168067,
1.65461779274716));
#25096=CARTESIAN_POINT('Ctrl Pts',(0.0661476220366477,-0.184268017658048,
1.65392134857332));
#25097=CARTESIAN_POINT('Ctrl Pts',(0.0544220854670605,-0.187668315422226,
1.65322490439949));
#25098=CARTESIAN_POINT('Ctrl Pts',(0.0427211585499092,-0.191061476613535,
1.65252992192841));
#25099=CARTESIAN_POINT('Ctrl Pts',(0.030676194008489,-0.193363546945208,
1.65183493945732));
#25100=CARTESIAN_POINT('Ctrl Pts',(0.0185110803761076,-0.194521206821542,
1.65113995698624));
#25101=CARTESIAN_POINT('Ctrl Pts',(0.00634768086012452,-0.195678703578663,
1.65044507244115));
#25102=CARTESIAN_POINT('Ctrl Pts',(-0.00593496808282118,-0.195691981273954,
1.64975018789606));
#25103=CARTESIAN_POINT('Ctrl Pts',(-0.0181059374205579,-0.194559335499798,
1.64905530335097));
#25104=CARTESIAN_POINT('Ctrl Pts',(-0.0302761832632767,-0.193426757055001,
1.64836046011282));
#25105=CARTESIAN_POINT('Ctrl Pts',(-0.042333893166877,-0.191148498147918,
1.64766561687467));
#25106=CARTESIAN_POINT('Ctrl Pts',(-0.0540541262823569,-0.187774629361506,
1.64697077363653));
#25107=CARTESIAN_POINT('Ctrl Pts',(-0.0658013715957562,-0.184392984653702,
1.64627432895898));
#25108=CARTESIAN_POINT('Ctrl Pts',(-0.0772087642590092,-0.179910993489646,
1.64557788428143));
#25109=CARTESIAN_POINT('Ctrl Pts',(-0.0880685331149196,-0.174427903372672,
1.64488143960388));
#25110=CARTESIAN_POINT('Ctrl Pts',(-0.0916129378370585,-0.172638335771338,
1.64465413441567));
#25111=CARTESIAN_POINT('Ctrl Pts',(-0.0950992074404759,-0.170742491570658,
1.64442682922745));
#25112=CARTESIAN_POINT('Ctrl Pts',(-0.0985207639132304,-0.16874483422598,
1.64419952403923));
#25113=CARTESIAN_POINT('Ctrl Pts',(-0.109004128105527,-0.162624178424318,
1.64350307986539));
#25114=CARTESIAN_POINT('Ctrl Pts',(-0.118952045286865,-0.15550119341922,
1.64280663569156));
#25115=CARTESIAN_POINT('Ctrl Pts',(-0.128167441182025,-0.147493277883612,
1.64211019151772));
#25116=CARTESIAN_POINT('Ctrl Pts',(-0.137363495728602,-0.139502169426891,
1.64141520904664));
#25117=CARTESIAN_POINT('Ctrl Pts',(-0.145829377222639,-0.130630329192478,
1.64072022657555));
#25118=CARTESIAN_POINT('Ctrl Pts',(-0.153398877393225,-0.121036954747293,
1.64002524410447));
#25119=CARTESIAN_POINT('Ctrl Pts',(-0.160967310988954,-0.111444932049483,
1.63933035955938));
#25120=CARTESIAN_POINT('Ctrl Pts',(-0.167639036205313,-0.101132234827594,
1.63863547501429));
#25121=CARTESIAN_POINT('Ctrl Pts',(-0.173287394034427,-0.0902919656932838,
1.6379405904692));
#25122=CARTESIAN_POINT('Ctrl Pts',(-0.178935416100738,-0.0794523409514253,
1.63724574723105));
#25123=CARTESIAN_POINT('Ctrl Pts',(-0.183559810586553,-0.06808599556662,
1.6365509039929));
#25124=CARTESIAN_POINT('Ctrl Pts',(-0.18708066713741,-0.0564090771367656,
1.63585606075475));
#25125=CARTESIAN_POINT('Ctrl Pts',(-0.190609638379593,-0.0447052463384756,
1.6351596160772));
#25126=CARTESIAN_POINT('Ctrl Pts',(-0.193029803639046,-0.0326902701718145,
1.63446317139965));
#25127=CARTESIAN_POINT('Ctrl Pts',(-0.194311881761601,-0.0205925376354037,
1.6337667267221));
#25128=CARTESIAN_POINT('Ctrl Pts',(-0.19473032563569,-0.0166440870837835,
1.63353942153388));
#25129=CARTESIAN_POINT('Ctrl Pts',(-0.195027950573094,-0.0126868506266221,
1.63331211634566));
#25130=CARTESIAN_POINT('Ctrl Pts',(-0.195204939685526,-0.00872877553671252,
1.63308481115744));
#25131=CARTESIAN_POINT('Ctrl Pts',(-0.195334153049388,-0.00583912775127325,
1.63291886384244));
#25132=CARTESIAN_POINT('Ctrl Pts',(-0.195399206533935,-0.00294658962844581,
1.63275291652743));
#25133=CARTESIAN_POINT('Ctrl Pts',(-0.195399992786049,-5.30962533302248E-5,
1.63258696921242));
#25134=CARTESIAN_POINT('',(-0.195203598247727,-0.000145069483009505,1.56258696921242));
#25135=CARTESIAN_POINT('Ctrl Pts',(-0.195702830166494,-5.20718601689164E-5,
1.63258690584025));
#25136=CARTESIAN_POINT('Ctrl Pts',(-0.195478538915108,0.061749283732994,
1.6290479699854));
#25137=CARTESIAN_POINT('Ctrl Pts',(-0.13051040340586,0.188655383227059,
1.6218041298366));
#25138=CARTESIAN_POINT('Ctrl Pts',(0.0856301532178521,0.214498446630602,
1.6108553853939));
#25139=CARTESIAN_POINT('Ctrl Pts',(0.226656931919608,0.0443705077713918,
1.59974067251211));
#25140=CARTESIAN_POINT('Ctrl Pts',(0.16019046818058,-0.166376442596738,
1.58862595963034));
#25141=CARTESIAN_POINT('Ctrl Pts',(-0.0529224685754463,-0.224813965462503,
1.57751124674856));
#25142=CARTESIAN_POINT('Ctrl Pts',(-0.181512116776874,-0.109731403433318,
1.56883158327592));
#25143=CARTESIAN_POINT('Ctrl Pts',(-0.195357411599742,-0.0224672944395423,
1.56385682409721));
#25144=CARTESIAN_POINT('Ctrl Pts',(-0.195203598247727,-0.000145069483009505,
1.56258696921242));
#25145=CARTESIAN_POINT('',(-0.195399954007542,0.000134066589732251,1.49258696650567));
#25146=CARTESIAN_POINT('Ctrl Pts',(-0.195203598247727,-0.000145069483009505,
1.56258696921242));
#25147=CARTESIAN_POINT('Ctrl Pts',(-0.194908648709454,0.0426596016193331,
1.56015191980329));
#25148=CARTESIAN_POINT('Ctrl Pts',(-0.159970883662516,0.151029040268688,
1.55401196610022));
#25149=CARTESIAN_POINT('Ctrl Pts',(0.0190478344627849,0.230172297962467,
1.54416710810324));
#25150=CARTESIAN_POINT('Ctrl Pts',(0.203720217624868,0.108812589703487,
1.53305239522145));
#25151=CARTESIAN_POINT('Ctrl Pts',(0.201896789043055,-0.112159677786471,
1.52193768233969));
#25152=CARTESIAN_POINT('Ctrl Pts',(0.0152468076525971,-0.230455291984146,
1.5108229694579));
#25153=CARTESIAN_POINT('Ctrl Pts',(-0.16133530721145,-0.148879556632701,
1.5010393984155));
#25154=CARTESIAN_POINT('Ctrl Pts',(-0.194916683322746,-0.0416061777329493,
1.49496073166699));
#25155=CARTESIAN_POINT('Ctrl Pts',(-0.195179950177078,0.000133868047100166,
1.49258696921242));
#25156=CARTESIAN_POINT('',(-0.195415762289312,7.15973788392893E-5,1.42258696921242));
#25157=CARTESIAN_POINT('Ctrl Pts',(-0.195399954007542,0.000134066589732251,
1.49258696650567));
#25158=CARTESIAN_POINT('Ctrl Pts',(-0.195390351133564,0.0141301049573953,
1.49179190213383));
#25159=CARTESIAN_POINT('Ctrl Pts',(-0.193872852752641,0.0280660265355398,
1.49099683776198));
#25160=CARTESIAN_POINT('Ctrl Pts',(-0.190910121066081,0.0416471568601563,
1.49020177339012));
#25161=CARTESIAN_POINT('Ctrl Pts',(-0.188912482783523,0.0508043093555799,
1.48966569682487));
#25162=CARTESIAN_POINT('Ctrl Pts',(-0.186258880595048,0.0598005076247773,
1.48912962025961));
#25163=CARTESIAN_POINT('Ctrl Pts',(-0.182980778986252,0.0685506711971836,
1.48859354369435));
#25164=CARTESIAN_POINT('Ctrl Pts',(-0.178722031421712,0.0799184511657234,
1.48789709952051));
#25165=CARTESIAN_POINT('Ctrl Pts',(-0.173384812841909,0.0909280864667609,
1.48720065534668));
#25166=CARTESIAN_POINT('Ctrl Pts',(-0.167051486644434,0.101365481352798,
1.48650421117284));
#25167=CARTESIAN_POINT('Ctrl Pts',(-0.160731452883988,0.111780970148742,
1.48580922870175));
#25168=CARTESIAN_POINT('Ctrl Pts',(-0.153419847023285,0.121625822527253,
1.48511424623067));
#25169=CARTESIAN_POINT('Ctrl Pts',(-0.145245450955154,0.130709291853464,
1.48441926375958));
#25170=CARTESIAN_POINT('Ctrl Pts',(-0.137072206694295,0.139791481280103,
1.48372437921449));
#25171=CARTESIAN_POINT('Ctrl Pts',(-0.128036964184847,0.148111819863908,
1.4830294946694));
#25172=CARTESIAN_POINT('Ctrl Pts',(-0.11830861287875,0.15551280371309,1.48233461012431));
#25173=CARTESIAN_POINT('Ctrl Pts',(-0.108580839867898,0.162913347615806,
1.48163976688616));
#25174=CARTESIAN_POINT('Ctrl Pts',(-0.098160753035793,0.169394136316214,
1.48094492364801));
#25175=CARTESIAN_POINT('Ctrl Pts',(-0.0872478639558456,0.174839841669862,
1.48025008040986));
#25176=CARTESIAN_POINT('Ctrl Pts',(-0.0763098234035006,0.180298098008577,
1.47955363573231));
#25177=CARTESIAN_POINT('Ctrl Pts',(-0.0648775252347868,0.184716175729808,
1.47885719105476));
#25178=CARTESIAN_POINT('Ctrl Pts',(-0.0531711118537846,0.188026574888318,
1.47816074637721));
#25179=CARTESIAN_POINT('Ctrl Pts',(-0.0493503798091365,0.189107020942446,
1.477933441189));
#25180=CARTESIAN_POINT('Ctrl Pts',(-0.0455005472779019,0.190069876311248,
1.47770613600079));
#25181=CARTESIAN_POINT('Ctrl Pts',(-0.0416294779424288,0.190913976875034,
1.47747883081258));
#25182=CARTESIAN_POINT('Ctrl Pts',(-0.0297688437596777,0.193500230732273,
1.47678238663874));
#25183=CARTESIAN_POINT('Ctrl Pts',(-0.0176242956823007,0.194986139082841,
1.47608594246491));
#25184=CARTESIAN_POINT('Ctrl Pts',(-0.00542038081509231,0.195324805060236,
1.47538949829107));
#25185=CARTESIAN_POINT('Ctrl Pts',(0.00675792037537916,0.195662760242697,
1.47469451581999));
#25186=CARTESIAN_POINT('Ctrl Pts',(0.0189944765403277,0.194858153606765,
1.4739995333489));
#25187=CARTESIAN_POINT('Ctrl Pts',(0.0310591869555855,0.192915750797228,
1.47330455087782));
#25188=CARTESIAN_POINT('Ctrl Pts',(0.0431221974016848,0.190973621680531,
1.47260966633273));
#25189=CARTESIAN_POINT('Ctrl Pts',(0.0550125396006769,0.187894108124109,
1.47191478178764));
#25190=CARTESIAN_POINT('Ctrl Pts',(0.0665062941107382,0.183733700892504,
1.47121989724254));
#25191=CARTESIAN_POINT('Ctrl Pts',(0.0779993653823561,0.179573540973485,
1.47052505400439));
#25192=CARTESIAN_POINT('Ctrl Pts',(0.0890950813965693,0.174332938155153,
1.46983021076624));
#25193=CARTESIAN_POINT('Ctrl Pts',(0.099588353227997,0.168116982786795,
1.46913536752809));
#25194=CARTESIAN_POINT('Ctrl Pts',(0.110105809419304,0.161886701200264,
1.46843892285055));
#25195=CARTESIAN_POINT('Ctrl Pts',(0.120017329584307,0.154677081225006,
1.467742478173));
#25196=CARTESIAN_POINT('Ctrl Pts',(0.129146822535201,0.146636483281144,
1.46704603349545));
#25197=CARTESIAN_POINT('Ctrl Pts',(0.13212650086488,0.144012197838365,1.46681872830723));
#25198=CARTESIAN_POINT('Ctrl Pts',(0.135023159806546,0.141299695680558,
1.46659142311902));
#25199=CARTESIAN_POINT('Ctrl Pts',(0.137831556989672,0.138504952611099,
1.4663641179308));
#25200=CARTESIAN_POINT('Ctrl Pts',(0.146436252163398,0.129942092504961,
1.46566767375697));
#25201=CARTESIAN_POINT('Ctrl Pts',(0.15427039494324,0.120543998095244,1.46497122958313));
#25202=CARTESIAN_POINT('Ctrl Pts',(0.161172816316964,0.110473903164767,
1.4642747854093));
#25203=CARTESIAN_POINT('Ctrl Pts',(0.168060750832027,0.100424943432224,
1.46357980293822));
#25204=CARTESIAN_POINT('Ctrl Pts',(0.174020293639803,0.089707455473858,
1.46288482046713));
#25205=CARTESIAN_POINT('Ctrl Pts',(0.178930671049179,0.0785173545013498,
1.46218983799605));
#25206=CARTESIAN_POINT('Ctrl Pts',(0.183840356565433,0.0673288302617974,
1.46149495345096));
#25207=CARTESIAN_POINT('Ctrl Pts',(0.187700776603113,0.0556686073443341,
1.46080006890588));
#25208=CARTESIAN_POINT('Ctrl Pts',(0.19043796893578,0.0437554566610235,
1.46010518436079));
#25209=CARTESIAN_POINT('Ctrl Pts',(0.193174998557906,0.0318430141468777,
1.45941034112264));
#25210=CARTESIAN_POINT('Ctrl Pts',(0.194788762984549,0.0196785332232306,
1.45871549788449));
#25211=CARTESIAN_POINT('Ctrl Pts',(0.195256344734548,0.00749131770139881,
1.45802065464634));
#25212=CARTESIAN_POINT('Ctrl Pts',(0.195725004143213,-0.00472398629568257,
1.4573242099688));
#25213=CARTESIAN_POINT('Ctrl Pts',(0.195042238430193,-0.016961252458877,
1.45662776529125));
#25214=CARTESIAN_POINT('Ctrl Pts',(0.193237210421569,-0.0289920766501849,
1.4559313206137));
#25215=CARTESIAN_POINT('Ctrl Pts',(0.192648086483255,-0.0329186896971232,
1.45570401542548));
#25216=CARTESIAN_POINT('Ctrl Pts',(0.19193982343752,-0.0368233874370288,
1.45547671023725));
#25217=CARTESIAN_POINT('Ctrl Pts',(0.191114599357323,-0.0406985246967225,
1.45524940504903));
#25218=CARTESIAN_POINT('Ctrl Pts',(0.188586181474533,-0.0525716226598113,
1.45455296087519));
#25219=CARTESIAN_POINT('Ctrl Pts',(0.184938147622258,-0.0642502279122655,
1.45385651670135));
#25220=CARTESIAN_POINT('Ctrl Pts',(0.18022024916266,-0.0755104084994154,
1.45316007252752));
#25221=CARTESIAN_POINT('Ctrl Pts',(0.175512252667091,-0.0867469561270848,
1.45246509005643));
#25222=CARTESIAN_POINT('Ctrl Pts',(0.169739114602154,-0.0975659937691164,
1.45177010758535));
#25223=CARTESIAN_POINT('Ctrl Pts',(0.162999950667442,-0.107759807360682,
1.45107512511426));
#25224=CARTESIAN_POINT('Ctrl Pts',(0.156261736309674,-0.117952184600432,
1.45038024056917));
#25225=CARTESIAN_POINT('Ctrl Pts',(0.148558210037661,-0.127518757880856,
1.44968535602408));
#25226=CARTESIAN_POINT('Ctrl Pts',(0.140033075610836,-0.136278750122571,
1.44899047147899));
#25227=CARTESIAN_POINT('Ctrl Pts',(0.131508447954845,-0.145038221632486,
1.44829562824084));
#25228=CARTESIAN_POINT('Ctrl Pts',(0.122162939052251,-0.152990598328739,
1.44760078500269));
#25229=CARTESIAN_POINT('Ctrl Pts',(0.112176782689824,-0.15999227926797,
1.44690594176454));
#25230=CARTESIAN_POINT('Ctrl Pts',(0.10216761074149,-0.167010097325757,
1.44620949708699));
#25231=CARTESIAN_POINT('Ctrl Pts',(0.0915155974866367,-0.173072396047143,
1.44551305240944));
#25232=CARTESIAN_POINT('Ctrl Pts',(0.080428462636264,-0.178079820299682,
1.44481660773189));
#25233=CARTESIAN_POINT('Ctrl Pts',(0.0768098503398591,-0.179714140366867,
1.44458930254368));
#25234=CARTESIAN_POINT('Ctrl Pts',(0.0731450451935352,-0.181236475487685,
1.44436199735546));
#25235=CARTESIAN_POINT('Ctrl Pts',(0.0694416517953648,-0.182644509898139,
1.44413469216724));
#25236=CARTESIAN_POINT('Ctrl Pts',(0.0580947627260293,-0.186958610114745,
1.44343824799341));
#25237=CARTESIAN_POINT('Ctrl Pts',(0.0463041473121616,-0.190226539090695,
1.44274180381957));
#25238=CARTESIAN_POINT('Ctrl Pts',(0.0342849323719999,-0.192368665359635,
1.44204535964574));
#25239=CARTESIAN_POINT('Ctrl Pts',(0.0222909434588516,-0.194506295716373,
1.44135037717466));
#25240=CARTESIAN_POINT('Ctrl Pts',(0.0100701476881834,-0.195522587676248,
1.44065539470357));
#25241=CARTESIAN_POINT('Ctrl Pts',(-0.00214918538429394,-0.19538818030317,
1.43996041223249));
#25242=CARTESIAN_POINT('Ctrl Pts',(-0.0143667967006226,-0.195253791868663,
1.4392655276874));
#25243=CARTESIAN_POINT('Ctrl Pts',(-0.0265820709186002,-0.193968989497673,
1.43857064314231));
#25244=CARTESIAN_POINT('Ctrl Pts',(-0.0385651919972097,-0.191556482443739,
1.43787575859722));
#25245=CARTESIAN_POINT('Ctrl Pts',(-0.0505476007473118,-0.18914411879965,
1.43718091535907));
#25246=CARTESIAN_POINT('Ctrl Pts',(-0.0622970304997711,-0.185604382614689,
1.43648607212092));
#25247=CARTESIAN_POINT('Ctrl Pts',(-0.0735950913425348,-0.181010835394691,
1.43579122888277));
#25248=CARTESIAN_POINT('Ctrl Pts',(-0.0849191913820126,-0.176406701200403,
1.43509478420523));
#25249=CARTESIAN_POINT('Ctrl Pts',(-0.0957890594016855,-0.170744296993414,
1.43439833952768));
#25250=CARTESIAN_POINT('Ctrl Pts',(-0.106008575956307,-0.164144271370389,
1.43370189485013));
#25251=CARTESIAN_POINT('Ctrl Pts',(-0.109344015523638,-0.161990159041222,
1.43347458966191));
#25252=CARTESIAN_POINT('Ctrl Pts',(-0.112610414407529,-0.159736508821645,
1.43324728447369));
#25253=CARTESIAN_POINT('Ctrl Pts',(-0.115801703119268,-0.157388454324569,
1.43301997928548));
#25254=CARTESIAN_POINT('Ctrl Pts',(-0.125492033249174,-0.150258600119908,
1.43232976836662));
#25255=CARTESIAN_POINT('Ctrl Pts',(-0.134558675788076,-0.142202839596349,
1.43163955744776));
#25256=CARTESIAN_POINT('Ctrl Pts',(-0.142819844890049,-0.133355359493281,
1.43094934652889));
#25257=CARTESIAN_POINT('Ctrl Pts',(-0.151160654346282,-0.124422586807406,
1.43025248175252));
#25258=CARTESIAN_POINT('Ctrl Pts',(-0.158679605738282,-0.11468327090578,
1.42955561697615));
#25259=CARTESIAN_POINT('Ctrl Pts',(-0.165224794108631,-0.104316477182468,
1.42885875219978));
#25260=CARTESIAN_POINT('Ctrl Pts',(-0.171692724670043,-0.094072050566634,
1.42817011304545));
#25261=CARTESIAN_POINT('Ctrl Pts',(-0.177209306120145,-0.0832156728885014,
1.42748147389112));
#25262=CARTESIAN_POINT('Ctrl Pts',(-0.181671077724288,-0.0719498402951364,
1.42679283473679));
#25263=CARTESIAN_POINT('Ctrl Pts',(-0.186212791443188,-0.0604821563830781,
1.4260918571494));
#25264=CARTESIAN_POINT('Ctrl Pts',(-0.189661094091221,-0.0485910563735383,
1.425390879562));
#25265=CARTESIAN_POINT('Ctrl Pts',(-0.191959025352893,-0.0365088014808403,
1.42468990197461));
#25266=CARTESIAN_POINT('Ctrl Pts',(-0.194256956614565,-0.0244265465881405,
1.42398892438721));
#25267=CARTESIAN_POINT('Ctrl Pts',(-0.195404466195307,-0.0121541052075848,
1.42328794679982));
#25268=CARTESIAN_POINT('Ctrl Pts',(-0.195399986884961,7.15915989697979E-5,
1.42258696921242));
#25269=CARTESIAN_POINT('',(-0.195392498133114,-0.000178699422991063,1.35258696921242));
#25270=CARTESIAN_POINT('Ctrl Pts',(-0.195688377393879,7.16972608892641E-5,
1.42258696921242));
#25271=CARTESIAN_POINT('Ctrl Pts',(-0.195707099359798,0.0040407295163859,
1.42235973494285));
#25272=CARTESIAN_POINT('Ctrl Pts',(-0.193798549159007,0.0727038566799422,
1.41842759637929));
#25273=CARTESIAN_POINT('Ctrl Pts',(-0.113142331553771,0.201347757766985,
1.41079055352198));
#25274=CARTESIAN_POINT('Ctrl Pts',(0.107818424683884,0.204248118830208,
1.39967584064012));
#25275=CARTESIAN_POINT('Ctrl Pts',(0.230076730733924,0.0201694006329071,
1.38856112775837));
#25276=CARTESIAN_POINT('Ctrl Pts',(0.141711137193357,-0.182373409088167,
1.3774464148766));
#25277=CARTESIAN_POINT('Ctrl Pts',(-0.0763840132470003,-0.217962357455062,
1.36633170199481));
#25278=CARTESIAN_POINT('Ctrl Pts',(-0.186850444349053,-0.0957346434792127,
1.35804522010676));
#25279=CARTESIAN_POINT('Ctrl Pts',(-0.195533353731187,-0.0155516148321636,
1.35346364251263));
#25280=CARTESIAN_POINT('Ctrl Pts',(-0.195392498133114,-0.000178699422991063,
1.35258696921242));
#25281=CARTESIAN_POINT('',(-0.19537121115614,3.68736377462065E-5,1.28258696733929));
#25282=CARTESIAN_POINT('Ctrl Pts',(-0.195392498133114,-0.000178699422991063,
1.35258696921242));
#25283=CARTESIAN_POINT('Ctrl Pts',(-0.194938084649759,0.0494157798589555,
1.3497587382187));
#25284=CARTESIAN_POINT('Ctrl Pts',(-0.150558264293769,0.164701191617148,
1.34322560293105));
#25285=CARTESIAN_POINT('Ctrl Pts',(0.0432653212731082,0.226870488874589,
1.33298756334949));
#25286=CARTESIAN_POINT('Ctrl Pts',(0.214078562825376,0.0866745388549855,
1.32187285046771));
#25287=CARTESIAN_POINT('Ctrl Pts',(0.188913438476778,-0.132867676693533,
1.31075813758593));
#25288=CARTESIAN_POINT('Ctrl Pts',(-0.00919262157656059,-0.23077608726999,
1.29964342470415));
#25289=CARTESIAN_POINT('Ctrl Pts',(-0.169454903792707,-0.135006243596358,
1.29025303524633));
#25290=CARTESIAN_POINT('Ctrl Pts',(-0.195026953550068,-0.0348317645878951,
1.28456755008241));
#25291=CARTESIAN_POINT('Ctrl Pts',(-0.195085605073228,3.67867518197285E-5,
1.28258696921242));
#25292=CARTESIAN_POINT('',(-0.19539993476676,0.000159665732175137,1.21258696921242));
#25293=CARTESIAN_POINT('Ctrl Pts',(-0.195399996519163,3.68823947128292E-5,
1.2825869671505));
#25294=CARTESIAN_POINT('Ctrl Pts',(-0.195397534591892,0.0130799774522216,
1.2818472934737));
#25295=CARTESIAN_POINT('Ctrl Pts',(-0.194084875265927,0.0260895437433635,
1.28110761979689));
#25296=CARTESIAN_POINT('Ctrl Pts',(-0.191507126714693,0.0388095402895012,
1.28036794612009));
#25297=CARTESIAN_POINT('Ctrl Pts',(-0.188915309047009,0.0515989614164704,
1.27962423537183));
#25298=CARTESIAN_POINT('Ctrl Pts',(-0.185044815819923,0.0640949892409484,
1.27888052462358));
#25299=CARTESIAN_POINT('Ctrl Pts',(-0.179990958120247,0.0760553416595802,
1.27813681387532));
#25300=CARTESIAN_POINT('Ctrl Pts',(-0.178353671118658,0.0799301103438472,
1.27789587556375));
#25301=CARTESIAN_POINT('Ctrl Pts',(-0.176592551635074,0.0837488379902776,
1.27765493725218));
#25302=CARTESIAN_POINT('Ctrl Pts',(-0.17471186284551,0.087503856949576,
1.27741399894062));
#25303=CARTESIAN_POINT('Ctrl Pts',(-0.169275638353994,0.0983579260257119,
1.27671755476678));
#25304=CARTESIAN_POINT('Ctrl Pts',(-0.162804829860834,0.108741885245363,
1.27602111059294));
#25305=CARTESIAN_POINT('Ctrl Pts',(-0.155403964771163,0.118451541709693,
1.27532466641911));
#25306=CARTESIAN_POINT('Ctrl Pts',(-0.148018632677917,0.128140819467302,
1.27462968394802));
#25307=CARTESIAN_POINT('Ctrl Pts',(-0.139707584601259,0.137157868789804,
1.27393470147693));
#25308=CARTESIAN_POINT('Ctrl Pts',(-0.130619039029278,0.145326620558891,
1.27323971900585));
#25309=CARTESIAN_POINT('Ctrl Pts',(-0.121531774072133,0.153494221316013,
1.27254483446076));
#25310=CARTESIAN_POINT('Ctrl Pts',(-0.111667848579019,0.160813143041246,
1.27184994991566));
#25311=CARTESIAN_POINT('Ctrl Pts',(-0.101211850984521,0.167144611699831,
1.27115506537057));
#25312=CARTESIAN_POINT('Ctrl Pts',(-0.0907564749397088,0.173475703988555,
1.27046022213242));
#25313=CARTESIAN_POINT('Ctrl Pts',(-0.0797098596379881,0.178819028996811,
1.26976537889427));
#25314=CARTESIAN_POINT('Ctrl Pts',(-0.0682825871154466,0.183080988354393,
1.26907053565611));
#25315=CARTESIAN_POINT('Ctrl Pts',(-0.0568289775956777,0.187352770459404,
1.26837409097856));
#25316=CARTESIAN_POINT('Ctrl Pts',(-0.0449938020940338,0.19053796637405,
1.26767764630101));
#25317=CARTESIAN_POINT('Ctrl Pts',(-0.033003103564723,0.192592718333524,
1.26698120162346));
#25318=CARTESIAN_POINT('Ctrl Pts',(-0.029089586707128,0.193263347022247,
1.26675389643525));
#25319=CARTESIAN_POINT('Ctrl Pts',(-0.0251595590618304,0.193813968205019,
1.26652659124704));
#25320=CARTESIAN_POINT('Ctrl Pts',(-0.0212209632995607,0.194244255298937,
1.26629928605883));
#25321=CARTESIAN_POINT('Ctrl Pts',(-0.00915343376659917,0.1955626191339,
1.26560284188499));
#25322=CARTESIAN_POINT('Ctrl Pts',(0.00308013755035486,0.195756795502481,
1.26490639771116));
#25323=CARTESIAN_POINT('Ctrl Pts',(0.0152515049529862,0.19480387982961,
1.26420995353733));
#25324=CARTESIAN_POINT('Ctrl Pts',(0.0273973269897674,0.193852964143977,
1.26351497106624));
#25325=CARTESIAN_POINT('Ctrl Pts',(0.0394803341542351,0.191759728256867,
1.26281998859516));
#25326=CARTESIAN_POINT('Ctrl Pts',(0.0512722178173541,0.188553227710612,
1.26212500612408));
#25327=CARTESIAN_POINT('Ctrl Pts',(0.0630624399537676,0.18534717897396,
1.26143012157899));
#25328=CARTESIAN_POINT('Ctrl Pts',(0.0745607642082807,0.181028361926375,
1.2607352370339));
#25329=CARTESIAN_POINT('Ctrl Pts',(0.0855504948284708,0.175676614364587,
1.26004035248881));
#25330=CARTESIAN_POINT('Ctrl Pts',(0.0965395721715766,0.170325184933803,
1.25934550925066));
#25331=CARTESIAN_POINT('Ctrl Pts',(0.10701934024705,0.16394135435562,1.25865066601251));
#25332=CARTESIAN_POINT('Ctrl Pts',(0.116796964282291,0.156651297902192,
1.25795582277437));
#25333=CARTESIAN_POINT('Ctrl Pts',(0.126597123288727,0.149344439696969,
1.25725937809682));
#25334=CARTESIAN_POINT('Ctrl Pts',(0.135691244748885,0.141127761107914,
1.25656293341927));
#25335=CARTESIAN_POINT('Ctrl Pts',(0.143919901946437,0.132167400760279,
1.25586648874173));
#25336=CARTESIAN_POINT('Ctrl Pts',(0.146605566053609,0.129242923826164,
1.2556391835535));
#25337=CARTESIAN_POINT('Ctrl Pts',(0.149199353082293,0.126239497477568,
1.25541187836528));
#25338=CARTESIAN_POINT('Ctrl Pts',(0.151696681528045,0.123163618058982,
1.25518457317706));
#25339=CARTESIAN_POINT('Ctrl Pts',(0.15934828798626,0.113739379583673,1.25448812900322));
#25340=CARTESIAN_POINT('Ctrl Pts',(0.166145390946764,0.103566014212564,
1.25379168482939));
#25341=CARTESIAN_POINT('Ctrl Pts',(0.171944974097777,0.0928228737031702,
1.25309524065555));
#25342=CARTESIAN_POINT('Ctrl Pts',(0.17773238503605,0.082102280985295,1.25240025818446));
#25343=CARTESIAN_POINT('Ctrl Pts',(0.182525954163857,0.0708150141047222,
1.25170527571338));
#25344=CARTESIAN_POINT('Ctrl Pts',(0.186226288000902,0.0591686543484393,
1.25101029324229));
#25345=CARTESIAN_POINT('Ctrl Pts',(0.189926100445126,0.0475239356139243,
1.2503154086972));
#25346=CARTESIAN_POINT('Ctrl Pts',(0.192532674704041,0.0355210437962889,
1.24962052415211));
#25347=CARTESIAN_POINT('Ctrl Pts',(0.193995581981284,0.0233853409584502,
1.24892563960702));
#25348=CARTESIAN_POINT('Ctrl Pts',(0.195458402296995,0.011250359519239,
1.24823079636887));
#25349=CARTESIAN_POINT('Ctrl Pts',(0.195777612335889,-0.00101654460194885,
1.24753595313072));
#25350=CARTESIAN_POINT('Ctrl Pts',(0.194954655312547,-0.0131849297292836,
1.24684110989257));
#25351=CARTESIAN_POINT('Ctrl Pts',(0.194129801579661,-0.0253813599325303,
1.24614466521503));
#25352=CARTESIAN_POINT('Ctrl Pts',(0.192157649324152,-0.0374779490240786,
1.24544822053748));
#25353=CARTESIAN_POINT('Ctrl Pts',(0.189091335363429,-0.0492506537060681,
1.24475177585993));
#25354=CARTESIAN_POINT('Ctrl Pts',(0.188090553686938,-0.053093021865166,
1.24452447067171));
#25355=CARTESIAN_POINT('Ctrl Pts',(0.186973615999746,-0.0569010070520961,
1.24429716548349));
#25356=CARTESIAN_POINT('Ctrl Pts',(0.185743496105052,-0.0606672370779526,
1.24406986029527));
#25357=CARTESIAN_POINT('Ctrl Pts',(0.181974511153627,-0.0722066523433209,
1.24337341612144));
#25358=CARTESIAN_POINT('Ctrl Pts',(0.177112733230786,-0.0834343452077754,
1.2426769719476));
#25359=CARTESIAN_POINT('Ctrl Pts',(0.171231299791148,-0.0941328952695809,
1.24198052777377));
#25360=CARTESIAN_POINT('Ctrl Pts',(0.165362210352309,-0.104808991126666,
1.24128554530269));
#25361=CARTESIAN_POINT('Ctrl Pts',(0.158478065326005,-0.114957352860113,
1.2405905628316));
#25362=CARTESIAN_POINT('Ctrl Pts',(0.150699376209801,-0.124381903868597,
1.23989558036052));
#25363=CARTESIAN_POINT('Ctrl Pts',(0.142921783144072,-0.133805126917645,
1.23920069581543));
#25364=CARTESIAN_POINT('Ctrl Pts',(0.134250417229716,-0.142504038029514,
1.23850581127034));
#25365=CARTESIAN_POINT('Ctrl Pts',(0.124847281702347,-0.150314058728833,
1.23781092672525));
#25366=CARTESIAN_POINT('Ctrl Pts',(0.115444705137994,-0.158123615166766,
1.2371160834871));
#25367=CARTESIAN_POINT('Ctrl Pts',(0.105311136093151,-0.165043847112332,
1.23642124024895));
#25368=CARTESIAN_POINT('Ctrl Pts',(0.0946409745778109,-0.170951004474856,
1.23572639701081));
#25369=CARTESIAN_POINT('Ctrl Pts',(0.0839462210162306,-0.176871776353598,
1.23502995233326));
#25370=CARTESIAN_POINT('Ctrl Pts',(0.0727132031683232,-0.181774445238699,
1.23433350765571));
#25371=CARTESIAN_POINT('Ctrl Pts',(0.0611589772496136,-0.185582163749056,
1.23363706297816));
#25372=CARTESIAN_POINT('Ctrl Pts',(0.0573879160557474,-0.18682492458934,
1.23340975778994));
#25373=CARTESIAN_POINT('Ctrl Pts',(0.0535827550179384,-0.187951445986059,
1.23318245260173));
#25374=CARTESIAN_POINT('Ctrl Pts',(0.049751300876871,-0.188960228781241,
1.23295514741351));
#25375=CARTESIAN_POINT('Ctrl Pts',(0.0380120443523155,-0.192051055285797,
1.23225870323967));
#25376=CARTESIAN_POINT('Ctrl Pts',(0.0259421034513624,-0.194054676576599,
1.23156225906584));
#25377=CARTESIAN_POINT('Ctrl Pts',(0.0137638156624678,-0.194914641262296,
1.230865814892));
#25378=CARTESIAN_POINT('Ctrl Pts',(0.00161108776398865,-0.195772801047049,
1.23017083242092));
#25379=CARTESIAN_POINT('Ctrl Pts',(-0.010648676171227,-0.195491932984147,
1.22947584994983));
#25380=CARTESIAN_POINT('Ctrl Pts',(-0.0227853820001425,-0.194066963615932,
1.22878086747875));
#25381=CARTESIAN_POINT('Ctrl Pts',(-0.0349203777154394,-0.192642195031979,
1.22808598293366));
#25382=CARTESIAN_POINT('Ctrl Pts',(-0.0469314759806912,-0.190073701345935,
1.22739109838857));
#25383=CARTESIAN_POINT('Ctrl Pts',(-0.0585925475005012,-0.186408351147156,
1.22669621384348));
#25384=CARTESIAN_POINT('Ctrl Pts',(-0.0702529258358215,-0.182743218832635,
1.22600137060533));
#25385=CARTESIAN_POINT('Ctrl Pts',(-0.0815624912920071,-0.177981647562636,
1.22530652736718));
#25386=CARTESIAN_POINT('Ctrl Pts',(-0.0923118506849833,-0.172219865936289,
1.22461168412903));
#25387=CARTESIAN_POINT('Ctrl Pts',(-0.103085984655443,-0.166444804848336,
1.22391523945149));
#25388=CARTESIAN_POINT('Ctrl Pts',(-0.113296594269027,-0.159665401962586,
1.22321879477394));
#25389=CARTESIAN_POINT('Ctrl Pts',(-0.122761408172187,-0.152022355801973,
1.22252235009639));
#25390=CARTESIAN_POINT('Ctrl Pts',(-0.125850528349432,-0.149527823067158,
1.22229504490817));
#25391=CARTESIAN_POINT('Ctrl Pts',(-0.128860475478536,-0.146941605895026,
1.22206773971995));
#25392=CARTESIAN_POINT('Ctrl Pts',(-0.131785756567397,-0.144269450563724,
1.22184043453172));
#25393=CARTESIAN_POINT('Ctrl Pts',(-0.140615130944615,-0.13620408552787,
1.22115435940125));
#25394=CARTESIAN_POINT('Ctrl Pts',(-0.148736969234767,-0.127292292619823,
1.22046828427079));
#25395=CARTESIAN_POINT('Ctrl Pts',(-0.155985658870892,-0.11768446892693,
1.21978220914032));
#25396=CARTESIAN_POINT('Ctrl Pts',(-0.163222788613678,-0.108091967371237,
1.21909722813247));
#25397=CARTESIAN_POINT('Ctrl Pts',(-0.169588919704724,-0.0978062968135252,
1.21841224712463));
#25398=CARTESIAN_POINT('Ctrl Pts',(-0.174956910238458,-0.0870128700814545,
1.21772726611678));
#25399=CARTESIAN_POINT('Ctrl Pts',(-0.180319767440095,-0.0762297649480411,
1.21704294014642));
#25400=CARTESIAN_POINT('Ctrl Pts',(-0.184685958470788,-0.0649406667622732,
1.21635861417606));
#25401=CARTESIAN_POINT('Ctrl Pts',(-0.187974379745736,-0.0533553423679934,
1.21567428820569));
#25402=CARTESIAN_POINT('Ctrl Pts',(-0.19126753333635,-0.041753345714432,
1.21498897743252));
#25403=CARTESIAN_POINT('Ctrl Pts',(-0.193479596159008,-0.029855149983414,
1.21430366665935));
#25404=CARTESIAN_POINT('Ctrl Pts',(-0.194579881002083,-0.0178837890061103,
1.21361835588617));
#25405=CARTESIAN_POINT('Ctrl Pts',(-0.1951318539993,-0.0118781914183708,
1.21327456032826));
#25406=CARTESIAN_POINT('Ctrl Pts',(-0.195404848907981,-0.00585429143267565,
1.21293076477034));
#25407=CARTESIAN_POINT('Ctrl Pts',(-0.19539993476676,0.000159665732175137,
1.21258696921242));
#25408=CARTESIAN_POINT('',(-0.195593625707714,-0.000136366597080911,1.14258696921242));
#25409=CARTESIAN_POINT('Ctrl Pts',(-0.195527484430252,0.000159769955907059,
1.21258696921242));
#25410=CARTESIAN_POINT('Ctrl Pts',(-0.195623513973876,0.0110197689033327,
1.21196655335827));
#25411=CARTESIAN_POINT('Ctrl Pts',(-0.18985927784004,0.0866298604487836,
1.20764123321016));
#25412=CARTESIAN_POINT('Ctrl Pts',(-0.0912307526971303,0.212176946224813,
1.1996110087682));
#25413=CARTESIAN_POINT('Ctrl Pts',(0.128799216677344,0.191710376689535,
1.18849629588638));
#25414=CARTESIAN_POINT('Ctrl Pts',(0.230919855567683,-0.00425758753962621,
1.17738158300462));
#25415=CARTESIAN_POINT('Ctrl Pts',(0.121644755665287,-0.196327940360556,
1.16626687012284));
#25416=CARTESIAN_POINT('Ctrl Pts',(-0.0989901185229759,-0.208669746685701,
1.15515215724107));
#25417=CARTESIAN_POINT('Ctrl Pts',(-0.191321962564428,-0.0817735492630111,
1.1472588569376));
#25418=CARTESIAN_POINT('Ctrl Pts',(-0.195660812389172,-0.00859214891261325,
1.14307046092805));
#25419=CARTESIAN_POINT('Ctrl Pts',(-0.195593625707714,-0.000136366597080911,
1.14258696921242));
#25420=CARTESIAN_POINT('',(-0.195381487698991,-7.45427749785765E-5,1.07258697294116));
#25421=CARTESIAN_POINT('Ctrl Pts',(-0.195593625707714,-0.000136366597080911,
1.14258696921242));
#25422=CARTESIAN_POINT('Ctrl Pts',(-0.195145973734063,0.0562028893414784,
1.13936555663412));
#25423=CARTESIAN_POINT('Ctrl Pts',(-0.139964136507604,0.178102071649159,
1.1324392397619));
#25424=CARTESIAN_POINT('Ctrl Pts',(0.0669982713500039,0.221027913131385,
1.12180801859573));
#25425=CARTESIAN_POINT('Ctrl Pts',(0.222039400633985,0.0635658030166764,
1.11069330571397));
#25426=CARTESIAN_POINT('Ctrl Pts',(0.173814409632558,-0.152087664691053,
1.09957859283218));
#25427=CARTESIAN_POINT('Ctrl Pts',(-0.0335291008517759,-0.228512376345667,
1.08846387995042));
#25428=CARTESIAN_POINT('Ctrl Pts',(-0.176523953997762,-0.121039463917083,
1.07946669181885));
#25429=CARTESIAN_POINT('Ctrl Pts',(-0.195201636949265,-0.028014216980228,
1.07417440798122));
#25430=CARTESIAN_POINT('Ctrl Pts',(-0.195106173000238,-7.54145949441056E-5,
1.07258702843751));
#25431=CARTESIAN_POINT('',(-0.19539992140511,0.000175256603135645,1.00258696921242));
#25432=CARTESIAN_POINT('Ctrl Pts',(-0.195399985803746,-7.44841983129522E-5,
1.07258696921242));
#25433=CARTESIAN_POINT('Ctrl Pts',(-0.195404755662087,0.0124386430582194,
1.07187708757107));
#25434=CARTESIAN_POINT('Ctrl Pts',(-0.194203212211483,0.0249440138070227,
1.07116720592972));
#25435=CARTESIAN_POINT('Ctrl Pts',(-0.1918257233382,0.0372028475492977,
1.07045732428836));
#25436=CARTESIAN_POINT('Ctrl Pts',(-0.189439939565944,0.0495044515390223,
1.06974496591765));
#25437=CARTESIAN_POINT('Ctrl Pts',(-0.185870207066471,0.0615569932970218,
1.06903260754694));
#25438=CARTESIAN_POINT('Ctrl Pts',(-0.181197963915298,0.0731331516683816,
1.06832024917622));
#25439=CARTESIAN_POINT('Ctrl Pts',(-0.176637833436752,0.0844315346732244,
1.06762498417977));
#25440=CARTESIAN_POINT('Ctrl Pts',(-0.171028039873804,0.0952755705208773,
1.06692971918331));
#25441=CARTESIAN_POINT('Ctrl Pts',(-0.16448631462972,0.105477070017767,
1.06623445418686));
#25442=CARTESIAN_POINT('Ctrl Pts',(-0.157933494544858,0.115695871374393,
1.06553801001302));
#25443=CARTESIAN_POINT('Ctrl Pts',(-0.15040156397909,0.125337862537118,
1.06484156583919));
#25444=CARTESIAN_POINT('Ctrl Pts',(-0.142016043722388,0.13421104025169,
1.06414512166535));
#25445=CARTESIAN_POINT('Ctrl Pts',(-0.133648123064461,0.143065594868009,
1.06345013919427));
#25446=CARTESIAN_POINT('Ctrl Pts',(-0.124430709813014,0.151153857448322,
1.06275515672319));
#25447=CARTESIAN_POINT('Ctrl Pts',(-0.114529799123765,0.158316408223121,
1.0620601742521));
#25448=CARTESIAN_POINT('Ctrl Pts',(-0.10463028351506,0.165477949763969,
1.06136528970701));
#25449=CARTESIAN_POINT('Ctrl Pts',(-0.0940481430551521,0.17171348860514,
1.06067040516192));
#25450=CARTESIAN_POINT('Ctrl Pts',(-0.082981597919551,0.17690453472627,
1.05997552061683));
#25451=CARTESIAN_POINT('Ctrl Pts',(-0.0719157106272202,0.182095272269183,
1.05928067737868));
#25452=CARTESIAN_POINT('Ctrl Pts',(-0.0603662800455644,0.186241292651039,
1.05858583414053));
#25453=CARTESIAN_POINT('Ctrl Pts',(-0.0485526003242364,0.189271775502199,
1.05789099090239));
#25454=CARTESIAN_POINT('Ctrl Pts',(-0.0367116930340006,0.192309242856292,
1.05719454622484));
#25455=CARTESIAN_POINT('Ctrl Pts',(-0.0246061846279033,0.194225885336874,
1.05649810154729));
#25456=CARTESIAN_POINT('Ctrl Pts',(-0.0124654871113448,0.195001978531185,
1.05580165686974));
#25457=CARTESIAN_POINT('Ctrl Pts',(-0.00850301367579334,0.195255279353628,
1.05557435168152));
#25458=CARTESIAN_POINT('Ctrl Pts',(-0.00453680405894013,0.195387499836847,
1.0553470464933));
#25459=CARTESIAN_POINT('Ctrl Pts',(-0.000574790968387507,0.19539915459219,
1.05511974130508));
#25460=CARTESIAN_POINT('Ctrl Pts',(0.0115644873085008,0.195434863792319,
1.05442329713125));
#25461=CARTESIAN_POINT('Ctrl Pts',(0.0237500757245702,0.194335133560062,
1.05372685295741));
#25462=CARTESIAN_POINT('Ctrl Pts',(0.0357525861558755,0.192101308124559,
1.05303040878358));
#25463=CARTESIAN_POINT('Ctrl Pts',(0.0477299056197295,0.189872171060223,
1.05233542631249));
#25464=CARTESIAN_POINT('Ctrl Pts',(0.0595240438404298,0.186513748477051,
1.05164044384141));
#25465=CARTESIAN_POINT('Ctrl Pts',(0.0709110411567376,0.182079060416258,
1.05094546137032));
#25466=CARTESIAN_POINT('Ctrl Pts',(0.0822964339965533,0.177644997221929,
1.05025057682523));
#25467=CARTESIAN_POINT('Ctrl Pts',(0.093273968340728,0.172135243953825,
1.04955569228014));
#25468=CARTESIAN_POINT('Ctrl Pts',(0.103636598944045,0.165652091321876,
1.04886080773505));
#25469=CARTESIAN_POINT('Ctrl Pts',(0.113998613547812,0.159169324076539,
1.04816596449691));
#25470=CARTESIAN_POINT('Ctrl Pts',(0.123745068727093,0.151713759496613,
1.04747112125876));
#25471=CARTESIAN_POINT('Ctrl Pts',(0.132697543456127,0.14343124471575,1.04677627802061));
#25472=CARTESIAN_POINT('Ctrl Pts',(0.14167065139415,0.135129640815553,1.04607983334306));
#25473=CARTESIAN_POINT('Ctrl Pts',(0.149845527317485,0.125997923791544,
1.04538338866551));
#25474=CARTESIAN_POINT('Ctrl Pts',(0.157081194432025,0.116218149855383,
1.04468694398796));
#25475=CARTESIAN_POINT('Ctrl Pts',(0.159442767042723,0.1130262332151,1.04445963879974));
#25476=CARTESIAN_POINT('Ctrl Pts',(0.161704633833709,0.109765518630711,
1.04423233361152));
#25477=CARTESIAN_POINT('Ctrl Pts',(0.163862925475782,0.106442950234003,
1.04400502842331));
#25478=CARTESIAN_POINT('Ctrl Pts',(0.170475751392048,0.0962628772660957,
1.04330858424947));
#25479=CARTESIAN_POINT('Ctrl Pts',(0.176159692457368,0.0854281744277342,
1.04261214007564));
#25480=CARTESIAN_POINT('Ctrl Pts',(0.180791486727862,0.0741323028559712,
1.0419156959018));
#25481=CARTESIAN_POINT('Ctrl Pts',(0.185413559750507,0.0628601391522177,
1.04122071343072));
#25482=CARTESIAN_POINT('Ctrl Pts',(0.188987471086921,0.0511295016428723,
1.04052573095963));
#25483=CARTESIAN_POINT('Ctrl Pts',(0.191436320594509,0.0391573129470908,
1.03983074848855));
#25484=CARTESIAN_POINT('Ctrl Pts',(0.193884825048757,0.0271868111837602,
1.03913586394346));
#25485=CARTESIAN_POINT('Ctrl Pts',(0.195208361997676,0.0149756731820053,
1.03844097939837));
#25486=CARTESIAN_POINT('Ctrl Pts',(0.195380600836856,0.0027533282820952,
1.03774609485328));
#25487=CARTESIAN_POINT('Ctrl Pts',(0.195552829437415,-0.00946829006880504,
1.03705125161513));
#25488=CARTESIAN_POINT('Ctrl Pts',(0.19457391019337,-0.0217002379464254,
1.03635640837698));
#25489=CARTESIAN_POINT('Ctrl Pts',(0.192469630852204,-0.0337135165714957,
1.03566156513883));
#25490=CARTESIAN_POINT('Ctrl Pts',(0.190360501674904,-0.0457544827908924,
1.03496512046129));
#25491=CARTESIAN_POINT('Ctrl Pts',(0.187121049392968,-0.0575749227607743,
1.03426867578374));
#25492=CARTESIAN_POINT('Ctrl Pts',(0.182827789725607,-0.0689576631278162,
1.03357223110619));
#25493=CARTESIAN_POINT('Ctrl Pts',(0.181426558259242,-0.0726727549721334,
1.03334492591797));
#25494=CARTESIAN_POINT('Ctrl Pts',(0.179913454732605,-0.076341381240727,
1.03311762072975));
#25495=CARTESIAN_POINT('Ctrl Pts',(0.178292215374938,-0.0799565252915397,
1.03289031554153));
#25496=CARTESIAN_POINT('Ctrl Pts',(0.173324872949159,-0.0910330257070951,
1.0321938713677));
#25497=CARTESIAN_POINT('Ctrl Pts',(0.167303798950699,-0.101684065071151,
1.03149742719386));
#25498=CARTESIAN_POINT('Ctrl Pts',(0.160324697846078,-0.111701169468202,
1.03080098302003));
#25499=CARTESIAN_POINT('Ctrl Pts',(0.153360244536167,-0.121697249884283,
1.03010600054894));
#25500=CARTESIAN_POINT('Ctrl Pts',(0.145442189425305,-0.131061282235646,
1.02941101807786));
#25501=CARTESIAN_POINT('Ctrl Pts',(0.136711090177366,-0.139611023284395,
1.02871603560678));
#25502=CARTESIAN_POINT('Ctrl Pts',(0.12798122117855,-0.148159559638166,
1.02802115106169));
#25503=CARTESIAN_POINT('Ctrl Pts',(0.118439127932392,-0.155893387786925,
1.0273262665166));
#25504=CARTESIAN_POINT('Ctrl Pts',(0.108263298844997,-0.162665971005613,
1.02663138197151));
#25505=CARTESIAN_POINT('Ctrl Pts',(0.0980880746528624,-0.169438151632684,
1.02593653873336));
#25506=CARTESIAN_POINT('Ctrl Pts',(0.0872799332730697,-0.175248737806347,
1.02524169549521));
#25507=CARTESIAN_POINT('Ctrl Pts',(0.0760452638153761,-0.179995216189903,
1.02454685225706));
#25508=CARTESIAN_POINT('Ctrl Pts',(0.0647847012622126,-0.184752634015727,
1.02385040757951));
#25509=CARTESIAN_POINT('Ctrl Pts',(0.0530964795691645,-0.188440767123773,
1.02315396290196));
#25510=CARTESIAN_POINT('Ctrl Pts',(0.0412045606015807,-0.191006136513021,
1.02245751822441));
#25511=CARTESIAN_POINT('Ctrl Pts',(0.0373232833567963,-0.191843420206434,
1.02223021303619));
#25512=CARTESIAN_POINT('Ctrl Pts',(0.0334203811648193,-0.192561511747185,
1.02200290784797));
#25513=CARTESIAN_POINT('Ctrl Pts',(0.029503775479741,-0.193159745372686,
1.02177560265975));
#25514=CARTESIAN_POINT('Ctrl Pts',(0.0175036217131327,-0.19499268339903,
1.02107915848592));
#25515=CARTESIAN_POINT('Ctrl Pts',(0.00528952893680135,-0.195709558060808,
1.02038271431208));
#25516=CARTESIAN_POINT('Ctrl Pts',(-0.00691144469128197,-0.195277730251761,
1.01968627013825));
#25517=CARTESIAN_POINT('Ctrl Pts',(-0.0190868108157334,-0.194846808766465,
1.01899128766716));
#25518=CARTESIAN_POINT('Ctrl Pts',(-0.0312482434387783,-0.193271926176745,
1.01829630519608));
#25519=CARTESIAN_POINT('Ctrl Pts',(-0.0431664006990371,-0.190572353322013,
1.01760132272499));
#25520=CARTESIAN_POINT('Ctrl Pts',(-0.0550828786400965,-0.187873160848612,
1.0169064381799));
#25521=CARTESIAN_POINT('Ctrl Pts',(-0.0667552863310145,-0.184049740907001,
1.01621155363481));
#25522=CARTESIAN_POINT('Ctrl Pts',(-0.0779637136878998,-0.179172596531923,
1.01551666908972));
#25523=CARTESIAN_POINT('Ctrl Pts',(-0.0891714747674275,-0.174295742075382,
1.01482182585157));
#25524=CARTESIAN_POINT('Ctrl Pts',(-0.0999145179078746,-0.16836566148151,
1.01412698261342));
#25525=CARTESIAN_POINT('Ctrl Pts',(-0.10999479168807,-0.161500172759964,
1.01343213937528));
#25526=CARTESIAN_POINT('Ctrl Pts',(-0.120098297971212,-0.154618860808768,
1.01273569469773));
#25527=CARTESIAN_POINT('Ctrl Pts',(-0.129535298579093,-0.14679838309348,
1.01203925002018));
#25528=CARTESIAN_POINT('Ctrl Pts',(-0.138139411542142,-0.138197912353229,
1.01134280534263));
#25529=CARTESIAN_POINT('Ctrl Pts',(-0.140947616672534,-0.135390895969288,
1.01111550015441));
#25530=CARTESIAN_POINT('Ctrl Pts',(-0.143667403064424,-0.132501075392946,
1.0108881949662));
#25531=CARTESIAN_POINT('Ctrl Pts',(-0.146293915739412,-0.129534745213899,
1.01066088977798));
#25532=CARTESIAN_POINT('Ctrl Pts',(-0.154268340861462,-0.12052859111255,
1.00997076243895));
#25533=CARTESIAN_POINT('Ctrl Pts',(-0.161438925506145,-0.11074811353596,
1.00928063509993));
#25534=CARTESIAN_POINT('Ctrl Pts',(-0.167655952100067,-0.100362551409478,
1.0085905077609));
#25535=CARTESIAN_POINT('Ctrl Pts',(-0.173860147416604,-0.0899984239714956,
1.00790180477083));
#25536=CARTESIAN_POINT('Ctrl Pts',(-0.17911416591557,-0.079032407179903,
1.00721310178076));
#25537=CARTESIAN_POINT('Ctrl Pts',(-0.183310450496771,-0.0676641614052141,
1.00652439879068));
#25538=CARTESIAN_POINT('Ctrl Pts',(-0.187507835192076,-0.0562929352874952,
1.00583551524759));
#25539=CARTESIAN_POINT('Ctrl Pts',(-0.190646574248882,-0.0445200902450065,
1.00514663170449));
#25540=CARTESIAN_POINT('Ctrl Pts',(-0.192667192514708,-0.0325655174763189,
1.00445774816139));
#25541=CARTESIAN_POINT('Ctrl Pts',(-0.194496301925863,-0.0217439674946309,
1.0038341551784));
#25542=CARTESIAN_POINT('Ctrl Pts',(-0.195409742132129,-0.0107742269164684,
1.00321056219541));
#25543=CARTESIAN_POINT('Ctrl Pts',(-0.19539992140511,0.000175256603135645,
1.00258696921242));
#25544=CARTESIAN_POINT('',(-0.195715067010162,-2.931307771456E-5,0.932586969212424));
#25545=CARTESIAN_POINT('Ctrl Pts',(-0.195321343181372,0.000175890211630183,
1.00258692909733));
#25546=CARTESIAN_POINT('Ctrl Pts',(-0.195476088018098,0.017966105673101,
1.00157334503028));
#25547=CARTESIAN_POINT('Ctrl Pts',(-0.185092782119974,0.100606533622347,
0.996854856669318));
#25548=CARTESIAN_POINT('Ctrl Pts',(-0.0682974629270655,0.220629923865294,
0.988431464014426));
#25549=CARTESIAN_POINT('Ctrl Pts',(0.148337561234701,0.177025632816321,
0.97731675113265));
#25550=CARTESIAN_POINT('Ctrl Pts',(0.229176864102385,-0.0286368941625076,
0.966202038250874));
#25551=CARTESIAN_POINT('Ctrl Pts',(0.100216050899271,-0.208083756908689,
0.955087325369096));
#25552=CARTESIAN_POINT('Ctrl Pts',(-0.120487614241236,-0.197040202906743,
0.943972612487321));
#25553=CARTESIAN_POINT('Ctrl Pts',(-0.194986802068985,-0.0678687340701233,
0.93647249376843));
#25554=CARTESIAN_POINT('Ctrl Pts',(-0.195718367640748,-0.0016061582711675,
0.932677279343464));
#25555=CARTESIAN_POINT('Ctrl Pts',(-0.195715067010162,-2.931307771456E-5,
0.932586969212424));
#25556=CARTESIAN_POINT('',(-0.195399936896884,-0.000157037236289389,0.862586969212423));
#25557=CARTESIAN_POINT('Ctrl Pts',(-0.195715067010162,-2.931307771456E-5,
0.932586969212424));
#25558=CARTESIAN_POINT('Ctrl Pts',(-0.195582961786627,0.0630827139603783,
0.928972375049538));
#25559=CARTESIAN_POINT('Ctrl Pts',(-0.128138062480741,0.191126119272836,
0.921652876592728));
#25560=CARTESIAN_POINT('Ctrl Pts',(0.0899808947771039,0.212710002872902,
0.910628473841993));
#25561=CARTESIAN_POINT('Ctrl Pts',(0.227513576082653,0.0397451814080767,
0.899513760960215));
#25562=CARTESIAN_POINT('Ctrl Pts',(0.156768799466018,-0.16960439340141,
0.888399048078441));
#25563=CARTESIAN_POINT('Ctrl Pts',(-0.0574900812163511,-0.223689510949474,
0.877284335196663));
#25564=CARTESIAN_POINT('Ctrl Pts',(-0.182608995805481,-0.107037763309046,
0.868680334011459));
#25565=CARTESIAN_POINT('Ctrl Pts',(-0.195393515914344,-0.0211417834289091,
0.86378123712018));
#25566=CARTESIAN_POINT('Ctrl Pts',(-0.195235485275365,-0.000158228367462752,
0.862587044522825));
#25567=CARTESIAN_POINT('',(-0.195399964130102,0.000118397444788799,0.792586969212424));
#25568=CARTESIAN_POINT('Ctrl Pts',(-0.195399936896884,-0.000157037236289389,
0.862586969212423));
#25569=CARTESIAN_POINT('Ctrl Pts',(-0.195409734496894,0.0120340231065371,
0.861893744600403));
#25570=CARTESIAN_POINT('Ctrl Pts',(-0.194274282005615,0.0242406068532915,
0.861200519988384));
#25571=CARTESIAN_POINT('Ctrl Pts',(-0.19201123716182,0.0362332002945821,
0.860507295376365));
#25572=CARTESIAN_POINT('Ctrl Pts',(-0.18974885363775,0.048222289192595,
0.85981427334235));
#25573=CARTESIAN_POINT('Ctrl Pts',(-0.186359709838977,0.0599966493212796,
0.859121251308335));
#25574=CARTESIAN_POINT('Ctrl Pts',(-0.181912610531916,0.0713369618743564,
0.858428229274321));
#25575=CARTESIAN_POINT('Ctrl Pts',(-0.177454434501244,0.0827055205940107,
0.857733481078376));
#25576=CARTESIAN_POINT('Ctrl Pts',(-0.171933407141078,0.0936370683755064,
0.85703873288243));
#25577=CARTESIAN_POINT('Ctrl Pts',(-0.165466127853881,0.103933250372743,
0.856343984686485));
#25578=CARTESIAN_POINT('Ctrl Pts',(-0.161466208777956,0.110301290618271,
0.85591429293536));
#25579=CARTESIAN_POINT('Ctrl Pts',(-0.157105246349051,0.116426790052616,
0.855484601184236));
#25580=CARTESIAN_POINT('Ctrl Pts',(-0.152418652238814,0.1222690248988,0.855054909433111));
#25581=CARTESIAN_POINT('Ctrl Pts',(-0.144822622865053,0.131738116195417,
0.854358465259276));
#25582=CARTESIAN_POINT('Ctrl Pts',(-0.136313921779505,0.140530156770072,
0.853662021085441));
#25583=CARTESIAN_POINT('Ctrl Pts',(-0.12703765742528,0.148467483294818,
0.852965576911606));
#25584=CARTESIAN_POINT('Ctrl Pts',(-0.117780862170854,0.156388150893478,
0.852270594440521));
#25585=CARTESIAN_POINT('Ctrl Pts',(-0.107760311345287,0.163457044708525,
0.851575611969437));
#25586=CARTESIAN_POINT('Ctrl Pts',(-0.0971579177599562,0.169533179692205,
0.850880629498353));
#25587=CARTESIAN_POINT('Ctrl Pts',(-0.0865570180971057,0.175608458522548,
0.850185744953263));
#25588=CARTESIAN_POINT('Ctrl Pts',(-0.0753751741160683,0.180690781469455,
0.849490860408173));
#25589=CARTESIAN_POINT('Ctrl Pts',(-0.0638220178270438,0.184683269519696,
0.848795975863083));
#25590=CARTESIAN_POINT('Ctrl Pts',(-0.0522695483075639,0.18867552023919,
0.848101132624934));
#25591=CARTESIAN_POINT('Ctrl Pts',(-0.0403466467615257,0.191577803907368,
0.847406289386786));
#25592=CARTESIAN_POINT('Ctrl Pts',(-0.0282788635343871,0.193342871286229,
0.846711446148637));
#25593=CARTESIAN_POINT('Ctrl Pts',(-0.016183267093484,0.195112006702725,
0.846015001471089));
#25594=CARTESIAN_POINT('Ctrl Pts',(-0.00394299772200419,0.195738630897938,
0.845318556793542));
#25595=CARTESIAN_POINT('Ctrl Pts',(0.00821173275305,0.19522737370869,0.844622112115994));
#25596=CARTESIAN_POINT('Ctrl Pts',(0.0121787862570268,0.195060509899723,
0.844394806927775));
#25597=CARTESIAN_POINT('Ctrl Pts',(0.0161367594936829,0.194772848920495,
0.844167501739555));
#25598=CARTESIAN_POINT('Ctrl Pts',(0.0200778185584785,0.194365740813377,
0.843940196551335));
#25599=CARTESIAN_POINT('Ctrl Pts',(0.0321528954448271,0.193118395464401,
0.8432437523775));
#25600=CARTESIAN_POINT('Ctrl Pts',(0.0441540321893043,0.190737074723704,
0.842547308203665));
#25601=CARTESIAN_POINT('Ctrl Pts',(0.0558532672044756,0.187247356570354,
0.841850864029829));
#25602=CARTESIAN_POINT('Ctrl Pts',(0.067527947769125,0.183764962666122,
0.841155881558745));
#25603=CARTESIAN_POINT('Ctrl Pts',(0.0789011322020904,0.179178965013493,
0.84046089908766));
#25604=CARTESIAN_POINT('Ctrl Pts',(0.0897557179776617,0.173565754370828,
0.839765916616576));
#25605=CARTESIAN_POINT('Ctrl Pts',(0.100608774295799,0.167953334653484,
0.839071032071486));
#25606=CARTESIAN_POINT('Ctrl Pts',(0.11094257919104,0.161314349961526,0.838376147526397));
#25607=CARTESIAN_POINT('Ctrl Pts',(0.120562056665277,0.153772398344562,
0.837681262981307));
#25608=CARTESIAN_POINT('Ctrl Pts',(0.130180962316199,0.146230895053796,
0.836986419743158));
#25609=CARTESIAN_POINT('Ctrl Pts',(0.139084952155297,0.137787092787488,
0.836291576505009));
#25610=CARTESIAN_POINT('Ctrl Pts',(0.147112017075362,0.128604877170418,
0.835596733266859));
#25611=CARTESIAN_POINT('Ctrl Pts',(0.155157582366897,0.119401498849231,
0.834900288589311));
#25612=CARTESIAN_POINT('Ctrl Pts',(0.162321660730657,0.109457011262306,
0.834203843911763));
#25613=CARTESIAN_POINT('Ctrl Pts',(0.168483304121249,0.0989673493248495,
0.833507399234215));
#25614=CARTESIAN_POINT('Ctrl Pts',(0.170494337525317,0.0955437398725704,
0.833280094045996));
#25615=CARTESIAN_POINT('Ctrl Pts',(0.172398952993282,0.0920622544280945,
0.833052788857778));
#25616=CARTESIAN_POINT('Ctrl Pts',(0.174194036704551,0.08853020714182,0.832825483669559));
#25617=CARTESIAN_POINT('Ctrl Pts',(0.179694023757454,0.0777083082950995,
0.832129039495724));
#25618=CARTESIAN_POINT('Ctrl Pts',(0.184201147367978,0.066333607930296,
0.831432595321889));
#25619=CARTESIAN_POINT('Ctrl Pts',(0.187613280394586,0.0546115099551607,
0.830736151148054));
#25620=CARTESIAN_POINT('Ctrl Pts',(0.191018252008375,0.0429140144155199,
0.83004116867697));
#25621=CARTESIAN_POINT('Ctrl Pts',(0.193332480626411,0.0308713799645606,
0.829346186205886));
#25622=CARTESIAN_POINT('Ctrl Pts',(0.194502420663427,0.0187074411950771,
0.828651203734802));
#25623=CARTESIAN_POINT('Ctrl Pts',(0.195672195850902,0.00654521637644226,
0.827956319189712));
#25624=CARTESIAN_POINT('Ctrl Pts',(0.195697872942552,-0.00573741290396437,
0.827261434644622));
#25625=CARTESIAN_POINT('Ctrl Pts',(0.194577514407471,-0.0179095194522505,
0.826566550099533));
#25626=CARTESIAN_POINT('Ctrl Pts',(0.193457222471343,-0.0300809024379134,
0.825871706861383));
#25627=CARTESIAN_POINT('Ctrl Pts',(0.191191137051048,-0.0421409061126653,
0.825176863623234));
#25628=CARTESIAN_POINT('Ctrl Pts',(0.18782910162498,-0.0538645391955886,
0.824482020385085));
#25629=CARTESIAN_POINT('Ctrl Pts',(0.184459317550445,-0.0656151923125061,
0.823785575707537));
#25630=CARTESIAN_POINT('Ctrl Pts',(0.179988844497181,-0.0770271037583809,
0.82308913102999));
#25631=CARTESIAN_POINT('Ctrl Pts',(0.174516720171798,-0.0878924022909733,
0.822392686352442));
#25632=CARTESIAN_POINT('Ctrl Pts',(0.172730731578815,-0.0914386117856203,
0.822165381164222));
#25633=CARTESIAN_POINT('Ctrl Pts',(0.170838407752911,-0.0949267934779921,
0.821938075976002));
#25634=CARTESIAN_POINT('Ctrl Pts',(0.168844205506616,-0.0983503648536164,
0.821710770787783));
#25635=CARTESIAN_POINT('Ctrl Pts',(0.162734135838796,-0.108839902540525,
0.821014326613947));
#25636=CARTESIAN_POINT('Ctrl Pts',(0.15562119694151,-0.118795005346275,
0.820317882440112));
#25637=CARTESIAN_POINT('Ctrl Pts',(0.147622588480279,-0.128018480581446,
0.819621438266277));
#25638=CARTESIAN_POINT('Ctrl Pts',(0.139640767564166,-0.137222597511057,
0.818926455795193));
#25639=CARTESIAN_POINT('Ctrl Pts',(0.130777478205338,-0.145697430863864,
0.818231473324109));
#25640=CARTESIAN_POINT('Ctrl Pts',(0.121191750101413,-0.153276611742811,
0.817536490853024));
#25641=CARTESIAN_POINT('Ctrl Pts',(0.111607372667467,-0.160854724682844,
0.816841606307935));
#25642=CARTESIAN_POINT('Ctrl Pts',(0.101301415844516,-0.167536857225407,
0.816146721762845));
#25643=CARTESIAN_POINT('Ctrl Pts',(0.0904668542828406,-0.173196155488993,
0.815451837217755));
#25644=CARTESIAN_POINT('Ctrl Pts',(0.0796329367743329,-0.178855117339429,
0.814756993979606));
#25645=CARTESIAN_POINT('Ctrl Pts',(0.0682712655334758,-0.183490983858409,
0.814062150741457));
#25646=CARTESIAN_POINT('Ctrl Pts',(0.0565979073780773,-0.187023626529972,
0.813367307503308));
#25647=CARTESIAN_POINT('Ctrl Pts',(0.0448976450597862,-0.190564411056914,
0.812670862825761));
#25648=CARTESIAN_POINT('Ctrl Pts',(0.0328851181857995,-0.192996704269116,
0.811974418148213));
#25649=CARTESIAN_POINT('Ctrl Pts',(0.0207886860788731,-0.194290994467356,
0.811277973470666));
#25650=CARTESIAN_POINT('Ctrl Pts',(0.0168406599606547,-0.19471342411124,
0.811050668282446));
#25651=CARTESIAN_POINT('Ctrl Pts',(0.0128837259739765,-0.195015043749426,
0.810823363094226));
#25652=CARTESIAN_POINT('Ctrl Pts',(0.00892583157243448,-0.195196028470716,
0.810596057906007));
#25653=CARTESIAN_POINT('Ctrl Pts',(-0.00320082738417567,-0.195750550589998,
0.809899613732172));
#25654=CARTESIAN_POINT('Ctrl Pts',(-0.0154222840393251,-0.195172650204224,
0.809203169558337));
#25655=CARTESIAN_POINT('Ctrl Pts',(-0.0275093024339257,-0.193453866023915,
0.808506725384502));
#25656=CARTESIAN_POINT('Ctrl Pts',(-0.0395709524950678,-0.191738689241957,
0.807811742913417));
#25657=CARTESIAN_POINT('Ctrl Pts',(-0.0514978555606483,-0.188887429541335,
0.807116760442333));
#25658=CARTESIAN_POINT('Ctrl Pts',(-0.0630639904949814,-0.184943486240659,
0.806421777971249));
#25659=CARTESIAN_POINT('Ctrl Pts',(-0.0746284957115704,-0.181000098658416,
0.805726893426159));
#25660=CARTESIAN_POINT('Ctrl Pts',(-0.0858314912680433,-0.175964571683546,
0.805032008881069));
#25661=CARTESIAN_POINT('Ctrl Pts',(-0.0964617491077431,-0.169930253219004,
0.804337124335979));
#25662=CARTESIAN_POINT('Ctrl Pts',(-0.10709137503898,-0.163896293460428,
0.80364228109783));
#25663=CARTESIAN_POINT('Ctrl Pts',(-0.117147582437623,-0.156864115666681,
0.80294743785968));
#25664=CARTESIAN_POINT('Ctrl Pts',(-0.126445879661726,-0.14897180779118,
0.80225259462153));
#25665=CARTESIAN_POINT('Ctrl Pts',(-0.135765607128928,-0.141061310125409,
0.801556149943982));
#25666=CARTESIAN_POINT('Ctrl Pts',(-0.144323311928957,-0.132287340628995,
0.800859705266435));
#25667=CARTESIAN_POINT('Ctrl Pts',(-0.1519703648202,-0.122825763650853,
0.800163260588887));
#25668=CARTESIAN_POINT('Ctrl Pts',(-0.154466205269271,-0.119737699939265,
0.799935955400668));
#25669=CARTESIAN_POINT('Ctrl Pts',(-0.156865371508102,-0.116576639620415,
0.79970865021245));
#25670=CARTESIAN_POINT('Ctrl Pts',(-0.159163700943832,-0.11334935510122,
0.799481345024231));
#25671=CARTESIAN_POINT('Ctrl Pts',(-0.16627106320176,-0.103369288784035,
0.798778425638236));
#25672=CARTESIAN_POINT('Ctrl Pts',(-0.17246084605519,-0.092683670684521,
0.79807550625224));
#25673=CARTESIAN_POINT('Ctrl Pts',(-0.177599482383803,-0.0814836416528211,
0.797372586866245));
#25674=CARTESIAN_POINT('Ctrl Pts',(-0.18272618655519,-0.070309619619629,
0.796671299692396));
#25675=CARTESIAN_POINT('Ctrl Pts',(-0.186806164619108,-0.0586242921696647,
0.795970012518547));
#25676=CARTESIAN_POINT('Ctrl Pts',(-0.189751053307921,-0.0466443755294713,
0.795268725344698));
#25677=CARTESIAN_POINT('Ctrl Pts',(-0.192692582140228,-0.0346781269104265,
0.794568238277245));
#25678=CARTESIAN_POINT('Ctrl Pts',(-0.194501349927928,-0.0224187725981258,
0.793867751209792));
#25679=CARTESIAN_POINT('Ctrl Pts',(-0.195138918234439,-0.0100976527120339,
0.793167264142338));
#25680=CARTESIAN_POINT('Ctrl Pts',(-0.19531497556794,-0.00669531371441858,
0.792973832499034));
#25681=CARTESIAN_POINT('Ctrl Pts',(-0.195402028337336,-0.00328831475456294,
0.792780400855729));
#25682=CARTESIAN_POINT('Ctrl Pts',(-0.195399964130102,0.000118397444788799,
0.792586969212424));
#25683=CARTESIAN_POINT('',(-0.195665606136028,9.31787759667347E-5,0.722586969212424));
#25684=CARTESIAN_POINT('Ctrl Pts',(-0.195153759558878,0.000119703465488583,
0.792586886482477));
#25685=CARTESIAN_POINT('Ctrl Pts',(-0.195290253173666,0.024864238661261,
0.791180135035802));
#25686=CARTESIAN_POINT('Ctrl Pts',(-0.179437438454886,0.114608714513428,
0.786068479295203));
#25687=CARTESIAN_POINT('Ctrl Pts',(-0.0445992966086936,0.226612024149397,
0.777251919260677));
#25688=CARTESIAN_POINT('Ctrl Pts',(0.166214644641796,0.16035834450904,0.766137206378902));
#25689=CARTESIAN_POINT('Ctrl Pts',(0.224867276437698,-0.0526954906473987,
0.755022493497125));
#25690=CARTESIAN_POINT('Ctrl Pts',(0.0776650071207437,-0.217509203060494,
0.74390778061535));
#25691=CARTESIAN_POINT('Ctrl Pts',(-0.134687138099445,-0.184138771498097,
0.733095939187116));
#25692=CARTESIAN_POINT('Ctrl Pts',(-0.195315412358655,-0.0593474407707721,
0.725989002052807));
#25693=CARTESIAN_POINT('Ctrl Pts',(-0.195665606136028,9.31787759667347E-5,
0.722586969212424));
#25694=CARTESIAN_POINT('',(-0.195399920232252,-0.000176559421619332,0.652586969212424));
#25695=CARTESIAN_POINT('Ctrl Pts',(-0.195665606136028,9.31787759667347E-5,
0.722586969212424));
#25696=CARTESIAN_POINT('Ctrl Pts',(-0.195696782701144,0.0053849756768864,
0.722284097758882));
#25697=CARTESIAN_POINT('Ctrl Pts',(-0.19310225815126,0.0753781479809831,
0.718276322011416));
#25698=CARTESIAN_POINT('Ctrl Pts',(-0.109018190962289,0.203610266898278,
0.71056364197002));
#25699=CARTESIAN_POINT('Ctrl Pts',(0.111955804692466,0.202009911991322,
0.699448929088245));
#25700=CARTESIAN_POINT('Ctrl Pts',(0.230439782817406,0.015479445795746,
0.688334216206469));
#25701=CARTESIAN_POINT('Ctrl Pts',(0.137967505075176,-0.185221689578759,
0.677219503324693));
#25702=CARTESIAN_POINT('Ctrl Pts',(-0.080807218998807,-0.216361503287337,
0.666104790442915));
#25703=CARTESIAN_POINT('Ctrl Pts',(-0.18777605090878,-0.0930453392534147,
0.657893945738827));
#25704=CARTESIAN_POINT('Ctrl Pts',(-0.195562463745895,-0.0142157590911969,
0.653388005328663));
#25705=CARTESIAN_POINT('Ctrl Pts',(-0.195432764861167,-0.000176589099362662,
0.652586969212424));
#25706=CARTESIAN_POINT('',(-0.195368572466251,1.52014745227871E-5,0.582586968017739));
#25707=CARTESIAN_POINT('Ctrl Pts',(-0.195399920232252,-0.000176559421619332,
0.652586969212424));
#25708=CARTESIAN_POINT('Ctrl Pts',(-0.195410776640569,0.0118383265557513,
0.651901311615086));
#25709=CARTESIAN_POINT('Ctrl Pts',(-0.19430915187813,0.0238869003000631,
0.651215654017748));
#25710=CARTESIAN_POINT('Ctrl Pts',(-0.192102813592723,0.0357444962163329,
0.65052999642041));
#25711=CARTESIAN_POINT('Ctrl Pts',(-0.189897203385873,0.0475981791962381,
0.649844565086015));
#25712=CARTESIAN_POINT('Ctrl Pts',(-0.18658771446154,0.0592601148205221,
0.649159133751619));
#25713=CARTESIAN_POINT('Ctrl Pts',(-0.182233720267025,0.0705126314757841,
0.648473702417224));
#25714=CARTESIAN_POINT('Ctrl Pts',(-0.177880280221303,0.081763715982024,
0.647788358320186));
#25715=CARTESIAN_POINT('Ctrl Pts',(-0.172482949831443,0.0926046537378351,
0.647103014223148));
#25716=CARTESIAN_POINT('Ctrl Pts',(-0.166149261678216,0.10283765285042,
0.646417670126111));
#25717=CARTESIAN_POINT('Ctrl Pts',(-0.159801609071076,0.11309321357972,
0.645730814989087));
#25718=CARTESIAN_POINT('Ctrl Pts',(-0.152514017080856,0.122737435692944,
0.645043959852063));
#25719=CARTESIAN_POINT('Ctrl Pts',(-0.144436353403315,0.131602810819346,
0.644357104715039));
#25720=CARTESIAN_POINT('Ctrl Pts',(-0.142547874655067,0.133675448798569,
0.644196524703148));
#25721=CARTESIAN_POINT('Ctrl Pts',(-0.14061636936524,0.135705677700539,
0.644035944691256));
#25722=CARTESIAN_POINT('Ctrl Pts',(-0.138644023767034,0.137691665229549,
0.643875364679365));
#25723=CARTESIAN_POINT('Ctrl Pts',(-0.130089854512213,0.146305000274161,
0.643178920505529));
#25724=CARTESIAN_POINT('Ctrl Pts',(-0.120699673502432,0.154148626491242,
0.642482476331694));
#25725=CARTESIAN_POINT('Ctrl Pts',(-0.110636551736313,0.16106121016526,
0.641786032157858));
#25726=CARTESIAN_POINT('Ctrl Pts',(-0.100594550532793,0.167959285651899,
0.641091049686774));
#25727=CARTESIAN_POINT('Ctrl Pts',(-0.0898830842274528,0.173929644787307,
0.64039606721569));
#25728=CARTESIAN_POINT('Ctrl Pts',(-0.0786979460104241,0.178851316164406,
0.639701084744605));
#25729=CARTESIAN_POINT('Ctrl Pts',(-0.0675143838270778,0.183772294057016,
0.639006200199515));
#25730=CARTESIAN_POINT('Ctrl Pts',(-0.0558580639667775,0.187644483188165,
0.638311315654425));
#25731=CARTESIAN_POINT('Ctrl Pts',(-0.04394768256483,0.190393700518638,
0.637616431109335));
#25732=CARTESIAN_POINT('Ctrl Pts',(-0.0320380091674312,0.193142754423751,
0.636921587871186));
#25733=CARTESIAN_POINT('Ctrl Pts',(-0.019875163546431,0.194768798139928,
0.636226744633037));
#25734=CARTESIAN_POINT('Ctrl Pts',(-0.00768842626097916,0.195248682714198,
0.635531901394887));
#25735=CARTESIAN_POINT('Ctrl Pts',(0.00452639839750962,0.195729673302058,
0.634835456717339));
#25736=CARTESIAN_POINT('Ctrl Pts',(0.0167643475810499,0.195059261525867,
0.634139012039792));
#25737=CARTESIAN_POINT('Ctrl Pts',(0.0287969878279878,0.193266379621585,
0.633442567362243));
#25738=CARTESIAN_POINT('Ctrl Pts',(0.0327241935979091,0.192681219921404,
0.633215262174025));
#25739=CARTESIAN_POINT('Ctrl Pts',(0.0366296043435642,0.191976899050893,
0.632987956985806));
#25740=CARTESIAN_POINT('Ctrl Pts',(0.0405055726968939,0.191155587364054,
0.632760651797587));
#25741=CARTESIAN_POINT('Ctrl Pts',(0.0523812170620796,0.188639156728729,
0.632064207623752));
#25742=CARTESIAN_POINT('Ctrl Pts',(0.0640634990743473,0.185002914352939,
0.631367763449917));
#25743=CARTESIAN_POINT('Ctrl Pts',(0.0753284366688527,0.180296385512929,
0.630671319276082));
#25744=CARTESIAN_POINT('Ctrl Pts',(0.0865697313198354,0.175599734774294,
0.629976336804997));
#25745=CARTESIAN_POINT('Ctrl Pts',(0.0973945914643227,0.169837521530361,
0.629281354333913));
#25746=CARTESIAN_POINT('Ctrl Pts',(0.107595203085472,0.163108651741702,
0.628586371862828));
#25747=CARTESIAN_POINT('Ctrl Pts',(0.117794377396932,0.1563807300795,0.627891487317738));
#25748=CARTESIAN_POINT('Ctrl Pts',(0.127368722555747,0.148686865242318,
0.627196602772649));
#25749=CARTESIAN_POINT('Ctrl Pts',(0.136137316504897,0.140170578420885,
0.626501718227559));
#25750=CARTESIAN_POINT('Ctrl Pts',(0.144905389210927,0.131654797844346,
0.62580687498941));
#25751=CARTESIAN_POINT('Ctrl Pts',(0.152867196198784,0.122317321672737,
0.62511203175126));
#25752=CARTESIAN_POINT('Ctrl Pts',(0.159878954651258,0.11233823863503,0.624417188513111));
#25753=CARTESIAN_POINT('Ctrl Pts',(0.16690687344843,0.102336156313655,0.623720743835563));
#25754=CARTESIAN_POINT('Ctrl Pts',(0.172979922348,0.0916902684111838,0.623024299158015));
#25755=CARTESIAN_POINT('Ctrl Pts',(0.177998536573932,0.0806081942332073,
0.622327854480467));
#25756=CARTESIAN_POINT('Ctrl Pts',(0.179636508817812,0.0769912336359282,
0.622100549292249));
#25757=CARTESIAN_POINT('Ctrl Pts',(0.181162542804326,0.0733279671628344,
0.62187324410403));
#25758=CARTESIAN_POINT('Ctrl Pts',(0.182574315093772,0.0696259970703467,
0.621645938915812));
#25759=CARTESIAN_POINT('Ctrl Pts',(0.186899867860399,0.0582834688912404,
0.620949494741977));
#25760=CARTESIAN_POINT('Ctrl Pts',(0.190179697863685,0.0464961584779568,
0.620253050568142));
#25761=CARTESIAN_POINT('Ctrl Pts',(0.192333956506123,0.0344791121507029,
0.619556606394306));
#25762=CARTESIAN_POINT('Ctrl Pts',(0.194483693772832,0.0224872872989626,
0.618861623923222));
#25763=CARTESIAN_POINT('Ctrl Pts',(0.195512322176856,0.0102675237078589,
0.618166641452139));
#25764=CARTESIAN_POINT('Ctrl Pts',(0.195390250357663,-0.00195193882324224,
0.617471658981055));
#25765=CARTESIAN_POINT('Ctrl Pts',(0.195268195738911,-0.0141696795799548,
0.616776774435965));
#25766=CARTESIAN_POINT('Ctrl Pts',(0.193995725410556,-0.0263862445888409,
0.616081889890875));
#25767=CARTESIAN_POINT('Ctrl Pts',(0.19159531661398,-0.0383717950008675,
0.615387005345786));
#25768=CARTESIAN_POINT('Ctrl Pts',(0.189195050508078,-0.050356632939979,
0.614692162107637));
#25769=CARTESIAN_POINT('Ctrl Pts',(0.185667177242148,-0.0621096300890771,
0.613997318869487));
#25770=CARTESIAN_POINT('Ctrl Pts',(0.181085037818701,-0.073412322386637,
0.613302475631338));
#25771=CARTESIAN_POINT('Ctrl Pts',(0.176492337713076,-0.0847410645552472,
0.612606030953791));
#25772=CARTESIAN_POINT('Ctrl Pts',(0.170840909584216,-0.0956166432650318,
0.611909586276243));
#25773=CARTESIAN_POINT('Ctrl Pts',(0.164251203983628,-0.105842817375241,
0.611213141598696));
#25774=CARTESIAN_POINT('Ctrl Pts',(0.162100459897061,-0.109180429831521,
0.610985836410476));
#25775=CARTESIAN_POINT('Ctrl Pts',(0.159850108273844,-0.112449102123599,
0.610758531222256));
#25776=CARTESIAN_POINT('Ctrl Pts',(0.157505276597089,-0.115642759583445,
0.610531226034036));
#25777=CARTESIAN_POINT('Ctrl Pts',(0.150320907543799,-0.125427860172448,
0.6098347818602));
#25778=CARTESIAN_POINT('Ctrl Pts',(0.142195762931484,-0.134575537290636,
0.609138337686365));
#25779=CARTESIAN_POINT('Ctrl Pts',(0.133267225082851,-0.142902087873889,
0.60844189351253));
#25780=CARTESIAN_POINT('Ctrl Pts',(0.124357426522772,-0.151211162624404,
0.607746911041446));
#25781=CARTESIAN_POINT('Ctrl Pts',(0.114648164614459,-0.158701885674412,
0.607051928570361));
#25782=CARTESIAN_POINT('Ctrl Pts',(0.104315160084808,-0.165225625665273,
0.606356946099277));
#25783=CARTESIAN_POINT('Ctrl Pts',(0.0939836115195674,-0.171748446433344,
0.605662061554187));
#25784=CARTESIAN_POINT('Ctrl Pts',(0.0830292095313433,-0.177304048869929,
0.604967177009097));
#25785=CARTESIAN_POINT('Ctrl Pts',(0.0716572538540142,-0.181786682598317,
0.604272292464007));
#25786=CARTESIAN_POINT('Ctrl Pts',(0.0602859741748835,-0.186269049859581,
0.603577449225858));
#25787=CARTESIAN_POINT('Ctrl Pts',(0.0484980146352318,-0.189678278754606,
0.602882605987709));
#25788=CARTESIAN_POINT('Ctrl Pts',(0.036516699986673,-0.191957522962981,
0.60218776274956));
#25789=CARTESIAN_POINT('Ctrl Pts',(0.0245077714127372,-0.194242020257626,
0.601491318072013));
#25790=CARTESIAN_POINT('Ctrl Pts',(0.0123054699786841,-0.195391233850034,
0.600794873394465));
#25791=CARTESIAN_POINT('Ctrl Pts',(0.000139995024282486,-0.195399949850027,
0.600098428716917));
#25792=CARTESIAN_POINT('Ctrl Pts',(-0.00383056525628826,-0.195402794572778,
0.599871123528698));
#25793=CARTESIAN_POINT('Ctrl Pts',(-0.007797216565637,-0.195284564411506,
0.599643818340479));
#25794=CARTESIAN_POINT('Ctrl Pts',(-0.0117520744557401,-0.195046273345549,
0.59941651315226));
#25795=CARTESIAN_POINT('Ctrl Pts',(-0.023869429794117,-0.194316169356887,
0.598720068978424));
#25796=CARTESIAN_POINT('Ctrl Pts',(-0.0359613798620174,-0.192449965942189,
0.598023624804589));
#25797=CARTESIAN_POINT('Ctrl Pts',(-0.047799078157251,-0.189463474388382,
0.597327180630754));
#25798=CARTESIAN_POINT('Ctrl Pts',(-0.0596119313940944,-0.186483250907572,
0.59663219815967));
#25799=CARTESIAN_POINT('Ctrl Pts',(-0.0711707331989876,-0.182387545907051,
0.595937215688586));
#25800=CARTESIAN_POINT('Ctrl Pts',(-0.0822553144165228,-0.177243401147233,
0.595242233217501));
#25801=CARTESIAN_POINT('Ctrl Pts',(-0.0933383337692836,-0.172099981219354,
0.594547348672412));
#25802=CARTESIAN_POINT('Ctrl Pts',(-0.103946452668831,-0.165908741055547,
0.593852464127323));
#25803=CARTESIAN_POINT('Ctrl Pts',(-0.113879490669761,-0.158784828005687,
0.593157579582233));
#25804=CARTESIAN_POINT('Ctrl Pts',(-0.123811938207988,-0.151661338432005,
0.592462736344084));
#25805=CARTESIAN_POINT('Ctrl Pts',(-0.133068688445595,-0.143605818162909,
0.591767893105934));
#25806=CARTESIAN_POINT('Ctrl Pts',(-0.141480875677578,-0.134775078621775,
0.591073049867785));
#25807=CARTESIAN_POINT('Ctrl Pts',(-0.149912450891368,-0.125923986440734,
0.590376605190237));
#25808=CARTESIAN_POINT('Ctrl Pts',(-0.15749502048588,-0.11629478655119,
0.58968016051269));
#25809=CARTESIAN_POINT('Ctrl Pts',(-0.164099372475197,-0.106078065372849,
0.588983715835142));
#25810=CARTESIAN_POINT('Ctrl Pts',(-0.166254896841161,-0.102743538158704,
0.588756410646923));
#25811=CARTESIAN_POINT('Ctrl Pts',(-0.168306574198394,-0.0993466394256172,
0.588529105458703));
#25812=CARTESIAN_POINT('Ctrl Pts',(-0.170250980957266,-0.095894543552221,
0.588301800270483));
#25813=CARTESIAN_POINT('Ctrl Pts',(-0.176472841648792,-0.0848482645161776,
0.587574451834201));
#25814=CARTESIAN_POINT('Ctrl Pts',(-0.181633608107616,-0.0731628494365437,
0.586847103397918));
#25815=CARTESIAN_POINT('Ctrl Pts',(-0.185615753856331,-0.0610569563632686,
0.586119754961635));
#25816=CARTESIAN_POINT('Ctrl Pts',(-0.189582653754339,-0.0489974113269807,
0.585395191216413));
#25817=CARTESIAN_POINT('Ctrl Pts',(-0.192379592139015,-0.0365212802349419,
0.584670627471192));
#25818=CARTESIAN_POINT('Ctrl Pts',(-0.193936890827428,-0.0238671819909773,
0.58394606372597));
#25819=CARTESIAN_POINT('Ctrl Pts',(-0.194910587582813,-0.0159552415943475,
0.583493032221454));
#25820=CARTESIAN_POINT('Ctrl Pts',(-0.195400620193043,-0.00797414202748591,
0.583040000716939));
#25821=CARTESIAN_POINT('Ctrl Pts',(-0.195399999410133,1.51828823620237E-5,
0.582586969212423));
#25822=CARTESIAN_POINT('',(-0.195488415809582,0.000168817958016994,0.512586969212423));
#25823=CARTESIAN_POINT('Ctrl Pts',(-0.195080329228051,1.5371999046063E-5,
0.582586957060278));
#25824=CARTESIAN_POINT('Ctrl Pts',(-0.195102226640896,0.0317061316006451,
0.580787000503088));
#25825=CARTESIAN_POINT('Ctrl Pts',(-0.172828823719728,0.128597837672465,
0.57528213965197));
#25826=CARTESIAN_POINT('Ctrl Pts',(-0.0204016541079559,0.230056252374797,
0.566072374506932));
#25827=CARTESIAN_POINT('Ctrl Pts',(0.182230257970378,0.141895171965532,
0.554957661625154));
#25828=CARTESIAN_POINT('Ctrl Pts',(0.218039356482699,-0.0761639401008706,
0.543842948743379));
#25829=CARTESIAN_POINT('Ctrl Pts',(0.0542441778475854,-0.224498721414439,
0.532728235861602));
#25830=CARTESIAN_POINT('Ctrl Pts',(-0.145841485605917,-0.170897033639993,
0.52230957601795));
#25831=CARTESIAN_POINT('Ctrl Pts',(-0.195008257896402,-0.052526494143854,
0.515595820468224));
#25832=CARTESIAN_POINT('Ctrl Pts',(-0.195488415809582,0.000168817958016994,
0.512586969212423));
#25833=CARTESIAN_POINT('',(-0.195399963336573,-0.000119699900101725,0.442586969212423));
#25834=CARTESIAN_POINT('Ctrl Pts',(-0.195488415809582,0.000168817958016994,
0.512586969212423));
#25835=CARTESIAN_POINT('Ctrl Pts',(-0.195599493209505,0.0123590955640317,
0.511890916174299));
#25836=CARTESIAN_POINT('Ctrl Pts',(-0.189008463564054,0.0893152196074113,
0.507489958842245));
#25837=CARTESIAN_POINT('Ctrl Pts',(-0.086890608201959,0.213990955307397,
0.499384097216276));
#25838=CARTESIAN_POINT('Ctrl Pts',(0.132676899813103,0.189047472881976,
0.488269384334496));
#25839=CARTESIAN_POINT('Ctrl Pts',(0.230785249680916,-0.00895964713562786,
0.477154671452722));
#25840=CARTESIAN_POINT('Ctrl Pts',(0.117621085806451,-0.198764652090832,
0.466039958570945));
#25841=CARTESIAN_POINT('Ctrl Pts',(-0.103219381045709,-0.206610421139929,
0.454925245689168));
#25842=CARTESIAN_POINT('Ctrl Pts',(-0.192087873248582,-0.079093845467276,
0.447107582569661));
#25843=CARTESIAN_POINT('Ctrl Pts',(-0.195677774776043,-0.00724967654898506,
0.44299482374408));
#25844=CARTESIAN_POINT('Ctrl Pts',(-0.195626364086859,-0.000119838590748017,
0.442586969212423));
#25845=CARTESIAN_POINT('',(-0.195390096198874,-9.39320554627862E-5,0.372586973725733));
#25846=CARTESIAN_POINT('Ctrl Pts',(-0.195399963336573,-0.000119699900101725,
0.442586969212423));
#25847=CARTESIAN_POINT('Ctrl Pts',(-0.195407310566176,0.0118740310377059,
0.441900082807232));
#25848=CARTESIAN_POINT('Ctrl Pts',(-0.194306083298946,0.0239118037275281,
0.441213196402041));
#25849=CARTESIAN_POINT('Ctrl Pts',(-0.192098246916485,0.0357690303420858,
0.44052630999685));
#25850=CARTESIAN_POINT('Ctrl Pts',(-0.189892534040976,0.0476148526228203,
0.439840084242089));
#25851=CARTESIAN_POINT('Ctrl Pts',(-0.186582402621779,0.0592795776638148,
0.439153858487328));
#25852=CARTESIAN_POINT('Ctrl Pts',(-0.182221619809175,0.0705438960798197,
0.438467632732567));
#25853=CARTESIAN_POINT('Ctrl Pts',(-0.177863933633089,0.0818002155880018,
0.437781894273739));
#25854=CARTESIAN_POINT('Ctrl Pts',(-0.172457395824743,0.0926558495972733,
0.437096155814912));
#25855=CARTESIAN_POINT('Ctrl Pts',(-0.166104625509635,0.102909734157193,
0.436410417356085));
#25856=CARTESIAN_POINT('Ctrl Pts',(-0.159737017950417,0.113187567227877,
0.435723077317411));
#25857=CARTESIAN_POINT('Ctrl Pts',(-0.152419265438923,0.122860088840632,
0.435035737278736));
#25858=CARTESIAN_POINT('Ctrl Pts',(-0.144297762712538,0.131754755800904,
0.434348397240062));
#25859=CARTESIAN_POINT('Ctrl Pts',(-0.13778889742042,0.138883262804243,
0.433797538135247));
#25860=CARTESIAN_POINT('Ctrl Pts',(-0.130764771052242,0.145512637421945,
0.433246679030432));
#25861=CARTESIAN_POINT('Ctrl Pts',(-0.123316693953183,0.151572269866414,
0.432695819925617));
#25862=CARTESIAN_POINT('Ctrl Pts',(-0.113900184619716,0.159233386247437,
0.431999375751781));
#25863=CARTESIAN_POINT('Ctrl Pts',(-0.103733686146086,0.166040755813973,
0.431302931577945));
#25864=CARTESIAN_POINT('Ctrl Pts',(-0.0929964058226484,0.171851181270509,
0.43060648740411));
#25865=CARTESIAN_POINT('Ctrl Pts',(-0.0822816609913256,0.177649411758383,
0.429911504933026));
#25866=CARTESIAN_POINT('Ctrl Pts',(-0.0709992389971638,0.182454373002956,
0.429216522461941));
#25867=CARTESIAN_POINT('Ctrl Pts',(-0.0593566206831002,0.186166462020103,
0.428521539990857));
#25868=CARTESIAN_POINT('Ctrl Pts',(-0.0477156428636164,0.189878027988075,
0.427826655445767));
#25869=CARTESIAN_POINT('Ctrl Pts',(-0.0357153885134297,0.192496717905539,
0.427131770900677));
#25870=CARTESIAN_POINT('Ctrl Pts',(-0.0235811686724703,0.193971875497559,
0.426436886355588));
#25871=CARTESIAN_POINT('Ctrl Pts',(-0.0114476701419841,0.195446945399835,
0.425742043117439));
#25872=CARTESIAN_POINT('Ctrl Pts',(0.000818905484256999,0.195778538784712,
0.425047199879289));
#25873=CARTESIAN_POINT('Ctrl Pts',(0.0129881151909117,0.194967866233868,
0.42435235664114));
#25874=CARTESIAN_POINT('Ctrl Pts',(0.0251853718739311,0.19415532528611,
0.423655911963592));
#25875=CARTESIAN_POINT('Ctrl Pts',(0.0372839457004307,0.192195385610171,
0.422959467286044));
#25876=CARTESIAN_POINT('Ctrl Pts',(0.049059739844796,0.18914095782342,0.422263022608497));
#25877=CARTESIAN_POINT('Ctrl Pts',(0.0529031163407337,0.188144055549127,
0.422035717420278));
#25878=CARTESIAN_POINT('Ctrl Pts',(0.0567122271421686,0.187030962613515,
0.421808412232059));
#25879=CARTESIAN_POINT('Ctrl Pts',(0.060479697061881,0.185804645376005,
0.42158110704384));
#25880=CARTESIAN_POINT('Ctrl Pts',(0.0720229112588168,0.182047311449621,
0.420884662870005));
#25881=CARTESIAN_POINT('Ctrl Pts',(0.0832555063943229,0.177196870423139,
0.42018821869617));
#25882=CARTESIAN_POINT('Ctrl Pts',(0.0939599883447792,0.171326240226793,
0.419491774522335));
#25883=CARTESIAN_POINT('Ctrl Pts',(0.104642003640618,0.165467931357311,
0.418796792051251));
#25884=CARTESIAN_POINT('Ctrl Pts',(0.114797309786046,0.158594034667023,
0.418101809580167));
#25885=CARTESIAN_POINT('Ctrl Pts',(0.124229708622614,0.150824863651655,
0.417406827109083));
#25886=CARTESIAN_POINT('Ctrl Pts',(0.133660778393953,0.143056787345623,
0.416711942563993));
#25887=CARTESIAN_POINT('Ctrl Pts',(0.1423684388659,0.134394207449415,0.416017058018904));
#25888=CARTESIAN_POINT('Ctrl Pts',(0.150187948103768,0.124998960973201,
0.415322173473814));
#25889=CARTESIAN_POINT('Ctrl Pts',(0.158006992516213,0.115604272991042,
0.414627330235665));
#25890=CARTESIAN_POINT('Ctrl Pts',(0.164937450830462,0.105477695122798,
0.413932486997516));
#25891=CARTESIAN_POINT('Ctrl Pts',(0.170855376770996,0.0948135023529931,
0.413237643759367));
#25892=CARTESIAN_POINT('Ctrl Pts',(0.176786942046618,0.0841247312934131,
0.412541199081819));
#25893=CARTESIAN_POINT('Ctrl Pts',(0.181700948228195,0.0728966684410854,
0.411844754404271));
#25894=CARTESIAN_POINT('Ctrl Pts',(0.185520328854313,0.0613462923230709,
0.411148309726724));
#25895=CARTESIAN_POINT('Ctrl Pts',(0.186766895968817,0.0575764876247876,
0.410921004538504));
#25896=CARTESIAN_POINT('Ctrl Pts',(0.187897258122969,0.0537724657555652,
0.410693699350284));
#25897=CARTESIAN_POINT('Ctrl Pts',(0.188909908278612,0.0499420319387021,
0.410466394162065));
#25898=CARTESIAN_POINT('Ctrl Pts',(0.192012584053656,0.0382059016026106,
0.409769949988229));
#25899=CARTESIAN_POINT('Ctrl Pts',(0.194028388996668,0.0261379895188498,
0.409073505814394));
#25900=CARTESIAN_POINT('Ctrl Pts',(0.194900647294117,0.0139605760745879,
0.408377061640559));
#25901=CARTESIAN_POINT('Ctrl Pts',(0.195771074888688,0.00180872068565739,
0.407682079169474));
#25902=CARTESIAN_POINT('Ctrl Pts',(0.195502583269476,-0.0104513205404809,
0.40698709669839));
#25903=CARTESIAN_POINT('Ctrl Pts',(0.194089866700077,-0.0225894586997189,
0.406292114227305));
#25904=CARTESIAN_POINT('Ctrl Pts',(0.192677349188469,-0.0347258865435164,
0.405597229682215));
#25905=CARTESIAN_POINT('Ctrl Pts',(0.190120982082382,-0.0467395715973172,
0.404902345137126));
#25906=CARTESIAN_POINT('Ctrl Pts',(0.186467405668497,-0.058404337366844,
0.404207460592036));
#25907=CARTESIAN_POINT('Ctrl Pts',(0.182814046438984,-0.0700684097322835,
0.403512617353886));
#25908=CARTESIAN_POINT('Ctrl Pts',(0.17806389466511,-0.0813827762586296,
0.402817774115737));
#25909=CARTESIAN_POINT('Ctrl Pts',(0.172312967513375,-0.0921379467251932,
0.402122930877587));
#25910=CARTESIAN_POINT('Ctrl Pts',(0.166548785916879,-0.102917905162302,
0.401426486200039));
#25911=CARTESIAN_POINT('Ctrl Pts',(0.159779694153344,-0.113135353418367,
0.400730041522491));
#25912=CARTESIAN_POINT('Ctrl Pts',(0.152146206670055,-0.122607878196765,
0.400033596844944));
#25913=CARTESIAN_POINT('Ctrl Pts',(0.149654793690548,-0.125699515044703,
0.399806291656725));
#25914=CARTESIAN_POINT('Ctrl Pts',(0.147071616394809,-0.128712071440798,
0.399578986468507));
#25915=CARTESIAN_POINT('Ctrl Pts',(0.144402415512848,-0.131640048594851,
0.399351681280288));
#25916=CARTESIAN_POINT('Ctrl Pts',(0.136224206218077,-0.14061112684452,
0.398655237106453));
#25917=CARTESIAN_POINT('Ctrl Pts',(0.12717785096287,-0.148848931662931,
0.397958792932618));
#25918=CARTESIAN_POINT('Ctrl Pts',(0.117419376155819,-0.156185306937555,
0.397262348758782));
#25919=CARTESIAN_POINT('Ctrl Pts',(0.107681382515825,-0.16350628456751,
0.396567366287698));
#25920=CARTESIAN_POINT('Ctrl Pts',(0.0972348839673393,-0.169929007252841,
0.395872383816614));
#25921=CARTESIAN_POINT('Ctrl Pts',(0.0862703243360016,-0.175324245724774,
0.395177401345529));
#25922=CARTESIAN_POINT('Ctrl Pts',(0.0753073096578856,-0.180718723984593,
0.394482516800439));
#25923=CARTESIAN_POINT('Ctrl Pts',(0.0638271429792277,-0.185085578044804,
0.39378763225535));
#25924=CARTESIAN_POINT('Ctrl Pts',(0.0520451499259236,-0.188341345352496,
0.39309274771026));
#25925=CARTESIAN_POINT('Ctrl Pts',(0.0402638572452036,-0.191596919123309,
0.392397904472111));
#25926=CARTESIAN_POINT('Ctrl Pts',(0.0281816250544544,-0.19374132977803,
0.391703061233961));
#25927=CARTESIAN_POINT('Ctrl Pts',(0.0160265349818396,-0.194741649824776,
0.391008217995812));
#25928=CARTESIAN_POINT('Ctrl Pts',(0.00384343047508048,-0.195744275358352,
0.390311773318264));
#25929=CARTESIAN_POINT('Ctrl Pts',(-0.00841198957600976,-0.195597539064805,
0.389615328640716));
#25930=CARTESIAN_POINT('Ctrl Pts',(-0.0205102638617534,-0.194320583254377,
0.388918883963168));
#25931=CARTESIAN_POINT('Ctrl Pts',(-0.0244588912291522,-0.193903811197394,
0.388691578774949));
#25932=CARTESIAN_POINT('Ctrl Pts',(-0.0283908365629753,-0.193367055319197,
0.38846427358673));
#25933=CARTESIAN_POINT('Ctrl Pts',(-0.0322983667202349,-0.192712157133911,
0.388236968398512));
#25934=CARTESIAN_POINT('Ctrl Pts',(-0.044270713825152,-0.190705603613638,
0.387540524224677));
#25935=CARTESIAN_POINT('Ctrl Pts',(-0.0560977372091341,-0.187571997144415,
0.386844080050843));
#25936=CARTESIAN_POINT('Ctrl Pts',(-0.0675535427233033,-0.183351244515904,
0.386147635877009));
#25937=CARTESIAN_POINT('Ctrl Pts',(-0.078985304698777,-0.179139350437673,
0.385452653405926));
#25938=CARTESIAN_POINT('Ctrl Pts',(-0.0900465559772294,-0.173845068732815,
0.384757670934844));
#25939=CARTESIAN_POINT('Ctrl Pts',(-0.100525445100651,-0.167558332789856,
0.384062688463761));
#25940=CARTESIAN_POINT('Ctrl Pts',(-0.111002857703909,-0.1612724826748,
0.383367803918672));
#25941=CARTESIAN_POINT('Ctrl Pts',(-0.120897297563241,-0.153994866222789,
0.382672919373584));
#25942=CARTESIAN_POINT('Ctrl Pts',(-0.130021873704177,-0.14586114067309,
0.381978034828495));
#25943=CARTESIAN_POINT('Ctrl Pts',(-0.13914590744087,-0.137727898627193,
0.381283191590347));
#25944=CARTESIAN_POINT('Ctrl Pts',(-0.147499532374186,-0.128739251218365,
0.380588348352199));
#25945=CARTESIAN_POINT('Ctrl Pts',(-0.154931399895884,-0.119068977178364,
0.379893505114051));
#25946=CARTESIAN_POINT('Ctrl Pts',(-0.162380396008324,-0.109376415581983,
0.379197060436504));
#25947=CARTESIAN_POINT('Ctrl Pts',(-0.168902911728162,-0.0989998245785479,
0.378500615758957));
#25948=CARTESIAN_POINT('Ctrl Pts',(-0.174390599395294,-0.0881423782442364,
0.377804171081411));
#25949=CARTESIAN_POINT('Ctrl Pts',(-0.176181667542286,-0.0845987315451845,
0.377576865893186));
#25950=CARTESIAN_POINT('Ctrl Pts',(-0.177862878884868,-0.0810040369262574,
0.377349560704961));
#25951=CARTESIAN_POINT('Ctrl Pts',(-0.179431587178082,-0.0773657903905484,
0.377122255516736));
#25952=CARTESIAN_POINT('Ctrl Pts',(-0.184725790511809,-0.0650871423961478,
0.376355127625286));
#25953=CARTESIAN_POINT('Ctrl Pts',(-0.188767040765519,-0.0522371217977153,
0.375587999733836));
#25954=CARTESIAN_POINT('Ctrl Pts',(-0.191453853265823,-0.0390714994550838,
0.374820871842387));
#25955=CARTESIAN_POINT('Ctrl Pts',(-0.194061877734694,-0.0262919455362255,
0.374076239192573));
#25956=CARTESIAN_POINT('Ctrl Pts',(-0.195393669118938,-0.0132155597336468,
0.373331606542758));
#25957=CARTESIAN_POINT('Ctrl Pts',(-0.195399977418944,-9.39397482887344E-5,
0.372586973892944));
#25958=CARTESIAN_POINT('',(-0.19539992650912,0.000169470441615271,0.302586967349177));
#25959=CARTESIAN_POINT('Ctrl Pts',(-0.195123386395527,-9.37244138880245E-5,
0.372586969212423));
#25960=CARTESIAN_POINT('Ctrl Pts',(-0.19495607068899,0.0384983387935844,
0.370393827019935));
#25961=CARTESIAN_POINT('Ctrl Pts',(-0.165199853610515,0.142522406630586,
0.364495780533521));
#25962=CARTESIAN_POINT('Ctrl Pts',(0.00402447047846805,0.230924035961026,
0.354892829753184));
#25963=CARTESIAN_POINT('Ctrl Pts',(0.196205039257053,0.121842887839667,
0.343778116871407));
#25964=CARTESIAN_POINT('Ctrl Pts',(0.208769571438819,-0.0987794148000683,
0.332663403989631));
#25965=CARTESIAN_POINT('Ctrl Pts',(0.0302158574941567,-0.22897403499859,
0.321548691107855));
#25966=CARTESIAN_POINT('Ctrl Pts',(-0.155790063617848,-0.157337309383673,
0.311523212848785));
#25967=CARTESIAN_POINT('Ctrl Pts',(-0.194903398518234,-0.0457626416864486,
0.305202638883641));
#25968=CARTESIAN_POINT('Ctrl Pts',(-0.195283952697599,0.000169337138534779,
0.302586969212423));
#25969=CARTESIAN_POINT('',(-0.195399999941521,-4.78056065513374E-6,0.232586969207602));
#25970=CARTESIAN_POINT('Ctrl Pts',(-0.19539992650912,0.000169470441615271,
0.302586967349177));
#25971=CARTESIAN_POINT('Ctrl Pts',(-0.195386996090356,0.0150782819843667,
0.301738458498935));
#25972=CARTESIAN_POINT('Ctrl Pts',(-0.19366378775983,0.0299110432009344,
0.300889949648692));
#25973=CARTESIAN_POINT('Ctrl Pts',(-0.190305156722521,0.0443295310692184,
0.30004144079845));
#25974=CARTESIAN_POINT('Ctrl Pts',(-0.189352300468089,0.0484201102939455,
0.299800715647067));
#25975=CARTESIAN_POINT('Ctrl Pts',(-0.188268106887131,0.0524774798667048,
0.299559990495685));
#25976=CARTESIAN_POINT('Ctrl Pts',(-0.187054971073491,0.0564942279945073,
0.299319265344302));
#25977=CARTESIAN_POINT('Ctrl Pts',(-0.183545236571318,0.0681151193507628,
0.298622821170576));
#25978=CARTESIAN_POINT('Ctrl Pts',(-0.178936005112572,0.0794488282295186,
0.29792637699685));
#25979=CARTESIAN_POINT('Ctrl Pts',(-0.173295528940874,0.0902763515495762,
0.297229932823124));
#25980=CARTESIAN_POINT('Ctrl Pts',(-0.167666891046876,0.101081149974792,
0.296534950352147));
#25981=CARTESIAN_POINT('Ctrl Pts',(-0.161011638749481,0.111381068199425,
0.295839967881171));
#25982=CARTESIAN_POINT('Ctrl Pts',(-0.153445864238863,0.120977381142049,
0.295144985410195));
#25983=CARTESIAN_POINT('Ctrl Pts',(-0.145881155778107,0.130572341923294,
0.29445010086521));
#25984=CARTESIAN_POINT('Ctrl Pts',(-0.137406684932671,0.13946317907191,
0.293755216320225));
#25985=CARTESIAN_POINT('Ctrl Pts',(-0.128180730309582,0.147481728960919,
0.29306033177524));
#25986=CARTESIAN_POINT('Ctrl Pts',(-0.118955324117087,0.155499802192688,
0.292365488537193));
#25987=CARTESIAN_POINT('Ctrl Pts',(-0.108979201367998,0.162645136797938,
0.291670645299147));
#25988=CARTESIAN_POINT('Ctrl Pts',(-0.0984439432562392,0.168789662112827,
0.290975802061101));
#25989=CARTESIAN_POINT('Ctrl Pts',(-0.0878844040166807,0.174948349017575,
0.290279357383651));
#25990=CARTESIAN_POINT('Ctrl Pts',(-0.0767639454581824,0.180101236904367,
0.289582912706202));
#25991=CARTESIAN_POINT('Ctrl Pts',(-0.0652978492051816,0.184166638914808,
0.288886468028752));
#25992=CARTESIAN_POINT('Ctrl Pts',(-0.0615555517086098,0.185493502341605,
0.288659162840011));
#25993=CARTESIAN_POINT('Ctrl Pts',(-0.0577765609300914,0.186704918764145,
0.288431857651269));
#25994=CARTESIAN_POINT('Ctrl Pts',(-0.0539686480960809,0.187799214648734,
0.288204552462527));
#25995=CARTESIAN_POINT('Ctrl Pts',(-0.042301520206118,0.191152046131886,
0.287508108288854));
#25996=CARTESIAN_POINT('Ctrl Pts',(-0.0302794540633588,0.193425347083275,
0.28681166411518));
#25997=CARTESIAN_POINT('Ctrl Pts',(-0.018123467799382,0.194557703303993,
0.286115219941507));
#25998=CARTESIAN_POINT('Ctrl Pts',(-0.00599299461925058,0.195687682926172,
0.285420237470587));
#25999=CARTESIAN_POINT('Ctrl Pts',(0.00626998454611778,0.19568131607234,
0.284725254999667));
#26000=CARTESIAN_POINT('Ctrl Pts',(0.0184355467757656,0.194528379973408,
0.284030272528747));
#26001=CARTESIAN_POINT('Ctrl Pts',(0.0305993948257797,0.193375606328092,
0.283335387983823));
#26002=CARTESIAN_POINT('Ctrl Pts',(0.0426649783854545,0.1910766207582,0.2826405034389));
#26003=CARTESIAN_POINT('Ctrl Pts',(0.05440517568215,0.18767321827846,0.281945618893976));
#26004=CARTESIAN_POINT('Ctrl Pts',(0.0661446750907626,0.184270018111676,
0.281250775655993));
#26005=CARTESIAN_POINT('Ctrl Pts',(0.0775579929528,0.179762800890329,0.280555932418011));
#26006=CARTESIAN_POINT('Ctrl Pts',(0.0884336345056216,0.174243083903282,
0.279861089180029));
#26007=CARTESIAN_POINT('Ctrl Pts',(0.099334341684665,0.168710645352898,
0.279164644502646));
#26008=CARTESIAN_POINT('Ctrl Pts',(0.109694147573257,0.162161502351643,
0.278468199825263));
#26009=CARTESIAN_POINT('Ctrl Pts',(0.119327676998619,0.154732238082803,
0.277771755147881));
#26010=CARTESIAN_POINT('Ctrl Pts',(0.122471862456992,0.152307479341837,
0.277544449958837));
#26011=CARTESIAN_POINT('Ctrl Pts',(0.125538947031261,0.149789286873123,
0.277317144769794));
#26012=CARTESIAN_POINT('Ctrl Pts',(0.128523310477063,0.147183282556194,
0.27708983958075));
#26013=CARTESIAN_POINT('Ctrl Pts',(0.137667151606952,0.139198702296266,
0.276393395406186));
#26014=CARTESIAN_POINT('Ctrl Pts',(0.146096443818796,0.130330500407694,
0.275696951231621));
#26015=CARTESIAN_POINT('Ctrl Pts',(0.15363973429167,0.120731073244567,0.275000507057057));
#26016=CARTESIAN_POINT('Ctrl Pts',(0.161167192844588,0.111151793437958,
0.274305524585242));
#26017=CARTESIAN_POINT('Ctrl Pts',(0.167811746267886,0.100844970032632,
0.273610542113427));
#26018=CARTESIAN_POINT('Ctrl Pts',(0.173440124003984,0.0899982410132693,
0.272915559641613));
#26019=CARTESIAN_POINT('Ctrl Pts',(0.179067708677579,0.0791530403444332,
0.272220675095802));
#26020=CARTESIAN_POINT('Ctrl Pts',(0.18367895827777,0.067768839943914,0.271525790549991));
#26021=CARTESIAN_POINT('Ctrl Pts',(0.187185826647367,0.0560591321939784,
0.27083090600418));
#26022=CARTESIAN_POINT('Ctrl Pts',(0.190692486553528,0.0443501205197569,
0.270136062765314));
#26023=CARTESIAN_POINT('Ctrl Pts',(0.19309466992589,0.0323164865258053,
0.269441219526448));
#26024=CARTESIAN_POINT('Ctrl Pts',(0.194354581457236,0.0201855558898628,
0.268746376287582));
#26025=CARTESIAN_POINT('Ctrl Pts',(0.195617396768639,0.00802666650159185,
0.268049931609338));
#26026=CARTESIAN_POINT('Ctrl Pts',(0.19573265863162,-0.00422908998952003,
0.267353486931093));
#26027=CARTESIAN_POINT('Ctrl Pts',(0.194714600152907,-0.0163518955260133,
0.266657042252849));
#26028=CARTESIAN_POINT('Ctrl Pts',(0.194382326854407,-0.0203085293215227,
0.266429737068224));
#26029=CARTESIAN_POINT('Ctrl Pts',(0.193929740567102,-0.0242510495988667,
0.266202431883599));
#26030=CARTESIAN_POINT('Ctrl Pts',(0.193358517085165,-0.0281716856191818,
0.265975126698974));
#26031=CARTESIAN_POINT('Ctrl Pts',(0.191608335864775,-0.0401841881715449,
0.265278682526058));
#26032=CARTESIAN_POINT('Ctrl Pts',(0.188728252853097,-0.0520754914273812,
0.264582238353142));
#26033=CARTESIAN_POINT('Ctrl Pts',(0.184753337141331,-0.0636188998265577,
0.263885794180226));
#26034=CARTESIAN_POINT('Ctrl Pts',(0.180786764015271,-0.0751380808254853,
0.263190811710053));
#26035=CARTESIAN_POINT('Ctrl Pts',(0.175730130750634,-0.0863099722633644,
0.262495829239881));
#26036=CARTESIAN_POINT('Ctrl Pts',(0.1696688217757,-0.0969208487233055,
0.261800846769709));
#26037=CARTESIAN_POINT('Ctrl Pts',(0.163608366864844,-0.107530230065861,
0.261105962225507));
#26038=CARTESIAN_POINT('Ctrl Pts',(0.156543910936009,-0.117577971276881,
0.260411077681305));
#26039=CARTESIAN_POINT('Ctrl Pts',(0.148607085361824,-0.126874324353919,
0.259716193137103));
#26040=CARTESIAN_POINT('Ctrl Pts',(0.140670731586706,-0.136170124815726,
0.259021349899829));
#26041=CARTESIAN_POINT('Ctrl Pts',(0.131862700088761,-0.144713977140462,
0.258326506662554));
#26042=CARTESIAN_POINT('Ctrl Pts',(0.12235349475577,-0.15235085270864,0.25763166342528));
#26043=CARTESIAN_POINT('Ctrl Pts',(0.11282237308887,-0.160005329360096,
0.256935218748572));
#26044=CARTESIAN_POINT('Ctrl Pts',(0.102587574404305,-0.166748158713353,
0.256238774071864));
#26045=CARTESIAN_POINT('Ctrl Pts',(0.0918499103809251,-0.172466674934655,
0.255542329395156));
#26046=CARTESIAN_POINT('Ctrl Pts',(0.0883453580868168,-0.174333080802694,
0.255315024202503));
#26047=CARTESIAN_POINT('Ctrl Pts',(0.0847874212998323,-0.176090746132482,
0.255087719009851));
#26048=CARTESIAN_POINT('Ctrl Pts',(0.081183537746253,-0.177736865053378,
0.254860413817198));
#26049=CARTESIAN_POINT('Ctrl Pts',(0.070141538783967,-0.182780436285939,
0.254163969644105));
#26050=CARTESIAN_POINT('Ctrl Pts',(0.0585886545158649,-0.186808939278657,
0.253467525471012));
#26051=CARTESIAN_POINT('Ctrl Pts',(0.0467343719214419,-0.189728907868855,
0.252771081297919));
#26052=CARTESIAN_POINT('Ctrl Pts',(0.0349049691930304,-0.192642748004909,
0.252076098827597));
#26053=CARTESIAN_POINT('Ctrl Pts',(0.0227762476073445,-0.194452391887296,
0.251381116357274));
#26054=CARTESIAN_POINT('Ctrl Pts',(0.0105740813452859,-0.195113681744011,
0.250686133886952));
#26055=CARTESIAN_POINT('Ctrl Pts',(-0.0016263655792097,-0.195774878422149,
0.249991249342641));
#26056=CARTESIAN_POINT('Ctrl Pts',(-0.0138993660566686,-0.195287948947145,
0.249296364798329));
#26057=CARTESIAN_POINT('Ctrl Pts',(-0.0260141132144387,-0.193660594633153,
0.248601480254018));
#26058=CARTESIAN_POINT('Ctrl Pts',(-0.0381281402190967,-0.192033337056159,
0.247906637016657));
#26059=CARTESIAN_POINT('Ctrl Pts',(-0.0500830681767129,-0.189265932318957,
0.247211793779297));
#26060=CARTESIAN_POINT('Ctrl Pts',(-0.0616561819046621,-0.18541756991434,
0.246516950541937));
#26061=CARTESIAN_POINT('Ctrl Pts',(-0.0732559687572675,-0.181560337999533,
0.245820505865178));
#26062=CARTESIAN_POINT('Ctrl Pts',(-0.0844713745976783,-0.176617512523793,
0.245124061188419));
#26063=CARTESIAN_POINT('Ctrl Pts',(-0.0950988423629525,-0.170696719890062,
0.24442761651166));
#26064=CARTESIAN_POINT('Ctrl Pts',(-0.0985674288599389,-0.168764295173807,
0.244200311319581));
#26065=CARTESIAN_POINT('Ctrl Pts',(-0.101973600475422,-0.166728049500301,
0.243973006127501));
#26066=CARTESIAN_POINT('Ctrl Pts',(-0.105310966422842,-0.164592710504102,
0.243745700935422));
#26067=CARTESIAN_POINT('Ctrl Pts',(-0.115543810534397,-0.158045453949777,
0.243048750516156));
#26068=CARTESIAN_POINT('Ctrl Pts',(-0.125199707284002,-0.15051727213275,
0.242351800096891));
#26069=CARTESIAN_POINT('Ctrl Pts',(-0.134086365345269,-0.142133763154625,
0.241654849677626));
#26070=CARTESIAN_POINT('Ctrl Pts',(-0.142954369225497,-0.133767852186139,
0.240959362242444));
#26071=CARTESIAN_POINT('Ctrl Pts',(-0.151055658945902,-0.124550717705166,
0.240263874807263));
#26072=CARTESIAN_POINT('Ctrl Pts',(-0.158230506826314,-0.114648448351854,
0.239568387372081));
#26073=CARTESIAN_POINT('Ctrl Pts',(-0.165404331796768,-0.104747590753899,
0.238872999091757));
#26074=CARTESIAN_POINT('Ctrl Pts',(-0.17165142749491,-0.0941624718976632,
0.238177610811433));
#26075=CARTESIAN_POINT('Ctrl Pts',(-0.176852967045611,-0.0830914438866242,
0.237482222531109));
#26076=CARTESIAN_POINT('Ctrl Pts',(-0.182054153530154,-0.072021167346431,
0.236786881451824));
#26077=CARTESIAN_POINT('Ctrl Pts',(-0.18620957656066,-0.0604658495818994,
0.236091540372539));
#26078=CARTESIAN_POINT('Ctrl Pts',(-0.18924805461596,-0.0486449773776757,
0.235396199293253));
#26079=CARTESIAN_POINT('Ctrl Pts',(-0.192293556288096,-0.0367967805472705,
0.234699250893059));
#26080=CARTESIAN_POINT('Ctrl Pts',(-0.194216802258729,-0.0246826660200671,
0.234002302492864));
#26081=CARTESIAN_POINT('Ctrl Pts',(-0.194997693637588,-0.0125323372130376,
0.233305354092669));
#26082=CARTESIAN_POINT('Ctrl Pts',(-0.195265996886212,-0.00835765584372756,
0.233065892465921));
#26083=CARTESIAN_POINT('Ctrl Pts',(-0.195399897822299,-0.00417871467006272,
0.232826430839172));
#26084=CARTESIAN_POINT('Ctrl Pts',(-0.195399999941518,-4.78064468390912E-6,
0.232586969212423));
#26085=CARTESIAN_POINT('',(-0.19539992906386,-0.00016649876455978,0.162586971253333));
#26086=CARTESIAN_POINT('Ctrl Pts',(-0.195399999941521,-4.78056065513374E-6,
0.232586969207602));
#26087=CARTESIAN_POINT('Ctrl Pts',(-0.19540029672657,0.0121259720518583,
0.231891019119132));
#26088=CARTESIAN_POINT('Ctrl Pts',(-0.194266622200123,0.0242999913662591,
0.231195069030662));
#26089=CARTESIAN_POINT('Ctrl Pts',(-0.192000856353013,0.0362881683157171,
0.230499118942192));
#26090=CARTESIAN_POINT('Ctrl Pts',(-0.189739844128247,0.0482511938286821,
0.229804628971012));
#26091=CARTESIAN_POINT('Ctrl Pts',(-0.186351542393054,0.0600282837654985,
0.229110138999833));
#26092=CARTESIAN_POINT('Ctrl Pts',(-0.181889493436239,0.0713958834773282,
0.228415649028654));
#26093=CARTESIAN_POINT('Ctrl Pts',(-0.177428065158018,0.0827619019367191,
0.22772125566221));
#26094=CARTESIAN_POINT('Ctrl Pts',(-0.171893463435113,0.0937177112672988,
0.227026862295766));
#26095=CARTESIAN_POINT('Ctrl Pts',(-0.165388451631415,0.104056811727839,
0.226332468929322));
#26096=CARTESIAN_POINT('Ctrl Pts',(-0.158883771142894,0.114395385594271,
0.225638110929926));
#26097=CARTESIAN_POINT('Ctrl Pts',(-0.151409268985664,0.124116585139044,
0.224943752930529));
#26098=CARTESIAN_POINT('Ctrl Pts',(-0.143111171736177,0.133042671817348,
0.224249394931133));
#26099=CARTESIAN_POINT('Ctrl Pts',(-0.134794009745904,0.141989266031734,
0.22355344165575));
#26100=CARTESIAN_POINT('Ctrl Pts',(-0.125650120571794,0.150136503959947,
0.222857488380368));
#26101=CARTESIAN_POINT('Ctrl Pts',(-0.115861791947887,0.157344225081903,
0.222161535104985));
#26102=CARTESIAN_POINT('Ctrl Pts',(-0.11283667685439,0.159571794955527,
0.221946448460613));
#26103=CARTESIAN_POINT('Ctrl Pts',(-0.109750220520155,0.161709939439695,
0.221731361816241));
#26104=CARTESIAN_POINT('Ctrl Pts',(-0.106608316477594,0.163755387263483,
0.221516275171868));
#26105=CARTESIAN_POINT('Ctrl Pts',(-0.0964349244294766,0.170378486614536,
0.220819831000477));
#26106=CARTESIAN_POINT('Ctrl Pts',(-0.0856059651325258,0.176073362452133,
0.220123386829086));
#26107=CARTESIAN_POINT('Ctrl Pts',(-0.0743147751887864,0.18071655759404,
0.219426942657695));
#26108=CARTESIAN_POINT('Ctrl Pts',(-0.0630472832895308,0.185350007558906,
0.218731960189192));
#26109=CARTESIAN_POINT('Ctrl Pts',(-0.0513202596931032,0.188935759214472,
0.218036977720689));
#26110=CARTESIAN_POINT('Ctrl Pts',(-0.0393505492747393,0.191396693471377,
0.217341995252186));
#26111=CARTESIAN_POINT('Ctrl Pts',(-0.0273825254423316,0.193857280971594,
0.216647110709834));
#26112=CARTESIAN_POINT('Ctrl Pts',(-0.0151727298308682,0.195193144473447,
0.215952226167483));
#26113=CARTESIAN_POINT('Ctrl Pts',(-0.00295056508101129,0.195377721774267,
0.215257341625131));
#26114=CARTESIAN_POINT('Ctrl Pts',(0.00927087312890606,0.195562288102988,
0.214562498389813));
#26115=CARTESIAN_POINT('Ctrl Pts',(0.0215038029545236,0.194595717610321,
0.213867655154495));
#26116=CARTESIAN_POINT('Ctrl Pts',(0.0335191997017815,0.192503566853583,
0.213172811919178));
#26117=CARTESIAN_POINT('Ctrl Pts',(0.0455622889237909,0.190406594214287,
0.212476367244543));
#26118=CARTESIAN_POINT('Ctrl Pts',(0.0573859930816696,0.187179076431562,
0.211779922569909));
#26119=CARTESIAN_POINT('Ctrl Pts',(0.0687730616908222,0.182897309946512,
0.211083477895275));
#26120=CARTESIAN_POINT('Ctrl Pts',(0.0724895664205764,0.181499829529067,
0.210856172693548));
#26121=CARTESIAN_POINT('Ctrl Pts',(0.076159718528558,0.179990430187524,
0.21062886749182));
#26122=CARTESIAN_POINT('Ctrl Pts',(0.0797764976032439,0.178372841066569,
0.210401562290093));
#26123=CARTESIAN_POINT('Ctrl Pts',(0.0908580074399471,0.173416682731915,
0.209705118084665));
#26124=CARTESIAN_POINT('Ctrl Pts',(0.101515120126267,0.167406363771345,
0.209008673879237));
#26125=CARTESIAN_POINT('Ctrl Pts',(0.111539265227651,0.160437378165051,
0.208312229673809));
#26126=CARTESIAN_POINT('Ctrl Pts',(0.121542371573814,0.153483019121006,
0.207617247171001));
#26127=CARTESIAN_POINT('Ctrl Pts',(0.130914392769052,0.145574420638768,
0.206922264668194));
#26128=CARTESIAN_POINT('Ctrl Pts',(0.139472943765809,0.136851956351744,
0.206227282165386));
#26129=CARTESIAN_POINT('Ctrl Pts',(0.148030288822697,0.128130721100737,
0.205532397588864));
#26130=CARTESIAN_POINT('Ctrl Pts',(0.155773745952015,0.11859643951404,0.204837513012342));
#26131=CARTESIAN_POINT('Ctrl Pts',(0.16255659831078,0.108427451992692,0.20414262843582));
#26132=CARTESIAN_POINT('Ctrl Pts',(0.169339047466181,0.098259068961871,
0.203447785166374));
#26133=CARTESIAN_POINT('Ctrl Pts',(0.175160541501862,0.0874567982968869,
0.202752941896928));
#26134=CARTESIAN_POINT('Ctrl Pts',(0.179918358774935,0.0762269255298523,
0.202058098627482));
#26135=CARTESIAN_POINT('Ctrl Pts',(0.184687141617781,0.0649711707361879,
0.201361653919412));
#26136=CARTESIAN_POINT('Ctrl Pts',(0.188387071916958,0.0532866775537924,
0.200665209211341));
#26137=CARTESIAN_POINT('Ctrl Pts',(0.190964444600237,0.0413973537623237,
0.19996876450327));
#26138=CARTESIAN_POINT('Ctrl Pts',(0.191805645305132,0.0375169263724499,
0.199741459471619));
#26139=CARTESIAN_POINT('Ctrl Pts',(0.192527675912343,0.033614753752915,
0.199514154439968));
#26140=CARTESIAN_POINT('Ctrl Pts',(0.193129862663858,0.0296987566648717,
0.199286849408317));
#26141=CARTESIAN_POINT('Ctrl Pts',(0.194974913860842,0.0177004602950171,
0.198590405290818));
#26142=CARTESIAN_POINT('Ctrl Pts',(0.195704118410672,0.00548709834586105,
0.197893961173319));
#26143=CARTESIAN_POINT('Ctrl Pts',(0.195284607996036,-0.00671430412138008,
0.197197517055821));
#26144=CARTESIAN_POINT('Ctrl Pts',(0.194865978053238,-0.0188900981868488,
0.196502534640845));
#26145=CARTESIAN_POINT('Ctrl Pts',(0.193303373686754,-0.0310531136309142,
0.19580755222587));
#26146=CARTESIAN_POINT('Ctrl Pts',(0.190615834192916,-0.0429739892835024,
0.195112569810894));
#26147=CARTESIAN_POINT('Ctrl Pts',(0.187928673380375,-0.0548931852537454,
0.194417685320746));
#26148=CARTESIAN_POINT('Ctrl Pts',(0.184117039430817,-0.0665694460773828,
0.193722800830599));
#26149=CARTESIAN_POINT('Ctrl Pts',(0.179251213331651,-0.0777827906360454,
0.193027916340451));
#26150=CARTESIAN_POINT('Ctrl Pts',(0.174385676473917,-0.0889954686349565,
0.192333073156626));
#26151=CARTESIAN_POINT('Ctrl Pts',(0.168466445016061,-0.099744492260233,
0.191638229972801));
#26152=CARTESIAN_POINT('Ctrl Pts',(0.161611136962421,-0.109831691281313,
0.190943386788976));
#26153=CARTESIAN_POINT('Ctrl Pts',(0.154740029123084,-0.119942138795614,
0.190246942163858));
#26154=CARTESIAN_POINT('Ctrl Pts',(0.1469290832769,-0.129387029182578,0.189550497538739));
#26155=CARTESIAN_POINT('Ctrl Pts',(0.138337304105884,-0.137999819901028,
0.188854052913621));
#26156=CARTESIAN_POINT('Ctrl Pts',(0.135533120877919,-0.14081086087379,
0.188626747451261));
#26157=CARTESIAN_POINT('Ctrl Pts',(0.132646044039451,-0.143533566533357,
0.188399441988901));
#26158=CARTESIAN_POINT('Ctrl Pts',(0.129682363299695,-0.146163075532112,
0.188172136526541));
#26159=CARTESIAN_POINT('Ctrl Pts',(0.120601903162391,-0.154219662506403,
0.187475692350802));
#26160=CARTESIAN_POINT('Ctrl Pts',(0.110735649197369,-0.161455338184431,
0.186779248175063));
#26161=CARTESIAN_POINT('Ctrl Pts',(0.100256524520575,-0.167719376611814,
0.186082803999324));
#26162=CARTESIAN_POINT('Ctrl Pts',(0.089799393530819,-0.17397026801547,
0.185387821527279));
#26163=CARTESIAN_POINT('Ctrl Pts',(0.0787326507484688,-0.17925306098191,
0.184692839055233));
#26164=CARTESIAN_POINT('Ctrl Pts',(0.0672593302743625,-0.183459375587742,
0.183997856583187));
#26165=CARTESIAN_POINT('Ctrl Pts',(0.0557876264624159,-0.187665097497704,
0.183302972038491));
#26166=CARTESIAN_POINT('Ctrl Pts',(0.0439102637455561,-0.190794297918841,
0.182608087493795));
#26167=CARTESIAN_POINT('Ctrl Pts',(0.0318501821642357,-0.192786736826227,
0.181913202949099));
#26168=CARTESIAN_POINT('Ctrl Pts',(0.0197908174998791,-0.194779057292188,
0.181218359712126));
#26169=CARTESIAN_POINT('Ctrl Pts',(0.00754962393995063,-0.195634634032994,
0.180523516475154));
#26170=CARTESIAN_POINT('Ctrl Pts',(-0.00464311434237927,-0.195344827137049,
0.179828673238181));
#26171=CARTESIAN_POINT('Ctrl Pts',(-0.0168639538091138,-0.195054352309353,
0.17913222856292));
#26172=CARTESIAN_POINT('Ctrl Pts',(-0.0290352416459393,-0.193613309459193,
0.178435783887658));
#26173=CARTESIAN_POINT('Ctrl Pts',(-0.040930824353633,-0.19106498270937,
0.177739339212397));
#26174=CARTESIAN_POINT('Ctrl Pts',(-0.0448132973973497,-0.19023326137584,
0.177512034023186));
#26175=CARTESIAN_POINT('Ctrl Pts',(-0.0486665021716956,-0.18928399100357,
0.177284728833975));
#26176=CARTESIAN_POINT('Ctrl Pts',(-0.0524829434433919,-0.188219820017759,
0.177057423644765));
#26177=CARTESIAN_POINT('Ctrl Pts',(-0.0641762050919854,-0.184959287786276,
0.176360979270988));
#26178=CARTESIAN_POINT('Ctrl Pts',(-0.0756058517517343,-0.180593370571617,
0.175664534897211));
#26179=CARTESIAN_POINT('Ctrl Pts',(-0.0865514713732667,-0.175185623848313,
0.174968090523434));
#26180=CARTESIAN_POINT('Ctrl Pts',(-0.0974741182626512,-0.169789226936284,
0.174273107851288));
#26181=CARTESIAN_POINT('Ctrl Pts',(-0.107913944199139,-0.163355657667378,
0.173578125179142));
#26182=CARTESIAN_POINT('Ctrl Pts',(-0.117669787918049,-0.155996733976457,
0.172883142506997));
#26183=CARTESIAN_POINT('Ctrl Pts',(-0.127424256977318,-0.148638847204092,
0.172188257762273));
#26184=CARTESIAN_POINT('Ctrl Pts',(-0.136494209348649,-0.140356354588377,
0.17149337301755));
#26185=CARTESIAN_POINT('Ctrl Pts',(-0.144708136496583,-0.131303904099178,
0.170798488272827));
#26186=CARTESIAN_POINT('Ctrl Pts',(-0.15292157536601,-0.122251991734671,
0.170103644835663));
#26187=CARTESIAN_POINT('Ctrl Pts',(-0.160278521350541,-0.112430878895252,
0.169408801398499));
#26188=CARTESIAN_POINT('Ctrl Pts',(-0.166646837862244,-0.102029365530298,
0.168713957961336));
#26189=CARTESIAN_POINT('Ctrl Pts',(-0.17302983170028,-0.0916038793609551,
0.168017513089341));
#26190=CARTESIAN_POINT('Ctrl Pts',(-0.178419245622511,-0.0805961024668422,
0.167321068217346));
#26191=CARTESIAN_POINT('Ctrl Pts',(-0.182728809640674,-0.0692195212877294,
0.166624623345351));
#26192=CARTESIAN_POINT('Ctrl Pts',(-0.184135355966955,-0.0655064569509017,
0.16639731915123));
#26193=CARTESIAN_POINT('Ctrl Pts',(-0.18542726699935,-0.0617542403422105,
0.166170014957109));
#26194=CARTESIAN_POINT('Ctrl Pts',(-0.186602703495507,-0.0579706050353778,
0.165942710762988));
#26195=CARTESIAN_POINT('Ctrl Pts',(-0.190950036443863,-0.0439768907958402,
0.165102029862207));
#26196=CARTESIAN_POINT('Ctrl Pts',(-0.193725456221651,-0.0294728360944788,
0.164261348961425));
#26197=CARTESIAN_POINT('Ctrl Pts',(-0.19484001101867,-0.0147827638229339,
0.163420668060643));
#26198=CARTESIAN_POINT('Ctrl Pts',(-0.195208442835856,-0.00992675312154956,
0.163142769124873));
#26199=CARTESIAN_POINT('Ctrl Pts',(-0.195395767369531,-0.0050505877175918,
0.162864870189103));
#26200=CARTESIAN_POINT('Ctrl Pts',(-0.19539992906386,-0.00016649876455978,
0.162586971253333));
#26201=CARTESIAN_POINT('',(-0.195131096902049,0.000101113969644753,0.092586969212423));
#26202=CARTESIAN_POINT('Ctrl Pts',(-0.195269961073647,-0.00016635217456426,
0.162586969212423));
#26203=CARTESIAN_POINT('Ctrl Pts',(-0.194902238792413,0.0452585421341261,
0.160000645435353));
#26204=CARTESIAN_POINT('Ctrl Pts',(-0.156485712116744,0.156315318469729,
0.153709417364356));
#26205=CARTESIAN_POINT('Ctrl Pts',(0.0284055178284113,0.229205619323633,
0.143713284999436));
#26206=CARTESIAN_POINT('Ctrl Pts',(0.207982494406922,0.100426132144768,
0.132598572117659));
#26207=CARTESIAN_POINT('Ctrl Pts',(0.197161712231624,-0.120288773936243,
0.121483859235884));
#26208=CARTESIAN_POINT('Ctrl Pts',(0.00584918801334944,-0.230884768458966,
0.110369146354108));
#26209=CARTESIAN_POINT('Ctrl Pts',(-0.16458778281091,-0.143557725929993,
0.100736849679621));
#26210=CARTESIAN_POINT('Ctrl Pts',(-0.19494818999653,-0.0390035530360715,
0.0948094572990591));
#26211=CARTESIAN_POINT('Ctrl Pts',(-0.195131096902049,0.000101113969644753,
0.092586969212423));
#26212=CARTESIAN_POINT('Ctrl Pts',(-0.195131096902049,0.000101113969644753,
0.092586969212423));
#26213=CARTESIAN_POINT('Ctrl Pts',(-0.195253097178586,0.026184219880761,
0.0911045530051337));
#26214=CARTESIAN_POINT('Ctrl Pts',(-0.178242552021087,0.117302317988555,
0.0859172325039191));
#26215=CARTESIAN_POINT('Ctrl Pts',(-0.0399751411601922,0.227471578691004,
0.077025007708779));
#26216=CARTESIAN_POINT('Ctrl Pts',(0.169446625860149,0.15694328133998,0.0659102948270026));
#26217=CARTESIAN_POINT('Ctrl Pts',(0.223746334253747,-0.0572705996896112,
0.0547955819452267));
#26218=CARTESIAN_POINT('Ctrl Pts',(0.073221170054178,-0.219033718527302,
0.0436808690634503));
#26219=CARTESIAN_POINT('Ctrl Pts',(-0.136932020372999,-0.181643133843283,
0.0329446976177534));
#26220=CARTESIAN_POINT('Ctrl Pts',(-0.195234758244009,-0.0580117927957973,
0.0259134304659814));
#26221=CARTESIAN_POINT('Ctrl Pts',(-0.19563576606976,0.000124656684744311,
0.022587067608135));
#26222=CARTESIAN_POINT('Origin',(0.,0.,-0.129405622560373));
#26223=CARTESIAN_POINT('',(0.104759235283674,0.114983934194216,2.4));
#26224=CARTESIAN_POINT('Ctrl Pts',(0.104759235283674,0.114983934194216,
2.4));
#26225=CARTESIAN_POINT('Ctrl Pts',(0.116569373796386,0.104223986834125,
2.39879406899067));
#26226=CARTESIAN_POINT('Ctrl Pts',(0.126656121123575,0.0917046658947872,
2.39752488696204));
#26227=CARTESIAN_POINT('Ctrl Pts',(0.136910041192079,0.0739705316573757,
2.39599244051318));
#26228=CARTESIAN_POINT('Ctrl Pts',(0.138990080658535,0.0699840267182179,
2.39566173348939));
#26229=CARTESIAN_POINT('Ctrl Pts',(0.141302013217873,0.0650420429405182,
2.39526750720927));
#26230=CARTESIAN_POINT('Ctrl Pts',(0.141701216126826,0.0641676843380198,
2.39519833532576));
#26231=CARTESIAN_POINT('Ctrl Pts',(0.142313711985314,0.0627925633649434,
2.39509042818814));
#26232=CARTESIAN_POINT('Ctrl Pts',(0.142532518921949,0.0622942990681896,
2.39505150836491));
#26233=CARTESIAN_POINT('Ctrl Pts',(0.142915965079838,0.06140852286273,2.39498263294686));
#26234=CARTESIAN_POINT('Ctrl Pts',(0.143081653201886,0.0610214739101778,
2.39495264259946));
#26235=CARTESIAN_POINT('Ctrl Pts',(0.143459931281017,0.0601278011410767,
2.39488363652743));
#26236=CARTESIAN_POINT('Ctrl Pts',(0.143671413572795,0.05962071191288,2.39484465788404));
#26237=CARTESIAN_POINT('Ctrl Pts',(0.144244563817985,0.0582256606757036,
2.39473790025333));
#26238=CARTESIAN_POINT('Ctrl Pts',(0.144600720111675,0.0573354477356837,
2.39467030328277));
#26239=CARTESIAN_POINT('Ctrl Pts',(0.146388334651106,0.0527446755254263,
2.39432431936592));
#26240=CARTESIAN_POINT('Ctrl Pts',(0.147686139758198,0.0489934067215972,
2.39405032203227));
#26241=CARTESIAN_POINT('Ctrl Pts',(0.153461192843779,0.0299751782671007,
2.39269589807151));
#26242=CARTESIAN_POINT('Ctrl Pts',(0.155720448807173,0.0141377171635735,
2.39168795703575));
#26243=CARTESIAN_POINT('Ctrl Pts',(0.1555095411221,-0.00444786906095659,
2.39040901501096));
#26244=CARTESIAN_POINT('Ctrl Pts',(0.155409692815497,-0.00712923865114926,
2.39022190320889));
#26245=CARTESIAN_POINT('Ctrl Pts',(0.15520553410147,-0.0103611578266905,
2.38999178303995));
#26246=CARTESIAN_POINT('Ctrl Pts',(0.155167522712346,-0.0109156437366008,
2.38995213882522));
#26247=CARTESIAN_POINT('Ctrl Pts',(0.155104024069529,-0.0117744413034399,
2.38989046700507));
#26248=CARTESIAN_POINT('Ctrl Pts',(0.155080610331675,-0.0120789091181799,
2.38986854995593));
#26249=CARTESIAN_POINT('Ctrl Pts',(0.155056210688231,-0.0123844268449986,
2.38984650266975));
#26250=CARTESIAN_POINT('Ctrl Pts',(0.155056120886389,-0.0123855511358104,
2.38984642153603));
#26251=CARTESIAN_POINT('Ctrl Pts',(0.155055940024575,-0.0123878151585674,
2.3898462581528));
#26252=CARTESIAN_POINT('Ctrl Pts',(0.155055848964433,-0.0123889548883746,
2.38984617590343));
#26253=CARTESIAN_POINT('Ctrl Pts',(0.155055665561528,-0.0123912500828242,
2.38984601026762));
#26254=CARTESIAN_POINT('Ctrl Pts',(0.155055573218514,-0.0123924055462099,
2.38984592688126));
#26255=CARTESIAN_POINT('Ctrl Pts',(0.155055387224824,-0.0123947325078486,
2.38984575894976));
#26256=CARTESIAN_POINT('Ctrl Pts',(0.155055293573659,-0.0123959040076737,
2.3898456744045));
#26257=CARTESIAN_POINT('Ctrl Pts',(0.155055104937755,-0.012398263352653,
2.38984550413272));
#26258=CARTESIAN_POINT('Ctrl Pts',(0.155055009952702,-0.0123994511970267,
2.38984541840624));
#26259=CARTESIAN_POINT('Ctrl Pts',(0.155054818622254,-0.0124018435516719,
2.38984524574885));
#26260=CARTESIAN_POINT('Ctrl Pts',(0.15505472227678,-0.0124030480580616,
2.38984515881818));
#26261=CARTESIAN_POINT('Ctrl Pts',(0.155054528198523,-0.0124054740592664,
2.38984498372906));
#26262=CARTESIAN_POINT('Ctrl Pts',(0.155054430465124,-0.0124066955567403,
2.38984489557038));
#26263=CARTESIAN_POINT('Ctrl Pts',(0.155054233583061,-0.0124091558743604,
2.38984471800104));
#26264=CARTESIAN_POINT('Ctrl Pts',(0.155054134434034,-0.012410394693849,
2.3898446285904));
#26265=CARTESIAN_POINT('Ctrl Pts',(0.155053934692053,-0.0124128899979582,
2.38984444849233));
#26266=CARTESIAN_POINT('Ctrl Pts',(0.155053834098541,-0.0124141464841883,
2.38984435780476));
#26267=CARTESIAN_POINT('Ctrl Pts',(0.155053631438168,-0.0124166774731176,
2.3898441751274));
#26268=CARTESIAN_POINT('Ctrl Pts',(0.155053529370771,-0.0124179519769673,
2.3898440831375));
#26269=CARTESIAN_POINT('Ctrl Pts',(0.155053323732169,-0.0124205193647189,
2.38984389782916));
#26270=CARTESIAN_POINT('Ctrl Pts',(0.155053220160708,-0.0124218122461009,
2.38984380451087));
#26271=CARTESIAN_POINT('Ctrl Pts',(0.155053011482959,-0.0124244167588192,
2.38984361651896));
#26272=CARTESIAN_POINT('Ctrl Pts',(0.155052906376181,-0.012425728390341,
2.3898435218453));
#26273=CARTESIAN_POINT('Ctrl Pts',(0.155052694596044,-0.0124283707817298,
2.38984333111526));
#26274=CARTESIAN_POINT('Ctrl Pts',(0.155052587922058,-0.012429701543272,
2.38984323505873));
#26275=CARTESIAN_POINT('Ctrl Pts',(0.155052372974972,-0.0124323825819943,
2.38984304153488));
#26276=CARTESIAN_POINT('Ctrl Pts',(0.155052264700915,-0.0124337328647711,
2.38984294406714));
#26277=CARTESIAN_POINT('Ctrl Pts',(0.155052046519325,-0.0124364533553029,
2.38984274769124));
#26278=CARTESIAN_POINT('Ctrl Pts',(0.155051936611995,-0.0124378235539526,
2.38984264878371));
#26279=CARTESIAN_POINT('Ctrl Pts',(0.155051715129383,-0.0124405842862295,
2.38984244949855));
#26280=CARTESIAN_POINT('Ctrl Pts',(0.155051603553495,-0.0124419748205716,
2.38984234912083));
#26281=CARTESIAN_POINT('Ctrl Pts',(0.155051378698546,-0.0124447766426194,
2.38984214686499));
#26282=CARTESIAN_POINT('Ctrl Pts',(0.155051265418725,-0.012446187932723,
2.38984204498665));
#26283=CARTESIAN_POINT('Ctrl Pts',(0.155051037119204,-0.0124490317022854,
2.389841839698));
#26284=CARTESIAN_POINT('Ctrl Pts',(0.155050922098996,-0.0124504641807515,
2.38984173628772));
#26285=CARTESIAN_POINT('Ctrl Pts',(0.155050690280845,-0.0124533507764655,
2.38984152790262));
#26286=CARTESIAN_POINT('Ctrl Pts',(0.155050573482625,-0.0124548048895616,
2.38984142292807));
#26287=CARTESIAN_POINT('Ctrl Pts',(0.15505033807006,-0.0124577352096343,
2.38984121138146));
#26288=CARTESIAN_POINT('Ctrl Pts',(0.155050219454883,-0.0124592114191003,
2.38984110480919));
#26289=CARTESIAN_POINT('Ctrl Pts',(0.155049980368852,-0.012462186400449,
2.3898408900332));
#26290=CARTESIAN_POINT('Ctrl Pts',(0.155049859897092,-0.0124636851754628,
2.38984078182922));
#26291=CARTESIAN_POINT('Ctrl Pts',(0.15504961705678,-0.0124667057748541,
2.38984056375454));
#26292=CARTESIAN_POINT('Ctrl Pts',(0.155049494687644,-0.0124682275980645,
2.38984045388388));
#26293=CARTESIAN_POINT('Ctrl Pts',(0.155049248010524,-0.012471294791423,
2.38984023243981));
#26294=CARTESIAN_POINT('Ctrl Pts',(0.155049123701721,-0.012472840163012,
2.38984012086624));
#26295=CARTESIAN_POINT('Ctrl Pts',(0.155048873101805,-0.0124759549670296,
2.38983989597911));
#26296=CARTESIAN_POINT('Ctrl Pts',(0.155048746810194,-0.0124775243965821,
2.38983978266571));
#26297=CARTESIAN_POINT('Ctrl Pts',(0.155048492200137,-0.0124806878424747,
2.3898395542608));
#26298=CARTESIAN_POINT('Ctrl Pts',(0.155048363880935,-0.0124822818587952,
2.38983943916926));
#26299=CARTESIAN_POINT('Ctrl Pts',(0.155048105170051,-0.0124854950168308,
2.38983920716902));
#26300=CARTESIAN_POINT('Ctrl Pts',(0.155047974777361,-0.0124871141613046,
2.3898390902601));
#26301=CARTESIAN_POINT('Ctrl Pts',(0.155047711872207,-0.0124903781334359,
2.38983885458469));
#26302=CARTESIAN_POINT('Ctrl Pts',(0.155047579358919,-0.0124920229611797,
2.38983873581815));
#26303=CARTESIAN_POINT('Ctrl Pts',(0.155047312163825,-0.0124953388743151,
2.3898384963859));
#26304=CARTESIAN_POINT('Ctrl Pts',(0.155047177481234,-0.0124970099589203,
2.38983837572019));
#26305=CARTESIAN_POINT('Ctrl Pts',(0.1550262042962,-0.0127571838369673,
2.38981958882283));
#26306=CARTESIAN_POINT('Ctrl Pts',(0.1550047198774,-0.0130156279923222,
2.38980088721687));
#26307=CARTESIAN_POINT('Ctrl Pts',(0.15495389007473,-0.0136090981167331,
2.38975785013479));
#26308=CARTESIAN_POINT('Ctrl Pts',(0.154924104929042,-0.0139440778482577,
2.38973349109876));
#26309=CARTESIAN_POINT('Ctrl Pts',(0.154829757429084,-0.0149675274166969,
2.38965886812692));
#26310=CARTESIAN_POINT('Ctrl Pts',(0.154761691475387,-0.0156556528715037,
2.38960841819265));
#26311=CARTESIAN_POINT('Ctrl Pts',(0.153884679363036,-0.0239565647087003,
2.38899667448546));
#26312=CARTESIAN_POINT('Ctrl Pts',(0.152519468505603,-0.0314990607237558,
2.38840917103484));
#26313=CARTESIAN_POINT('Ctrl Pts',(0.148526520284105,-0.0469544457626036,
2.38717440265638));
#26314=CARTESIAN_POINT('Ctrl Pts',(0.145806548278979,-0.0548207718843048,
2.38652854545728));
#26315=CARTESIAN_POINT('Ctrl Pts',(0.140675311565931,-0.0665302598501802,
2.38555744753643));
#26316=CARTESIAN_POINT('Ctrl Pts',(0.138703525794674,-0.0705489726079016,
2.38522206495621));
#26317=CARTESIAN_POINT('Ctrl Pts',(0.13526802848711,-0.0768482638195142,
2.38469328468739));
#26318=CARTESIAN_POINT('Ctrl Pts',(0.1339134391031,-0.0791851482048425,
2.38449638440864));
#26319=CARTESIAN_POINT('Ctrl Pts',(0.132074980580046,-0.082174545623346,
2.38424333895301));
#26320=CARTESIAN_POINT('Ctrl Pts',(0.13164598316403,-0.0828600724473197,
2.38418522797746));
#26321=CARTESIAN_POINT('Ctrl Pts',(0.130939638441512,-0.0839694593102859,
2.38409104100489));
#26322=CARTESIAN_POINT('Ctrl Pts',(0.130665537400066,-0.0843953574501554,
2.38405484681215));
#26323=CARTESIAN_POINT('Ctrl Pts',(0.130134459947668,-0.0852117559223193,
2.38398539468413));
#26324=CARTESIAN_POINT('Ctrl Pts',(0.129877794261211,-0.0856024507813227,
2.38395212576083));
#26325=CARTESIAN_POINT('Ctrl Pts',(0.12928616605323,-0.0864942370727429,
2.38387611015374));
#26326=CARTESIAN_POINT('Ctrl Pts',(0.128950042879631,-0.0869945529289769,
2.38383340720542));
#26327=CARTESIAN_POINT('Ctrl Pts',(0.128049619270603,-0.0883181389949518,
2.38372027667117));
#26328=CARTESIAN_POINT('Ctrl Pts',(0.127480281856383,-0.0891379632401997,
2.38365003851123));
#26329=CARTESIAN_POINT('Ctrl Pts',(0.123161191456086,-0.0952312601868546,
2.38312660497771));
#26330=CARTESIAN_POINT('Ctrl Pts',(0.119093248057888,-0.100272068148527,
2.38268608754341));
#26331=CARTESIAN_POINT('Ctrl Pts',(0.10762137765009,-0.11280077759827,2.38154957650148));
#26332=CARTESIAN_POINT('Ctrl Pts',(0.0997523984692161,-0.119815795561994,
2.38087010831843));
#26333=CARTESIAN_POINT('Ctrl Pts',(0.0879178224206822,-0.128386312542348,
2.3798944733156));
#26334=CARTESIAN_POINT('Ctrl Pts',(0.0845061164354837,-0.130657182580203,
2.37961761469993));
#26335=CARTESIAN_POINT('Ctrl Pts',(0.0792176263915553,-0.133883433784787,
2.37918863032341));
#26336=CARTESIAN_POINT('Ctrl Pts',(0.0774043624997727,-0.134939874273829,
2.37904156940106));
#26337=CARTESIAN_POINT('Ctrl Pts',(0.0751285530480621,-0.136204840481189,
2.37885630925911));
#26338=CARTESIAN_POINT('Ctrl Pts',(0.0746855116924439,-0.136448277298856,
2.37882021217369));
#26339=CARTESIAN_POINT('Ctrl Pts',(0.0739851104910756,-0.136828691875197,
2.37876308390526));
#26340=CARTESIAN_POINT('Ctrl Pts',(0.073728533316691,-0.136967116001675,
2.37874214299667));
#26341=CARTESIAN_POINT('Ctrl Pts',(0.0732501280673066,-0.137223483256614,
2.37870306990078));
#26342=CARTESIAN_POINT('Ctrl Pts',(0.0730284030408225,-0.137341610466722,
2.37868494968358));
#26343=CARTESIAN_POINT('Ctrl Pts',(0.0725233253336301,-0.137609129013633,
2.3786436473589));
#26344=CARTESIAN_POINT('Ctrl Pts',(0.0722397996698917,-0.137758181041784,
2.37862044445164));
#26345=CARTESIAN_POINT('Ctrl Pts',(0.0713940185817091,-0.138199486819721,
2.37855117971983));
#26346=CARTESIAN_POINT('Ctrl Pts',(0.0708304449827274,-0.138489176735052,
2.37850496259013));
#26347=CARTESIAN_POINT('Ctrl Pts',(0.0665719760524741,-0.140645335941587,
2.3781553468359));
#26348=CARTESIAN_POINT('Ctrl Pts',(0.062806042893632,-0.142366891756567,
2.37784399831596));
#26349=CARTESIAN_POINT('Ctrl Pts',(0.0475972922137978,-0.148598530202747,
2.37659008370091));
#26350=CARTESIAN_POINT('Ctrl Pts',(0.0357051342040492,-0.151895406406671,
2.37562152280738));
#26351=CARTESIAN_POINT('Ctrl Pts',(0.0192972601592593,-0.154408253241854,
2.3743618554564));
#26352=CARTESIAN_POINT('Ctrl Pts',(0.0150212780361088,-0.154882731056818,
2.3740398479449));
#26353=CARTESIAN_POINT('Ctrl Pts',(0.00811726951375727,-0.15536014729364,
2.37353021394204));
#26354=CARTESIAN_POINT('Ctrl Pts',(0.00549950352845257,-0.155474829010473,
2.37333932123971));
#26355=CARTESIAN_POINT('Ctrl Pts',(0.00208643395044463,-0.155538031209154,
2.37309329505412));
#26356=CARTESIAN_POINT('Ctrl Pts',(0.00129281909216219,-0.155546652234968,
2.37303628892556));
#26357=CARTESIAN_POINT('Ctrl Pts',(1.62816883083261E-7,-0.155550800383033,
2.37294375214716));
#26358=CARTESIAN_POINT('Ctrl Pts',(-0.000498843587911407,-0.155550000532587,
2.37290810667281));
#26359=CARTESIAN_POINT('Ctrl Pts',(-0.00145968219985443,-0.155543836689673,
2.37283961528841));
#26360=CARTESIAN_POINT('Ctrl Pts',(-0.00192151049930675,-0.15553881705271,
2.37280675892364));
#26361=CARTESIAN_POINT('Ctrl Pts',(-0.00298051274202501,-0.155522589271181,
2.37273156053725));
#26362=CARTESIAN_POINT('Ctrl Pts',(-0.00357766107942544,-0.155509998357584,
2.3726892623878));
#26363=CARTESIAN_POINT('Ctrl Pts',(-0.00516715045182625,-0.155467323463744,
2.37257694168457));
#26364=CARTESIAN_POINT('Ctrl Pts',(-0.00615931330712721,-0.155431177856745,
2.37250710968175));
#26365=CARTESIAN_POINT('Ctrl Pts',(-0.0137410745203418,-0.155082253463266,
2.37197546235925));
#26366=CARTESIAN_POINT('Ctrl Pts',(-0.0203056524830594,-0.154360038189527,
2.37152701798302));
#26367=CARTESIAN_POINT('Ctrl Pts',(-0.037285816274013,-0.151389475245343,
2.37037570735659));
#26368=CARTESIAN_POINT('Ctrl Pts',(-0.0475499993521492,-0.148485651933286,
2.36968957644462));
#26369=CARTESIAN_POINT('Ctrl Pts',(-0.0610558234716782,-0.143119359274682,
2.36871834511214));
#26370=CARTESIAN_POINT('Ctrl Pts',(-0.0646189346133087,-0.141546292094857,
2.36845489966616));
#26371=CARTESIAN_POINT('Ctrl Pts',(-0.0699384917027309,-0.138955050627056,
2.36804496020318));
#26372=CARTESIAN_POINT('Ctrl Pts',(-0.0717404232971153,-0.138033363048832,
2.36790308473609));
#26373=CARTESIAN_POINT('Ctrl Pts',(-0.0739612288765335,-0.136842192252523,
2.36772378993123));
#26374=CARTESIAN_POINT('Ctrl Pts',(-0.0743975817882275,-0.136605449244348,
2.36768834457107));
#26375=CARTESIAN_POINT('Ctrl Pts',(-0.0750866579090631,-0.136227310638504,
2.36763201391692));
#26376=CARTESIAN_POINT('Ctrl Pts',(-0.0753401375512388,-0.136087288273885,
2.36761121565407));
#26377=CARTESIAN_POINT('Ctrl Pts',(-0.0758192264837021,-0.135820890390524,
2.36757175744182));
#26378=CARTESIAN_POINT('Ctrl Pts',(-0.0760449135485121,-0.13569465903409,
2.36755310681805));
#26379=CARTESIAN_POINT('Ctrl Pts',(-0.0765606930099079,-0.135404482271449,
2.36751034080948));
#26380=CARTESIAN_POINT('Ctrl Pts',(-0.0768505748603377,-0.135240166634578,
2.36748620178436));
#26381=CARTESIAN_POINT('Ctrl Pts',(-0.0776185794178367,-0.134801566996752,
2.36742197813306));
#26382=CARTESIAN_POINT('Ctrl Pts',(-0.0780957700560277,-0.134525674168724,
2.36738179420472));
#26383=CARTESIAN_POINT('Ctrl Pts',(-0.0814141682137354,-0.132583500873867,
2.36710045245604));
#26384=CARTESIAN_POINT('Ctrl Pts',(-0.0842030383169656,-0.130830026029818,
2.36685425420449));
#26385=CARTESIAN_POINT('Ctrl Pts',(-0.0880805307994597,-0.128216748570522,
2.36650001274247));
#26386=CARTESIAN_POINT('Ctrl Pts',(-0.0892167937467142,-0.127428717417893,
2.36639468937984));
#26387=CARTESIAN_POINT('Ctrl Pts',(-0.0913568074056298,-0.125901902927371,
2.36619361249075));
#26388=CARTESIAN_POINT('Ctrl Pts',(-0.0923624946677538,-0.125165989324826,
2.36609794737246));
#26389=CARTESIAN_POINT('Ctrl Pts',(-0.104880435575903,-0.115772940957153,
2.36489324984584));
#26390=CARTESIAN_POINT('Ctrl Pts',(-0.115148035305615,-0.105566905191347,
2.36376479872363));
#26391=CARTESIAN_POINT('Ctrl Pts',(-0.125701779821125,-0.091673827059514,
2.36247507984567));
#26392=CARTESIAN_POINT('Ctrl Pts',(-0.127467955827375,-0.0892017413483719,
2.36225321909189));
#26393=CARTESIAN_POINT('Ctrl Pts',(-0.129629484486658,-0.0859808518666029,
2.36197342586439));
#26394=CARTESIAN_POINT('Ctrl Pts',(-0.130092578962798,-0.0852785499775909,
2.36191296224966));
#26395=CARTESIAN_POINT('Ctrl Pts',(-0.130828799568427,-0.0841420865015539,
2.36181597908327));
#26396=CARTESIAN_POINT('Ctrl Pts',(-0.131105509857546,-0.0837102790219607,
2.36177932687718));
#26397=CARTESIAN_POINT('Ctrl Pts',(-0.131628582559035,-0.0828850662123731,
2.36170965286161));
#26398=CARTESIAN_POINT('Ctrl Pts',(-0.131875328951331,-0.0824919121492293,
2.36167661716648));
#26399=CARTESIAN_POINT('Ctrl Pts',(-0.132434749791534,-0.0815916323945268,
2.3616013272399));
#26400=CARTESIAN_POINT('Ctrl Pts',(-0.132746279469288,-0.0810838006882076,
2.36155911523679));
#26401=CARTESIAN_POINT('Ctrl Pts',(-0.133549926558461,-0.0797567109642289,
2.36144946386094));
#26402=CARTESIAN_POINT('Ctrl Pts',(-0.134037430604619,-0.0789346761347597,
2.36138219189014));
#26403=CARTESIAN_POINT('Ctrl Pts',(-0.137280067956952,-0.0733502300511387,
2.36092942835196));
#26404=CARTESIAN_POINT('Ctrl Pts',(-0.139788635886577,-0.0684486805213911,
2.36055293618593));
#26405=CARTESIAN_POINT('Ctrl Pts',(-0.148095241906383,-0.0498467703231422,
2.35918168311549));
#26406=CARTESIAN_POINT('Ctrl Pts',(-0.152179113346546,-0.0354726472762498,
2.35823929183334));
#26407=CARTESIAN_POINT('Ctrl Pts',(-0.154507966389611,-0.018161934973515,
2.35703742847534));
#26408=CARTESIAN_POINT('Ctrl Pts',(-0.154790021417189,-0.0155760937493597,
2.35685598884916));
#26409=CARTESIAN_POINT('Ctrl Pts',(-0.155052295667947,-0.0124451271287232,
2.35663267220013));
#26410=CARTESIAN_POINT('Ctrl Pts',(-0.155094669173755,-0.0119054253128199,
2.35659404801459));
#26411=CARTESIAN_POINT('Ctrl Pts',(-0.155156281376314,-0.0110644468220585,
2.35653364497798));
#26412=CARTESIAN_POINT('Ctrl Pts',(-0.155177462272496,-0.010763309549938,
2.35651197242452));
#26413=CARTESIAN_POINT('Ctrl Pts',(-0.155215151605479,-0.0102042161232831,
2.35647165116354));
#26414=CARTESIAN_POINT('Ctrl Pts',(-0.155231893726048,-0.00994627979441159,
2.35645301568399));
#26415=CARTESIAN_POINT('Ctrl Pts',(-0.155268332411986,-0.00936237637902016,
2.3564107540604));
#26416=CARTESIAN_POINT('Ctrl Pts',(-0.155287645260742,-0.00903639117765526,
2.35638710704518));
#26417=CARTESIAN_POINT('Ctrl Pts',(-0.155342996497391,-0.00804947633369134,
2.35631536070114));
#26418=CARTESIAN_POINT('Ctrl Pts',(-0.155375842157526,-0.00738838694983366,
2.35626709021258));
#26419=CARTESIAN_POINT('Ctrl Pts',(-0.155597422658225,-0.00226961719401098,
2.3558918046594));
#26420=CARTESIAN_POINT('Ctrl Pts',(-0.155598482864865,0.00219363379957986,
2.35555564534585));
#26421=CARTESIAN_POINT('Ctrl Pts',(-0.154768234457253,0.0215955998681862,
2.35407160552423));
#26422=CARTESIAN_POINT('Ctrl Pts',(-0.151975677561831,0.0363747912655102,
2.35289228841612));
#26423=CARTESIAN_POINT('Ctrl Pts',(-0.145908861679386,0.0540387766803025,
2.35150345769644));
#26424=CARTESIAN_POINT('Ctrl Pts',(-0.144577515450517,0.057505927437592,
2.3512312760094));
#26425=CARTESIAN_POINT('Ctrl Pts',(-0.142771863936644,0.0617478929263152,
2.3508984255192));
#26426=CARTESIAN_POINT('Ctrl Pts',(-0.142413338486806,0.0625703483803747,
2.35083389562364));
#26427=CARTESIAN_POINT('Ctrl Pts',(-0.141833964948203,0.0638686463804223,
2.35073202472981));
#26428=CARTESIAN_POINT('Ctrl Pts',(-0.141617796089092,0.0643465418394741,
2.35069452527094));
#26429=CARTESIAN_POINT('Ctrl Pts',(-0.141207132078897,0.0652423236229802,
2.35062422855432));
#26430=CARTESIAN_POINT('Ctrl Pts',(-0.141013189305969,0.0656604553122312,
2.35059141283929));
#26431=CARTESIAN_POINT('Ctrl Pts',(-0.140573878375023,0.0665966652099511,
2.3505179278292));
#26432=CARTESIAN_POINT('Ctrl Pts',(-0.140327498128499,0.0671142636362083,
2.35047729385793));
#26433=CARTESIAN_POINT('Ctrl Pts',(-0.139693852958658,0.0684266880519785,
2.35037423703304));
#26434=CARTESIAN_POINT('Ctrl Pts',(-0.139302658561361,0.0692196039236709,
2.35031195055833));
#26435=CARTESIAN_POINT('Ctrl Pts',(-0.136991318876314,0.0738055181699215,
2.34995149497577));
#26436=CARTESIAN_POINT('Ctrl Pts',(-0.134922960566627,0.0775221018112844,
2.3496585801293));
#26437=CARTESIAN_POINT('Ctrl Pts',(-0.131842760910188,0.0825591842526366,
2.34925765971958));
#26438=CARTESIAN_POINT('Ctrl Pts',(-0.130958354020009,0.0839550015511547,
2.34914611366222));
#26439=CARTESIAN_POINT('Ctrl Pts',(-0.122055105888294,0.0975234507064667,
2.3480558432599));
#26440=CARTESIAN_POINT('Ctrl Pts',(-0.112386401634549,0.108524038230606,
2.34713140761696));
#26441=CARTESIAN_POINT('Ctrl Pts',(-0.0992539383505594,0.119799601629702,
2.34594251052381));
#26442=CARTESIAN_POINT('Ctrl Pts',(-0.0971315254245216,0.121526758883124,
2.34575187953925));
#26443=CARTESIAN_POINT('Ctrl Pts',(-0.0945311764809605,0.123531206609171,
2.34551855845236));
#26444=CARTESIAN_POINT('Ctrl Pts',(-0.0940957427491966,0.123863204809224,
2.34547949606559));
#26445=CARTESIAN_POINT('Ctrl Pts',(-0.0934171873717764,0.124374929182501,
2.34541861931852));
#26446=CARTESIAN_POINT('Ctrl Pts',(-0.0931752733715439,0.124556261719363,
2.34539691514289));
#26447=CARTESIAN_POINT('Ctrl Pts',(-0.0927264357954126,0.124890659585645,
2.34535664137385));
#26448=CARTESIAN_POINT('Ctrl Pts',(-0.0925196603170567,0.125043917079547,
2.34533808550703));
#26449=CARTESIAN_POINT('Ctrl Pts',(-0.0920524846099039,0.125388384413902,
2.34529615694643));
#26450=CARTESIAN_POINT('Ctrl Pts',(-0.0917918703910129,0.125579295243042,
2.34527276418319));
#26451=CARTESIAN_POINT('Ctrl Pts',(-0.0910241728054328,0.126137999324275,
2.34520385159877));
#26452=CARTESIAN_POINT('Ctrl Pts',(-0.090515468499498,0.126503536847386,
2.34515818257502));
#26453=CARTESIAN_POINT('Ctrl Pts',(-0.0869340474896806,0.129044362151233,
2.34483670254938));
#26454=CARTESIAN_POINT('Ctrl Pts',(-0.0837857480964293,0.131110329595634,
2.34455434347846));
#26455=CARTESIAN_POINT('Ctrl Pts',(-0.0797111245064023,0.133577459955539,
2.34419206343651));
#26456=CARTESIAN_POINT('Ctrl Pts',(-0.078851322236165,0.134086800562523,
2.34411578760551));
#26457=CARTESIAN_POINT('Ctrl Pts',(-0.0733888200384716,0.137252038576912,
2.34363250315201));
#26458=CARTESIAN_POINT('Ctrl Pts',(-0.0686576019598595,0.139678813674574,
2.34321990111197));
#26459=CARTESIAN_POINT('Ctrl Pts',(-0.0637706568557826,0.141877087107655,
2.34280436535828));
#26460=CARTESIAN_POINT('Ctrl Pts',(-0.0637296451045094,0.141895513869592,
2.34280087886671));
#26461=CARTESIAN_POINT('Ctrl Pts',(-0.063688625846537,0.141913922635448,
2.34279739246514));
#26462=CARTESIAN_POINT('',(0.143545299885862,-0.0599211930845659,2.4));
#26463=CARTESIAN_POINT('Origin',(0.,0.,2.4));
#26464=CARTESIAN_POINT('',(-0.155549935368252,0.000141798916507806,2.36940562256037));
#26465=CARTESIAN_POINT('Ctrl Pts',(-0.155549935368252,0.000141798916507806,
2.36940562256037));
#26466=CARTESIAN_POINT('Ctrl Pts',(-0.155559235828691,-0.0100605781955904,
2.37013602172971));
#26467=CARTESIAN_POINT('Ctrl Pts',(-0.154560452504158,-0.0202869430343912,
2.37086642089906));
#26468=CARTESIAN_POINT('Ctrl Pts',(-0.152565879395267,-0.0303225154686899,
2.3715968200684));
#26469=CARTESIAN_POINT('Ctrl Pts',(-0.150573087012895,-0.0403491282865703,
2.37232656714775));
#26470=CARTESIAN_POINT('Ctrl Pts',(-0.147586439117774,-0.0501843583611561,
2.37305631422709));
#26471=CARTESIAN_POINT('Ctrl Pts',(-0.143669539331068,-0.0596226967555041,
2.37378606130644));
#26472=CARTESIAN_POINT('Ctrl Pts',(-0.139743199481172,-0.0690837823518981,
2.3745175671386));
#26473=CARTESIAN_POINT('Ctrl Pts',(-0.134882515659627,-0.078145198024074,
2.37524907297077));
#26474=CARTESIAN_POINT('Ctrl Pts',(-0.12919902487086,-0.0866222516009543,
2.37598057880293));
#26475=CARTESIAN_POINT('Ctrl Pts',(-0.124563189169144,-0.0935367041931399,
2.37657724394744));
#26476=CARTESIAN_POINT('Ctrl Pts',(-0.119380988048105,-0.100062643096905,
2.37717390909194));
#26477=CARTESIAN_POINT('Ctrl Pts',(-0.113732697104638,-0.106116332905471,
2.37777057423645));
#26478=CARTESIAN_POINT('Ctrl Pts',(-0.106829383557614,-0.113515122961299,
2.37849981545584));
#26479=CARTESIAN_POINT('Ctrl Pts',(-0.0991717628314197,-0.120268582175319,
2.37922905667523));
#26480=CARTESIAN_POINT('Ctrl Pts',(-0.0909057529026238,-0.126221815028968,
2.37995829789462));
#26481=CARTESIAN_POINT('Ctrl Pts',(-0.0824734057365558,-0.13229484501742,
2.38070221366325));
#26482=CARTESIAN_POINT('Ctrl Pts',(-0.0734085507228057,-0.137534273118749,
2.38144612943189));
#26483=CARTESIAN_POINT('Ctrl Pts',(-0.0639035509383708,-0.141817272140833,
2.38219004520052));
#26484=CARTESIAN_POINT('Ctrl Pts',(-0.0546060702612576,-0.146006762046254,
2.38291771933425));
#26485=CARTESIAN_POINT('Ctrl Pts',(-0.0448884161511158,-0.149280862880942,
2.38364539346799));
#26486=CARTESIAN_POINT('Ctrl Pts',(-0.0349538919347246,-0.151571857343689,
2.38437306760172));
#26487=CARTESIAN_POINT('Ctrl Pts',(-0.0246867609076323,-0.153939554056588,
2.3851251041878));
#26488=CARTESIAN_POINT('Ctrl Pts',(-0.0141889885206651,-0.155256727301847,
2.38587714077389));
#26489=CARTESIAN_POINT('Ctrl Pts',(-0.00369546276844564,-0.155506096520127,
2.38662917735997));
#26490=CARTESIAN_POINT('Ctrl Pts',(0.00679806298377526,-0.155755465738407,
2.38738121394606));
#26491=CARTESIAN_POINT('Ctrl Pts',(0.017286243111928,-0.154937181577277,
2.38813325053214));
#26492=CARTESIAN_POINT('Ctrl Pts',(0.0275400002621714,-0.153092621917451,
2.38888528711823));
#26493=CARTESIAN_POINT('Ctrl Pts',(0.0378733824294785,-0.151233738425664,
2.38964316360525));
#26494=CARTESIAN_POINT('Ctrl Pts',(0.0480492838063025,-0.148318709903011,
2.39040104009227));
#26495=CARTESIAN_POINT('Ctrl Pts',(0.0578456617134533,-0.144394189360004,
2.39115891657929));
#26496=CARTESIAN_POINT('Ctrl Pts',(0.0676191605628735,-0.140478834381343,
2.3919150230754));
#26497=CARTESIAN_POINT('Ctrl Pts',(0.0770140719283949,-0.13555891450073,
2.39267112957151));
#26498=CARTESIAN_POINT('Ctrl Pts',(0.0858240262363051,-0.129730640253527,
2.39342723606762));
#26499=CARTESIAN_POINT('Ctrl Pts',(0.0946200577567245,-0.123911576703786,
2.39418214765287));
#26500=CARTESIAN_POINT('Ctrl Pts',(0.102832228730433,-0.117187452514392,
2.39493705923811));
#26501=CARTESIAN_POINT('Ctrl Pts',(0.110281164467125,-0.109698984789171,
2.39569197082336));
#26502=CARTESIAN_POINT('Ctrl Pts',(0.117734845393054,-0.102205746691685,
2.3964473633093));
#26503=CARTESIAN_POINT('Ctrl Pts',(0.124423690575448,-0.0939477881347089,
2.39720275579524));
#26504=CARTESIAN_POINT('Ctrl Pts',(0.130204459076775,-0.0851034742917383,
2.39795814828117));
#26505=CARTESIAN_POINT('Ctrl Pts',(0.135412997384256,-0.0771346467138956,
2.39863876552078));
#26506=CARTESIAN_POINT('Ctrl Pts',(0.139884590728665,-0.0686906712393692,
2.39931938276039));
#26507=CARTESIAN_POINT('Ctrl Pts',(0.143545299885862,-0.059921193084566,
2.4));
#26508=CARTESIAN_POINT('Ctrl Pts',(-0.155549934503847,0.000142743998182768,
2.36941789089093));
#26509=CARTESIAN_POINT('Ctrl Pts',(-0.155540753141536,0.0101477902640131,
2.36864722383324));
#26510=CARTESIAN_POINT('Ctrl Pts',(-0.154566316755707,0.020129469112165,
2.36786767664586));
#26511=CARTESIAN_POINT('Ctrl Pts',(-0.15240769985127,0.0311311135252802,
2.36703279674523));
#26512=CARTESIAN_POINT('Ctrl Pts',(-0.152162069399693,0.0323103396982948,
2.36694365403721));
#26513=CARTESIAN_POINT('Ctrl Pts',(-0.151774510091642,0.0340683940983547,
2.36681138487069));
#26514=CARTESIAN_POINT('Ctrl Pts',(-0.151642919170991,0.0346494225623182,
2.36676777389633));
#26515=CARTESIAN_POINT('Ctrl Pts',(-0.151425582149855,0.0355840970733577,
2.36669780064557));
#26516=CARTESIAN_POINT('Ctrl Pts',(-0.151341929135608,0.0359382162374241,
2.3666713321065));
#26517=CARTESIAN_POINT('Ctrl Pts',(-0.151194151876046,0.0365541184547088,
2.36662537386571));
#26518=CARTESIAN_POINT('Ctrl Pts',(-0.151130588873795,0.0368160324731053,
2.36660585435635));
#26519=CARTESIAN_POINT('Ctrl Pts',(-0.151001834577968,0.0373406172652141,
2.36656680954848));
#26520=CARTESIAN_POINT('Ctrl Pts',(-0.150936637827199,0.0376032858681038,
2.36654728462139));
#26521=CARTESIAN_POINT('Ctrl Pts',(-0.150809816011158,0.0381085890813387,
2.36650977476321));
#26522=CARTESIAN_POINT('Ctrl Pts',(-0.150748291449749,0.0383512423927614,
2.36649178484732));
#26523=CARTESIAN_POINT('Ctrl Pts',(-0.150580647257716,0.0390057955904033,
2.36644331682817));
#26524=CARTESIAN_POINT('Ctrl Pts',(-0.150473423017106,0.039417412333195,
2.36641290113435));
#26525=CARTESIAN_POINT('Ctrl Pts',(-0.150067489463824,0.0409499295291554,
2.36629987749851));
#26526=CARTESIAN_POINT('Ctrl Pts',(-0.149757923034017,0.0420679548025645,
2.36621786027761));
#26527=CARTESIAN_POINT('Ctrl Pts',(-0.146872923428985,0.0520516949238728,
2.36548852253291));
#26528=CARTESIAN_POINT('Ctrl Pts',(-0.143525042585431,0.0606765989985166,
2.36487954022323));
#26529=CARTESIAN_POINT('Ctrl Pts',(-0.13712921829303,0.0736094174797964,
2.3639285884703));
#26530=CARTESIAN_POINT('Ctrl Pts',(-0.134595612222951,0.0781459401903763,
2.36358716336465));
#26531=CARTESIAN_POINT('Ctrl Pts',(-0.128241386927552,0.0882945737058474,
2.3627897749356));
#26532=CARTESIAN_POINT('Ctrl Pts',(-0.124271295392331,0.093799851503765,
2.36233139260164));
#26533=CARTESIAN_POINT('Ctrl Pts',(-0.1189513152358,0.100244068046163,2.36174923267517));
#26534=CARTESIAN_POINT('Ctrl Pts',(-0.117929122285336,0.101444617278949,
2.36163869328799));
#26535=CARTESIAN_POINT('Ctrl Pts',(-0.116549163734938,0.103016309666412,
2.36149107166756));
#26536=CARTESIAN_POINT('Ctrl Pts',(-0.116207523949633,0.103401542496564,
2.36145465165947));
#26537=CARTESIAN_POINT('Ctrl Pts',(-0.115527842945404,0.104160327443861,
2.36138244022979));
#26538=CARTESIAN_POINT('Ctrl Pts',(-0.11518988700805,0.104533947735041,
2.36134665261909));
#26539=CARTESIAN_POINT('Ctrl Pts',(-0.114534093651337,0.105251904857536,
2.36127742994386));
#26540=CARTESIAN_POINT('Ctrl Pts',(-0.114216503077476,0.105596460644433,
2.36124400550691));
#26541=CARTESIAN_POINT('Ctrl Pts',(-0.11348237371508,0.10638573510344,2.36116696593551));
#26542=CARTESIAN_POINT('Ctrl Pts',(-0.113064771349945,0.106829449299423,
2.36112330582322));
#26543=CARTESIAN_POINT('Ctrl Pts',(-0.111940987178267,0.108009531116785,
2.36100623968675));
#26544=CARTESIAN_POINT('Ctrl Pts',(-0.111230160081044,0.108741412621635,
2.36093263441049));
#26545=CARTESIAN_POINT('Ctrl Pts',(-0.105348184852228,0.114679591069475,
2.36032704882579));
#26546=CARTESIAN_POINT('Ctrl Pts',(-0.0998226113658964,0.119520137638094,
2.35977927590904));
#26547=CARTESIAN_POINT('Ctrl Pts',(-0.0875313188339863,0.128839041187233,
2.35860231343413));
#26548=CARTESIAN_POINT('Ctrl Pts',(-0.0807146275283843,0.133215479215336,
2.35797216234008));
#26549=CARTESIAN_POINT('Ctrl Pts',(-0.0703474097044516,0.138782504958481,
2.35706121510311));
#26550=CARTESIAN_POINT('Ctrl Pts',(-0.0670451391377526,0.140407574908435,
2.3567776620958));
#26551=CARTESIAN_POINT('Ctrl Pts',(-0.0636886247653984,0.141913923120645,
2.35649769913034));
#26552=CARTESIAN_POINT('Ctrl Pts',(-0.0684401807326106,0.139375953783005,
-0.0231689358544845));
#26553=CARTESIAN_POINT('Ctrl Pts',(-0.114796989999545,0.116613226798551,
-0.0194634912834569));
#26554=CARTESIAN_POINT('Ctrl Pts',(-0.182204502677244,0.021600584598116,
-0.0120531424185038));
#26555=CARTESIAN_POINT('Ctrl Pts',(-0.116820455017618,-0.141707599811532,
-0.000937889259625344));
#26556=CARTESIAN_POINT('Ctrl Pts',(0.0556554964189628,-0.174830787340543,
0.0101768236221509));
#26557=CARTESIAN_POINT('Ctrl Pts',(0.177103618810993,-0.0481310406253423,
0.021291536503927));
#26558=CARTESIAN_POINT('Ctrl Pts',(0.136462891783692,0.122747837682665,
0.0324062493857032));
#26559=CARTESIAN_POINT('Ctrl Pts',(-0.0291242938817204,0.181195489255479,
0.0435209622674794));
#26560=CARTESIAN_POINT('Ctrl Pts',(-0.168038372731085,0.0737999881880242,
0.0546356751492556));
#26561=CARTESIAN_POINT('Ctrl Pts',(-0.153127523366183,-0.101172781343492,
0.0657503880310317));
#26562=CARTESIAN_POINT('Ctrl Pts',(0.00196713021444944,-0.18351791358781,
0.076865100912808));
#26563=CARTESIAN_POINT('Ctrl Pts',(0.155259338957376,-0.0978661493738991,
0.087979813794584));
#26564=CARTESIAN_POINT('Ctrl Pts',(0.166420139267564,0.0773797195872082,
0.0990945266763604));
#26565=CARTESIAN_POINT('Ctrl Pts',(0.0252310584054888,0.18178697236432,
0.110209239558137));
#26566=CARTESIAN_POINT('Ctrl Pts',(-0.139055574687841,0.11977790064492,
0.121323952439913));
#26567=CARTESIAN_POINT('Ctrl Pts',(-0.176043812140842,-0.0518822906588397,
0.132438665321689));
#26568=CARTESIAN_POINT('Ctrl Pts',(-0.0518725564901114,-0.176046614996211,
0.143553378203466));
#26569=CARTESIAN_POINT('Ctrl Pts',(0.119785431798764,-0.139049045125415,
0.154668091085242));
#26570=CARTESIAN_POINT('Ctrl Pts',(0.181785783219421,0.0252411197918558,
0.165782803967018));
#26571=CARTESIAN_POINT('Ctrl Pts',(0.077370206262428,0.166424257025588,
0.176897516848794));
#26572=CARTESIAN_POINT('Ctrl Pts',(-0.097873973618601,0.155254209412122,
0.18801222973057));
#26573=CARTESIAN_POINT('Ctrl Pts',(-0.183519360433008,0.00195658265477414,
0.199126942612347));
#26574=CARTESIAN_POINT('Ctrl Pts',(-0.101161822572116,-0.153132195043624,
0.210241655494122));
#26575=CARTESIAN_POINT('Ctrl Pts',(0.0738043738200084,-0.168036002759876,
0.221356368375899));
#26576=CARTESIAN_POINT('Ctrl Pts',(0.181206306397723,-0.0291111363940454,
0.232471081257675));
#26577=CARTESIAN_POINT('Ctrl Pts',(0.122722802371927,0.136463538999617,
0.243585794139451));
#26578=CARTESIAN_POINT('Ctrl Pts',(-0.0481073744247173,0.177112575131921,
0.254700507021226));
#26579=CARTESIAN_POINT('Ctrl Pts',(-0.174897622649273,0.0556237837726867,
0.265815219903004));
#26580=CARTESIAN_POINT('Ctrl Pts',(-0.141577723269147,-0.116785838178545,
0.27692993278478));
#26581=CARTESIAN_POINT('Ctrl Pts',(0.0213495991278188,-0.182283785205111,
0.288044645666556));
#26582=CARTESIAN_POINT('Ctrl Pts',(0.164732416494676,-0.08090991709903,
0.299159358548332));
#26583=CARTESIAN_POINT('Ctrl Pts',(0.157310831167827,0.094532989617669,
0.310274071430108));
#26584=CARTESIAN_POINT('Ctrl Pts',(0.00587893848749207,0.1834356067178,
0.321388784311885));
#26585=CARTESIAN_POINT('Ctrl Pts',(-0.150934832429759,0.104411972918147,
0.332503497193661));
#26586=CARTESIAN_POINT('Ctrl Pts',(-0.16957520837079,-0.0701956724823281,
0.343618210075437));
#26587=CARTESIAN_POINT('Ctrl Pts',(-0.0329778445068435,-0.180542641780405,
0.354732922957213));
#26588=CARTESIAN_POINT('Ctrl Pts',(0.133809109534271,-0.125611726900579,
0.365847635838989));
#26589=CARTESIAN_POINT('Ctrl Pts',(0.17810042326896,0.0443105287795206,
0.376962348720765));
#26590=CARTESIAN_POINT('Ctrl Pts',(0.0593495834231662,0.173668680759705,
0.388077061602541));
#26591=CARTESIAN_POINT('Ctrl Pts',(-0.113732872921998,0.144041720852737,
0.399191774484318));
#26592=CARTESIAN_POINT('Ctrl Pts',(-0.182698493418309,-0.0174483303496573,
0.410306487366094));
#26593=CARTESIAN_POINT('Ctrl Pts',(-0.0844126538894276,-0.162965295669527,
0.42142120024787));
#26594=CARTESIAN_POINT('Ctrl Pts',(0.0911488070387178,-0.159295570260851,
0.432535913129646));
#26595=CARTESIAN_POINT('Ctrl Pts',(0.183268030586852,-0.0097986067442389,
0.443650626011422));
#26596=CARTESIAN_POINT('Ctrl Pts',(0.10761441092159,0.148668497978929,0.454765338893199));
#26597=CARTESIAN_POINT('Ctrl Pts',(-0.0665548943940058,0.171036925140492,
0.465880051774975));
#26598=CARTESIAN_POINT('Ctrl Pts',(-0.179796476382766,0.03682948288604,
0.476994764656751));
#26599=CARTESIAN_POINT('Ctrl Pts',(-0.128443251814735,-0.131093534518557,
0.488109477538528));
#26600=CARTESIAN_POINT('Ctrl Pts',(0.0404934349617796,-0.179006886611403,
0.499224190420303));
#26601=CARTESIAN_POINT('Ctrl Pts',(0.172360379169117,-0.0630482626405321,
0.51033890330208));
#26602=CARTESIAN_POINT('Ctrl Pts',(0.146439897070056,0.11062793623413,0.521453616183855));
#26603=CARTESIAN_POINT('Ctrl Pts',(-0.013539088373249,0.183029715662056,
0.532568329065633));
#26604=CARTESIAN_POINT('Ctrl Pts',(-0.161123706159393,0.0878768174365303,
0.543683041947407));
#26605=CARTESIAN_POINT('Ctrl Pts',(-0.161207517586238,-0.0877229730629007,
0.554797754829185));
#26606=CARTESIAN_POINT('Ctrl Pts',(-0.0137137974260919,-0.183016708224871,
0.56591246771096));
#26607=CARTESIAN_POINT('Ctrl Pts',(0.146334227912434,-0.110767673400607,
0.577027180592736));
#26608=CARTESIAN_POINT('Ctrl Pts',(0.17242048480891,0.0628837033544609,
0.588141893474512));
#26609=CARTESIAN_POINT('Ctrl Pts',(0.0406642916501698,0.178968151116062,
0.599256606356289));
#26610=CARTESIAN_POINT('Ctrl Pts',(-0.128318054949308,0.131216083249494,
0.610371319238065));
#26611=CARTESIAN_POINT('Ctrl Pts',(-0.179831550895884,-0.0366578372478885,
0.621486032119841));
#26612=CARTESIAN_POINT('Ctrl Pts',(-0.0667181312987861,-0.170973315711281,
0.632600745001618));
#26613=CARTESIAN_POINT('Ctrl Pts',(0.10747244696062,-0.148771156053881,
0.643715457883394));
#26614=CARTESIAN_POINT('Ctrl Pts',(0.183277300574292,0.00962365956964026,
0.654830170765169));
#26615=CARTESIAN_POINT('Ctrl Pts',(0.0913008247582609,0.159208489496549,
0.665944883646947));
#26616=CARTESIAN_POINT('Ctrl Pts',(-0.0842570531624994,0.163045799460407,
0.677059596528721));
#26617=CARTESIAN_POINT('Ctrl Pts',(-0.182681754475266,0.01762272144563,
0.688174309410499));
#26618=CARTESIAN_POINT('Ctrl Pts',(-0.113870319439624,-0.143933088899077,
0.699289022292274));
#26619=CARTESIAN_POINT('Ctrl Pts',(0.0591837769528756,-0.173725255144161,
0.710403735174051));
#26620=CARTESIAN_POINT('Ctrl Pts',(0.178058044491996,-0.0444805184434471,
0.721518448055827));
#26621=CARTESIAN_POINT('Ctrl Pts',(0.133928954130774,0.125483939110744,
0.732633160937603));
#26622=CARTESIAN_POINT('Ctrl Pts',(-0.032805488354141,0.180574039283497,
0.743747873819379));
#26623=CARTESIAN_POINT('Ctrl Pts',(-0.169508124219243,0.0703575124132829,
0.754862586701155));
#26624=CARTESIAN_POINT('Ctrl Pts',(-0.151034432511191,-0.104267847035095,
0.765977299582931));
#26625=CARTESIAN_POINT('Ctrl Pts',(0.00570383313473486,-0.183441135018519,
0.777092012464709));
#26626=CARTESIAN_POINT('Ctrl Pts',(0.15722052085916,-0.0946831112188752,
0.788206725346483));
#26627=CARTESIAN_POINT('Ctrl Pts',(0.164809575861347,0.0807526311256457,
0.799321438228262));
#26628=CARTESIAN_POINT('Ctrl Pts',(0.0215235925793826,0.182263322398634,
0.810436151110036));
#26629=CARTESIAN_POINT('Ctrl Pts',(-0.141466178164294,0.116920931252278,
0.821550863991813));
#26630=CARTESIAN_POINT('Ctrl Pts',(-0.174950639917874,-0.0554568059090855,
0.832665576873588));
#26631=CARTESIAN_POINT('Ctrl Pts',(-0.0482764194013637,-0.177066572393253,
0.843780289755366));
#26632=CARTESIAN_POINT('Ctrl Pts',(0.122592482081562,-0.136580624784021,
0.854895002637141));
#26633=CARTESIAN_POINT('Ctrl Pts',(0.181234012486454,0.0289381486514157,
0.866009715518918));
#26634=CARTESIAN_POINT('Ctrl Pts',(0.0739647429309842,0.167965474227488,
0.877124428400693));
#26635=CARTESIAN_POINT('Ctrl Pts',(-0.101015600832807,0.15322869221428,
0.88823914128247));
#26636=CARTESIAN_POINT('Ctrl Pts',(-0.183521144128887,-0.00178140027397675,
0.899353854164246));
#26637=CARTESIAN_POINT('Ctrl Pts',(-0.0980221312474096,-0.155160708670163,
0.910468567046022));
#26638=CARTESIAN_POINT('Ctrl Pts',(0.077211308334424,-0.166498040813092,
0.921583279927798));
#26639=CARTESIAN_POINT('Ctrl Pts',(0.181761603201863,-0.0254146282837278,
0.932697992809575));
#26640=CARTESIAN_POINT('Ctrl Pts',(0.119918114829785,0.138934622988592,
0.943812705691351));
#26641=CARTESIAN_POINT('Ctrl Pts',(-0.0517044933012578,0.176096079177736,
0.954927418573126));
#26642=CARTESIAN_POINT('Ctrl Pts',(-0.175994187883316,0.052050259947511,
0.966042131454904));
#26643=CARTESIAN_POINT('Ctrl Pts',(-0.139169883500762,-0.119645005143115,
0.977156844336678));
#26644=CARTESIAN_POINT('Ctrl Pts',(0.0250575853607977,-0.181811168923138,
0.988271557218456));
#26645=CARTESIAN_POINT('Ctrl Pts',(0.16634607066597,-0.0775381744904013,
0.999386270100231));
#26646=CARTESIAN_POINT('Ctrl Pts',(0.155352932473362,0.0977171945014716,
1.01050098298201));
#26647=CARTESIAN_POINT('Ctrl Pts',(0.00214184661615762,0.183517291344398,
1.02161569586379));
#26648=CARTESIAN_POINT('Ctrl Pts',(-0.153029994182151,0.101316359043948,
1.03273040874556));
#26649=CARTESIAN_POINT('Ctrl Pts',(-0.168110422754029,-0.0736347030331013,
1.04384512162734));
#26650=CARTESIAN_POINT('Ctrl Pts',(-0.0292940505094485,-0.181176826150757,
1.05495983450911));
#26651=CARTESIAN_POINT('Ctrl Pts',(0.136339580192428,-0.122860500577948,
1.06607454739089));
#26652=CARTESIAN_POINT('Ctrl Pts',(0.177161049503372,0.0479285537876487,
1.07718926027266));
#26653=CARTESIAN_POINT('Ctrl Pts',(0.0558003155862178,0.174841380999436,
1.08830397315444));
#26654=CARTESIAN_POINT('Ctrl Pts',(-0.116642855175632,0.141695547092308,
1.09941868603622));
#26655=CARTESIAN_POINT('Ctrl Pts',(-0.182305244855916,-0.0211655717460261,
1.11053339891799));
#26656=CARTESIAN_POINT('Ctrl Pts',(-0.0810761741748326,-0.16465065353798,
1.12164811179977));
#26657=CARTESIAN_POINT('Ctrl Pts',(0.0943741352821535,-0.157406182594767,
1.13276282468155));
#26658=CARTESIAN_POINT('Ctrl Pts',(0.183429578425622,-0.00606411476721494,
1.14387753756332));
#26659=CARTESIAN_POINT('Ctrl Pts',(0.104564289276848,0.150829351047266,
1.1549922504451));
#26660=CARTESIAN_POINT('Ctrl Pts',(-0.0700244495886578,0.169645984889467,
1.16610696332687));
#26661=CARTESIAN_POINT('Ctrl Pts',(-0.180509258465268,0.0331600865142199,
1.17722167620865));
#26662=CARTESIAN_POINT('Ctrl Pts',(-0.125746743943006,-0.133682235607592,
1.18833638909043));
#26663=CARTESIAN_POINT('Ctrl Pts',(0.0441307128230818,-0.178145064245514,
1.1994511019722));
#26664=CARTESIAN_POINT('Ctrl Pts',(0.173608678528705,-0.059524872690566,
1.21056581485398));
#26665=CARTESIAN_POINT('Ctrl Pts',(0.144156461430417,0.113587404042756,
1.22168052773576));
#26666=CARTESIAN_POINT('Ctrl Pts',(-0.017263886303192,0.182716014511652,
1.23279524061753));
#26667=CARTESIAN_POINT('Ctrl Pts',(-0.162879997582005,0.0845771252585338,
1.24390995349931));
#26668=CARTESIAN_POINT('Ctrl Pts',(-0.159387504324502,-0.0909879508205247,
1.25502466638108));
#26669=CARTESIAN_POINT('Ctrl Pts',(-0.00998361185797865,-0.183258045453892,
1.26613937926286));
#26670=CARTESIAN_POINT('Ctrl Pts',(0.148559784872265,-0.107764437770621,
1.27725409214463));
#26671=CARTESIAN_POINT('Ctrl Pts',(0.17110402552832,0.0663821977439403,
1.28836880502641));
#26672=CARTESIAN_POINT('Ctrl Pts',(0.0370109696726974,0.179759205197393,
1.29948351790819));
#26673=CARTESIAN_POINT('Ctrl Pts',(-0.130963803535317,0.128575526026046,
1.31059823078997));
#26674=CARTESIAN_POINT('Ctrl Pts',(-0.179047673748397,-0.0403127058704685,
1.32171294367174));
#26675=CARTESIAN_POINT('Ctrl Pts',(-0.0632222292854659,-0.172296643767334,
1.33282765655352));
#26676=CARTESIAN_POINT('Ctrl Pts',(0.110480047964651,-0.146551501974699,
1.34394236943529));
#26677=CARTESIAN_POINT('Ctrl Pts',(0.183043290184881,0.0133543119480212,
1.35505708231707));
#26678=CARTESIAN_POINT('Ctrl Pts',(0.0880394279455103,0.161034911917692,
1.36617179519885));
#26679=CARTESIAN_POINT('Ctrl Pts',(-0.087560188468778,0.161295992277005,
1.37728650808062));
#26680=CARTESIAN_POINT('Ctrl Pts',(-0.183002770812981,0.0138985468335057,
1.3884012209624));
#26681=CARTESIAN_POINT('Ctrl Pts',(-0.11091534218414,-0.14622233275901,
1.39951593384417));
#26682=CARTESIAN_POINT('Ctrl Pts',(0.0627096118637963,-0.172483878403762,
1.41063064672595));
#26683=CARTESIAN_POINT('Ctrl Pts',(0.178927009091768,-0.0408449402837847,
1.42174535960773));
#26684=CARTESIAN_POINT('Ctrl Pts',(0.131345554185685,0.128185526191403,
1.4328600724895));
#26685=CARTESIAN_POINT('Ctrl Pts',(-0.0364762776077821,0.179868465555226,
1.44397478537128));
#26686=CARTESIAN_POINT('Ctrl Pts',(-0.170905876263246,0.0668906958253804,
1.45508949825306));
#26687=CARTESIAN_POINT('Ctrl Pts',(-0.148879574286476,-0.10732220687998,
1.46620421113483));
#26688=CARTESIAN_POINT('Ctrl Pts',(0.00943863520116258,-0.183286922323583,
1.47731892401661));
#26689=CARTESIAN_POINT('Ctrl Pts',(0.159116239676119,-0.0914615001005527,
1.48843363689838));
#26690=CARTESIAN_POINT('Ctrl Pts',(0.163130774348862,0.0840924145785586,
1.49954834978016));
#26691=CARTESIAN_POINT('Ctrl Pts',(0.0178071307235557,0.18266387115329,
1.51066306266194));
#26692=CARTESIAN_POINT('Ctrl Pts',(-0.143818062830546,0.114015562678875,
1.52177777554371));
#26693=CARTESIAN_POINT('Ctrl Pts',(-0.173784912977673,-0.0590083701745273,
1.53289248842549));
#26694=CARTESIAN_POINT('Ctrl Pts',(-0.0446602463747498,-0.178013050429057,
1.54400720130726));
#26695=CARTESIAN_POINT('Ctrl Pts',(0.125348673138568,-0.134055562628755,
1.55512191418904));
#26696=CARTESIAN_POINT('Ctrl Pts',(0.180607064596649,0.0326231811308033,
1.56623662707082));
#26697=CARTESIAN_POINT('Ctrl Pts',(0.0705285959663834,0.169437011542113,
1.57735133995259));
#26698=CARTESIAN_POINT('Ctrl Pts',(-0.104115323797061,0.151139614528901,
1.58846605283437));
#26699=CARTESIAN_POINT('Ctrl Pts',(-0.183446799597517,-0.00551864537181648,
1.59958076571614));
#26700=CARTESIAN_POINT('Ctrl Pts',(-0.0948417779722103,-0.157124857614515,
1.61069547859792));
#26701=CARTESIAN_POINT('Ctrl Pts',(0.0805862137851994,-0.164891012117331,
1.6218101914797));
#26702=CARTESIAN_POINT('Ctrl Pts',(0.182241501338543,-0.0217075774600834,
1.63292490436147));
#26703=CARTESIAN_POINT('Ctrl Pts',(0.11706368257684,0.141348073743014,1.64403961724325));
#26704=CARTESIAN_POINT('Ctrl Pts',(-0.0552801639970045,0.17500653472878,
1.65515433012502));
#26705=CARTESIAN_POINT('Ctrl Pts',(-0.177017746852174,0.0484551445018068,
1.66626904300681));
#26706=CARTESIAN_POINT('Ctrl Pts',(-0.136704312988724,-0.122454540706307,
1.67738375588858));
#26707=CARTESIAN_POINT('Ctrl Pts',(0.0287551771520279,-0.181263133362156,
1.68849846877036));
#26708=CARTESIAN_POINT('Ctrl Pts',(0.167890720816941,-0.0741342673321824,
1.69961318165213));
#26709=CARTESIAN_POINT('Ctrl Pts',(0.153330589953088,0.100860864134458,
1.71072789453391));
#26710=CARTESIAN_POINT('Ctrl Pts',(-0.00159613374009132,0.183522848949103,
1.72184260741568));
#26711=CARTESIAN_POINT('Ctrl Pts',(-0.155061675715616,0.0981787169073654,
1.73295732029746));
#26712=CARTESIAN_POINT('Ctrl Pts',(-0.166575901223461,-0.0770431882836061,
1.74407203317924));
#26713=CARTESIAN_POINT('Ctrl Pts',(-0.0255981046933993,-0.181735854375017,
1.75518674606101));
#26714=CARTESIAN_POINT('Ctrl Pts',(0.138813494183606,-0.120058309007955,
1.76630145894279));
#26715=CARTESIAN_POINT('Ctrl Pts',(0.176148185424323,0.0515266969738023,
1.77741617182456));
#26716=CARTESIAN_POINT('Ctrl Pts',(0.0522279005468018,0.175941553175437,
1.78853088470634));
#26717=CARTESIAN_POINT('Ctrl Pts',(-0.119504451398526,0.139290594891575,
1.79964559758812));
#26718=CARTESIAN_POINT('Ctrl Pts',(-0.181836372054304,-0.0248740331960887,
1.81076031046989));
#26719=CARTESIAN_POINT('Ctrl Pts',(-0.0777060622737596,-0.166267710681354,
1.82187502335167));
#26720=CARTESIAN_POINT('Ctrl Pts',(0.0975603150513518,-0.155451499370037,
1.83298973623345));
#26721=CARTESIAN_POINT('Ctrl Pts',(0.183515035626797,-0.00232710726154151,
1.84410444911522));
#26722=CARTESIAN_POINT('Ctrl Pts',(0.101470792057078,0.152927636771843,
1.855219161997));
#26723=CARTESIAN_POINT('Ctrl Pts',(-0.0734649570961186,0.168184671739659,
1.86633387487877));
#26724=CARTESIAN_POINT('Ctrl Pts',(-0.18114716132335,0.0294769346066355,
1.87744858776055));
#26725=CARTESIAN_POINT('Ctrl Pts',(-0.122998073546538,-0.136215482354805,
1.88856330064232));
#26726=CARTESIAN_POINT('Ctrl Pts',(0.0477496842907016,-0.177209343375145,
1.8996780135241));
#26727=CARTESIAN_POINT('Ctrl Pts',(0.174784961176733,-0.055976790509635,
1.91079272640588));
#26728=CARTESIAN_POINT('Ctrl Pts',(0.141813226508904,0.116499753289206,
1.92190743928765));
#26729=CARTESIAN_POINT('Ctrl Pts',(-0.0209815227920695,0.182326518725712,
1.93302215216943));
#26730=CARTESIAN_POINT('Ctrl Pts',(-0.164568722786704,0.0812423486222812,
1.94413686505121));
#26731=CARTESIAN_POINT('Ctrl Pts',(-0.157501373608142,-0.0942151847679616,
1.95525157793298));
#26732=CARTESIAN_POINT('Ctrl Pts',(-0.00624928486731097,-0.183423363200978,
1.96636629081476));
#26733=CARTESIAN_POINT('Ctrl Pts',(0.150723715954467,-0.104716499073386,
1.97748100369653));
#26734=CARTESIAN_POINT('Ctrl Pts',(0.169716588521531,0.0698531553326882,
1.98859571657831));
#26735=CARTESIAN_POINT('Ctrl Pts',(0.0333422947280978,0.180475691192936,
1.99971042946009));
#26736=CARTESIAN_POINT('Ctrl Pts',(-0.133555225445056,0.125881632836647,
2.01082514234186));
#26737=CARTESIAN_POINT('Ctrl Pts',(-0.178189523674224,-0.0439508518929735,
2.02193985522364));
#26738=CARTESIAN_POINT('Ctrl Pts',(-0.0597001012958023,-0.173548499372694,
2.03305456810542));
#26739=CARTESIAN_POINT('Ctrl Pts',(0.113441819405896,-0.144271055098171,
2.04416928098719));
#26740=CARTESIAN_POINT('Ctrl Pts',(0.182733349399699,0.0170794246634578,
2.05528399386897));
#26741=CARTESIAN_POINT('Ctrl Pts',(0.0847415104331493,0.162794533502435,
2.06639870675075));
#26742=CARTESIAN_POINT('Ctrl Pts',(-0.0908270018729541,0.159479275957466,
2.07751341963252));
#26743=CARTESIAN_POINT('Ctrl Pts',(-0.183247873568771,0.0101686067947032,
2.0886281325143));
#26744=CARTESIAN_POINT('Ctrl Pts',(-0.107914354784435,-0.148450920362924,
2.09974284539607));
#26745=CARTESIAN_POINT('Ctrl Pts',(0.0662094334203013,-0.17117095155347,
2.11085755827785));
#26746=CARTESIAN_POINT('Ctrl Pts',(0.179721750863506,-0.0371924187228543,
2.12197227115963));
#26747=CARTESIAN_POINT('Ctrl Pts',(0.128707669121284,0.130833939051324,
2.1330869840414));
#26748=CARTESIAN_POINT('Ctrl Pts',(-0.0401319355356154,0.179088278484728,
2.14420169692318));
#26749=CARTESIAN_POINT('Ctrl Pts',(-0.172232733083604,0.063396131372761,
2.15531640980495));
#26750=CARTESIAN_POINT('Ctrl Pts',(-0.146662956946516,-0.110332046861714,
2.16643112268673));
#26751=CARTESIAN_POINT('Ctrl Pts',(0.0131695208063343,-0.1830566786303,
2.17754583556851));
#26752=CARTESIAN_POINT('Ctrl Pts',(0.160945955671087,-0.0882019478537668,
2.18866054845028));
#26753=CARTESIAN_POINT('Ctrl Pts',(0.161384298584102,0.0873973129685732,
2.19977526133206));
#26754=CARTESIAN_POINT('Ctrl Pts',(0.0140832896991538,0.182988650085996,
2.21088997421383));
#26755=CARTESIAN_POINT('Ctrl Pts',(-0.146110303090852,0.111062891877556,
2.22200468709561));
#26756=CARTESIAN_POINT('Ctrl Pts',(-0.172547068633587,-0.0625354449444508,
2.23311939997739));
#26757=CARTESIAN_POINT('Ctrl Pts',(-0.0410255997730136,-0.178885706640729,
2.24423411285916));
#26758=CARTESIAN_POINT('Ctrl Pts',(0.128052966639604,-0.131474849570047,
2.25534882574094));
#26759=CARTESIAN_POINT('Ctrl Pts',(0.179905006972722,0.0362946014689825,
2.26646353862272));
#26760=CARTESIAN_POINT('Ctrl Pts',(0.0670635535236872,0.17083841355505,
2.27757825150449));
#26761=CARTESIAN_POINT('Ctrl Pts',(-0.107172544846188,0.148987553701467,
2.28869296438627));
#26762=CARTESIAN_POINT('Ctrl Pts',(-0.183295049527548,-0.00925305504128419,
2.29980767726805));
#26763=CARTESIAN_POINT('Ctrl Pts',(-0.0916245701370072,-0.15902486674809,
2.31092239014982));
#26764=CARTESIAN_POINT('Ctrl Pts',(0.0839324233649617,-0.163213606279465,
2.3220371030316));
#26765=CARTESIAN_POINT('Ctrl Pts',(0.182636797030692,-0.0179952824654467,
2.33315181591337));
#26766=CARTESIAN_POINT('Ctrl Pts',(0.114177823608791,0.143710045180207,
2.34426652879515));
#26767=CARTESIAN_POINT('Ctrl Pts',(-0.0588655274452063,0.173830775601519,
2.35538124167692));
#26768=CARTESIAN_POINT('Ctrl Pts',(-0.177905565768648,0.0448658907444426,
2.3664959545587));
#26769=CARTESIAN_POINT('Ctrl Pts',(-0.134302673977538,-0.125263140298141,
2.37761066744048));
#26770=CARTESIAN_POINT('Ctrl Pts',(0.0327061607400811,-0.180546868845806,
2.38872656798691));
#26771=CARTESIAN_POINT('Ctrl Pts',(0.123427388818086,-0.107442269004469,
2.39613756423943));
#26772=CARTESIAN_POINT('Ctrl Pts',(0.143308829964112,-0.0597686701569069,
2.39984365619801));
#26773=CARTESIAN_POINT('Ctrl Pts',(-0.0743730976566809,0.151458124609491,
-0.0153976563500216));
#26774=CARTESIAN_POINT('Ctrl Pts',(-0.124748468758219,0.126722150817118,
-0.0116922117789939));
#26775=CARTESIAN_POINT('Ctrl Pts',(-0.197999378815845,0.02347308803922,
-0.00428186291404084));
#26776=CARTESIAN_POINT('Ctrl Pts',(-0.126947343158939,-0.153991895501451,
0.00683339024483763));
#26777=CARTESIAN_POINT('Ctrl Pts',(0.0604801393858151,-0.189986453587436,
0.0179481031266138));
#26778=CARTESIAN_POINT('Ctrl Pts',(0.19245631142679,-0.0523034063678348,
0.0290628160083901));
#26779=CARTESIAN_POINT('Ctrl Pts',(0.148292536175391,0.133388556567168,
0.0401775288901662));
#26780=CARTESIAN_POINT('Ctrl Pts',(-0.0316490098340019,0.196902896413978,
0.0512922417719424));
#26781=CARTESIAN_POINT('Ctrl Pts',(-0.182605220667447,0.0801975341066568,
0.0624069546537186));
#26782=CARTESIAN_POINT('Ctrl Pts',(-0.166401785140401,-0.109943209771101,
0.0735216675354948));
#26783=CARTESIAN_POINT('Ctrl Pts',(0.00213765606661008,-0.199426646202769,
0.0846363804172708));
#26784=CARTESIAN_POINT('Ctrl Pts',(0.168718402768423,-0.106349933719559,
0.0957510932990472));
#26785=CARTESIAN_POINT('Ctrl Pts',(0.180846706383503,0.0840875839295365,
0.106865806180823));
#26786=CARTESIAN_POINT('Ctrl Pts',(0.0274182790092828,0.197545653790497,
0.1179805190626));
#26787=CARTESIAN_POINT('Ctrl Pts',(-0.151109972610529,0.130161162732459,
0.129095231944376));
#26788=CARTESIAN_POINT('Ctrl Pts',(-0.191304632630316,-0.056379843368586,
0.140209944826152));
#26789=CARTESIAN_POINT('Ctrl Pts',(-0.0563692653678523,-0.191307678458572,
0.151324657707928));
#26790=CARTESIAN_POINT('Ctrl Pts',(0.130169346744173,-0.151102877015818,
0.162439370589704));
#26791=CARTESIAN_POINT('Ctrl Pts',(0.197544361561446,0.0274292125933766,
0.17355408347148));
#26792=CARTESIAN_POINT('Ctrl Pts',(0.0840772459171892,0.180851181100206,
0.184668796353257));
#26793=CARTESIAN_POINT('Ctrl Pts',(-0.106358436229481,0.168712828555055,
0.195783509235032));
#26794=CARTESIAN_POINT('Ctrl Pts',(-0.199428218471545,0.00212619416399677,
0.206898222116809));
#26795=CARTESIAN_POINT('Ctrl Pts',(-0.109931301009821,-0.166406861794485,
0.218012934998585));
#26796=CARTESIAN_POINT('Ctrl Pts',(0.0802022999186832,-0.182602645249051,
0.229127647880362));
#26797=CARTESIAN_POINT('Ctrl Pts',(0.196914651268626,-0.0316347117549218,
0.240242360762137));
#26798=CARTESIAN_POINT('Ctrl Pts',(0.133361351004721,0.148293239496936,
0.251357073643914));
#26799=CARTESIAN_POINT('Ctrl Pts',(-0.0522776886004238,0.192466044149931,
0.26247178652569));
#26800=CARTESIAN_POINT('Ctrl Pts',(-0.190059082690547,0.060445677645449,
0.273586499407466));
#26801=CARTESIAN_POINT('Ctrl Pts',(-0.153850760269675,-0.126909725468206,
0.284701212289243));
#26802=CARTESIAN_POINT('Ctrl Pts',(0.023200345233862,-0.19808553415799,
0.295815925171018));
#26803=CARTESIAN_POINT('Ctrl Pts',(0.179012678926803,-0.0879238058898391,
0.306930638052795));
#26804=CARTESIAN_POINT('Ctrl Pts',(0.170947733972349,0.102727830250495,
0.318045350934571));
#26805=CARTESIAN_POINT('Ctrl Pts',(0.00638856971982268,0.199337204345436,
0.329160063816347));
#26806=CARTESIAN_POINT('Ctrl Pts',(-0.16401901502788,0.113463199179825,
0.340274776698123));
#26807=CARTESIAN_POINT('Ctrl Pts',(-0.184275280943301,-0.0762807688220648,
0.351389489579899));
#26808=CARTESIAN_POINT('Ctrl Pts',(-0.0358366156219873,-0.196193455139879,
0.362504202461675));
#26809=CARTESIAN_POINT('Ctrl Pts',(0.145408703837682,-0.136500709548084,
0.373618915343452));
#26810=CARTESIAN_POINT('Ctrl Pts',(0.193539526498743,0.048151703412559,
0.384733628225228));
#26811=CARTESIAN_POINT('Ctrl Pts',(0.0644944580298395,0.188723606743685,
0.395848341107004));
#26812=CARTESIAN_POINT('Ctrl Pts',(-0.123592105895363,0.156528355959058,
0.40696305398878));
#26813=CARTESIAN_POINT('Ctrl Pts',(-0.19853619244248,-0.0189608847193331,
0.418077766870556));
#26814=CARTESIAN_POINT('Ctrl Pts',(-0.0917301866239241,-0.177092370589023,
0.429192479752332));
#26815=CARTESIAN_POINT('Ctrl Pts',(0.099050280911231,-0.173104525389443,
0.440307192634109));
#26816=CARTESIAN_POINT('Ctrl Pts',(0.199155101437193,-0.0106480247200912,
0.451421905515884));
#26817=CARTESIAN_POINT('Ctrl Pts',(0.116943248937439,0.16155621741937,0.462536618397661));
#26818=CARTESIAN_POINT('Ctrl Pts',(-0.0723243803173798,0.1858637104725,
0.473651331279438));
#26819=CARTESIAN_POINT('Ctrl Pts',(-0.195382606433862,0.0400221433959911,
0.484766044161213));
#26820=CARTESIAN_POINT('Ctrl Pts',(-0.139577692640525,-0.142457722065341,
0.49588075704299));
#26821=CARTESIAN_POINT('Ctrl Pts',(0.0440037147861017,-0.194524568998165,
0.506995469924765));
#26822=CARTESIAN_POINT('Ctrl Pts',(0.18730189159157,-0.0685137669751007,
0.518110182806543));
#26823=CARTESIAN_POINT('Ctrl Pts',(0.159134424384059,0.120218009611093,
0.529224895688318));
#26824=CARTESIAN_POINT('Ctrl Pts',(-0.0147127598289137,0.198896127556861,
0.540339608570095));
#26825=CARTESIAN_POINT('Ctrl Pts',(-0.175091138052601,0.0954946502917501,
0.55145432145187));
#26826=CARTESIAN_POINT('Ctrl Pts',(-0.17518221489323,-0.0953274695143051,
0.562569034333647));
#26827=CARTESIAN_POINT('Ctrl Pts',(-0.0149026139951197,-0.198881992535802,
0.573683747215423));
#26828=CARTESIAN_POINT('Ctrl Pts',(0.15901959501782,-0.12036986026106,0.584798460097199));
#26829=CARTESIAN_POINT('Ctrl Pts',(0.1873672076467,0.0683349424348715,0.595913172978975));
#26830=CARTESIAN_POINT('Ctrl Pts',(0.0441893826355188,0.194482475614617,
0.607027885860752));
#26831=CARTESIAN_POINT('Ctrl Pts',(-0.139441642755814,0.142590894255063,
0.618142598742528));
#26832=CARTESIAN_POINT('Ctrl Pts',(-0.195420721473322,-0.0398356182046292,
0.629257311624304));
#26833=CARTESIAN_POINT('Ctrl Pts',(-0.0725017678422208,-0.18579458689276,
0.64037202450608));
#26834=CARTESIAN_POINT('Ctrl Pts',(0.116788978457446,-0.161667774679324,
0.651486737387856));
#26835=CARTESIAN_POINT('Ctrl Pts',(0.199165175017855,0.0104579117899193,
0.662601450269632));
#26836=CARTESIAN_POINT('Ctrl Pts',(0.0992154766862795,0.173009895800249,
0.673716163151409));
#26837=CARTESIAN_POINT('Ctrl Pts',(-0.0915610972390791,0.177179853062572,
0.684830876033184));
#26838=CARTESIAN_POINT('Ctrl Pts',(-0.198518002440172,0.0191503933657419,
0.695945588914962));
#26839=CARTESIAN_POINT('Ctrl Pts',(-0.123741467325564,-0.156410306959021,
0.707060301796736));
#26840=CARTESIAN_POINT('Ctrl Pts',(0.0643142781899493,-0.18878508542733,
0.718175014678514));
#26841=CARTESIAN_POINT('Ctrl Pts',(0.193493474006132,-0.0483364290772185,
0.729289727560289));
#26842=CARTESIAN_POINT('Ctrl Pts',(0.145538937477972,0.136361844137873,
0.740404440442067));
#26843=CARTESIAN_POINT('Ctrl Pts',(-0.0356493183232534,0.196227574418036,
0.75151915332384));
#26844=CARTESIAN_POINT('Ctrl Pts',(-0.184202381425786,0.0764566382727335,
0.76263386620562));
#26845=CARTESIAN_POINT('Ctrl Pts',(-0.164127249204111,-0.113306579365854,
0.773748579087393));
#26846=CARTESIAN_POINT('Ctrl Pts',(0.00619828489940304,-0.199343211881429,
0.784863291969171));
#26847=CARTESIAN_POINT('Ctrl Pts',(0.170849594877248,-0.102890965537207,
0.795978004850945));
#26848=CARTESIAN_POINT('Ctrl Pts',(0.17909652705594,0.0877528851685207,
0.807092717732724));
#26849=CARTESIAN_POINT('Ctrl Pts',(0.0233894217650114,0.198063297479358,
0.818207430614498));
#26850=CARTESIAN_POINT('Ctrl Pts',(-0.153729545584279,0.127056529440048,
0.829322143496276));
#26851=CARTESIAN_POINT('Ctrl Pts',(-0.1901166959004,-0.060264224866941,
0.84043685637805));
#26852=CARTESIAN_POINT('Ctrl Pts',(-0.0524613876851037,-0.192416053542971,
0.851551569259829));
#26853=CARTESIAN_POINT('Ctrl Pts',(0.133219733557517,-0.148420475170249,
0.862666282141603));
#26854=CARTESIAN_POINT('Ctrl Pts',(0.196944759132467,0.0314467281152284,
0.87378099502338));
#26855=CARTESIAN_POINT('Ctrl Pts',(0.0803765710474773,0.182526002765492,
0.884895707905156));
#26856=CARTESIAN_POINT('Ctrl Pts',(-0.109772403654785,0.166511724075962,
0.896010420786932));
#26857=CARTESIAN_POINT('Ctrl Pts',(-0.199430156791788,-0.00193582563815892,
0.907125133668708));
#26858=CARTESIAN_POINT('Ctrl Pts',(-0.106519437291686,-0.168611222455568,
0.918239846550485));
#26859=CARTESIAN_POINT('Ctrl Pts',(0.0839045735047286,-0.180931361029226,
0.92935455943226));
#26860=CARTESIAN_POINT('Ctrl Pts',(0.197518085435524,-0.0276177621248288,
0.940469272314037));
#26861=CARTESIAN_POINT('Ctrl Pts',(0.130313531752415,0.150978535895375,
0.951583985195813));
#26862=CARTESIAN_POINT('Ctrl Pts',(-0.05618663317982,0.19136143057266,0.962698698077589));
#26863=CARTESIAN_POINT('Ctrl Pts',(-0.191250706563621,0.0565623735164518,
0.973813410959366));
#26864=CARTESIAN_POINT('Ctrl Pts',(-0.151234190583289,-0.130016746834843,
0.984928123841142));
#26865=CARTESIAN_POINT('Ctrl Pts',(0.0272297679978432,-0.197571947891603,
0.996042836722918));
#26866=CARTESIAN_POINT('Ctrl Pts',(0.180766216950535,-0.0842597749124158,
1.0071575496047));
#26867=CARTESIAN_POINT('Ctrl Pts',(0.168820109684298,0.106188066302576,
1.01827226248647));
#26868=CARTESIAN_POINT('Ctrl Pts',(0.00232751821873696,0.199425970018551,
1.02938697536825));
#26869=CARTESIAN_POINT('Ctrl Pts',(-0.166295801382756,0.110099233881827,
1.04050168825003));
#26870=CARTESIAN_POINT('Ctrl Pts',(-0.18268351653597,-0.0800179207737264,
1.0516164011318));
#26871=CARTESIAN_POINT('Ctrl Pts',(-0.0318334822611076,-0.196882615448979,
1.06273111401358));
#26872=CARTESIAN_POINT('Ctrl Pts',(0.148158534994787,-0.133510985941596,
1.07384582689535));
#26873=CARTESIAN_POINT('Ctrl Pts',(0.192518720649659,0.0520833664264994,
1.08496053977713));
#26874=CARTESIAN_POINT('Ctrl Pts',(0.0606375125831525,0.189997965585494,
1.09607525265891));
#26875=CARTESIAN_POINT('Ctrl Pts',(-0.126754347607934,0.153978797960581,
1.10718996554068));
#26876=CARTESIAN_POINT('Ctrl Pts',(-0.198108854095019,-0.0230003649548643,
1.11830467842246));
#26877=CARTESIAN_POINT('Ctrl Pts',(-0.0881044753971729,-0.178923828133336,
1.12941939130423));
#26878=CARTESIAN_POINT('Ctrl Pts',(0.102555205209445,-0.171051351188312,
1.14053410418601));
#26879=CARTESIAN_POINT('Ctrl Pts',(0.199330653474907,-0.00658979849198673,
1.15164881706779));
#26880=CARTESIAN_POINT('Ctrl Pts',(0.11362871948236,0.163904389714545,1.16276352994956));
#26881=CARTESIAN_POINT('Ctrl Pts',(-0.0760947030218921,0.184352192910496,
1.17387824283134));
#26882=CARTESIAN_POINT('Ctrl Pts',(-0.19615717790434,0.0360346557566957,
1.18499295571311));
#26883=CARTESIAN_POINT('Ctrl Pts',(-0.136647430897652,-0.14527083151125,
1.19610766859489));
#26884=CARTESIAN_POINT('Ctrl Pts',(0.0479562996373891,-0.193588037295664,
1.20722238147667));
#26885=CARTESIAN_POINT('Ctrl Pts',(0.188658403061609,-0.0646849427080351,
1.21833709435844));
#26886=CARTESIAN_POINT('Ctrl Pts',(0.156653043125246,0.123434026664039,
1.22945180724022));
#26887=CARTESIAN_POINT('Ctrl Pts',(-0.0187604516559904,0.198555232397844,
1.240566520122));
#26888=CARTESIAN_POINT('Ctrl Pts',(-0.176999678212625,0.0919089156258833,
1.25168123300377));
#26889=CARTESIAN_POINT('Ctrl Pts',(-0.173204428999001,-0.0988754804490419,
1.26279594588555));
#26890=CARTESIAN_POINT('Ctrl Pts',(-0.0108490674882994,-0.199144250716743,
1.27391065876733));
#26891=CARTESIAN_POINT('Ctrl Pts',(0.161438080231363,-0.11710628125814,
1.2850253716491));
#26892=CARTESIAN_POINT('Ctrl Pts',(0.185936627633784,0.0721367130043656,
1.29614008453088));
#26893=CARTESIAN_POINT('Ctrl Pts',(0.0402193628416877,0.195342104297838,
1.30725479741266));
#26894=CARTESIAN_POINT('Ctrl Pts',(-0.142316745010891,0.139721433389453,
1.31836951029443));
#26895=CARTESIAN_POINT('Ctrl Pts',(-0.194568891875317,-0.0438073187185638,
1.32948422317621));
#26896=CARTESIAN_POINT('Ctrl Pts',(-0.0687028143758259,-0.187232631118989,
1.34059893605798));
#26897=CARTESIAN_POINT('Ctrl Pts',(0.120057301258331,-0.159255704053152,
1.35171364893976));
#26898=CARTESIAN_POINT('Ctrl Pts',(0.198910878822871,0.0145119655736819,
1.36282836182153));
#26899=CARTESIAN_POINT('Ctrl Pts',(0.0956713571200331,0.174994646448712,
1.37394307470331));
#26900=CARTESIAN_POINT('Ctrl Pts',(-0.0951505735098516,0.175278359245073,
1.38505778758509));
#26901=CARTESIAN_POINT('Ctrl Pts',(-0.198866846922735,0.0151033788904271,
1.39617250046686));
#26902=CARTESIAN_POINT('Ctrl Pts',(-0.12053033010116,-0.158897999938967,
1.40728721334864));
#26903=CARTESIAN_POINT('Ctrl Pts',(0.0681457593658351,-0.187436096681916,
1.41840192623042));
#26904=CARTESIAN_POINT('Ctrl Pts',(0.194437767085829,-0.0443856912706738,
1.42951663911219));
#26905=CARTESIAN_POINT('Ctrl Pts',(0.142731588719601,0.139297625394252,
1.44063135199397));
#26906=CARTESIAN_POINT('Ctrl Pts',(-0.0396383195899908,0.195460836176919,
1.45174606487574));
#26907=CARTESIAN_POINT('Ctrl Pts',(-0.185721301278944,0.0726892915782933,
1.46286077775752));
#26908=CARTESIAN_POINT('Ctrl Pts',(-0.161785591431329,-0.116625714420593,
1.4739754906393));
#26909=CARTESIAN_POINT('Ctrl Pts',(0.0102568480978256,-0.199175630853768,
1.48509020352107));
#26910=CARTESIAN_POINT('Ctrl Pts',(0.172909649061707,-0.0993900805928641,
1.49620491640285));
#26911=CARTESIAN_POINT('Ctrl Pts',(0.177272194222541,0.0913821865268278,
1.50731962928462));
#26912=CARTESIAN_POINT('Ctrl Pts',(0.0193507886465428,0.198498568855433,
1.5184343421664));
#26913=CARTESIAN_POINT('Ctrl Pts',(-0.156285309553457,0.123899301356701,
1.52954905504818));
#26914=CARTESIAN_POINT('Ctrl Pts',(-0.188849914856919,-0.0641236658140599,
1.54066376792995));
#26915=CARTESIAN_POINT('Ctrl Pts',(-0.0485317371965617,-0.193444579514605,
1.55177848081173));
#26916=CARTESIAN_POINT('Ctrl Pts',(0.136214852279427,-0.145676521366322,
1.56289319369351));
#26917=CARTESIAN_POINT('Ctrl Pts',(0.196263462617248,0.0354512073191666,
1.57400790657528));
#26918=CARTESIAN_POINT('Ctrl Pts',(0.0766425526532328,0.184125104159359,
1.58512261945706));
#26919=CARTESIAN_POINT('Ctrl Pts',(-0.113140834250107,0.164241549201438,
1.59623733233883));
#26920=CARTESIAN_POINT('Ctrl Pts',(-0.199349367509344,-0.00599704364859195,
1.60735204522061));
#26921=CARTESIAN_POINT('Ctrl Pts',(-0.103063386735022,-0.170745638812843,
1.61846675810238));
#26922=CARTESIAN_POINT('Ctrl Pts',(0.0875720415035815,-0.179185022827784,
1.62958147098416));
#26923=CARTESIAN_POINT('Ctrl Pts',(0.198039584803329,-0.0235893558585985,
1.64069618386594));
#26924=CARTESIAN_POINT('Ctrl Pts',(0.127211655538323,0.153601202970868,
1.65181089674772));
#26925=CARTESIAN_POINT('Ctrl Pts',(-0.0600722702865052,0.190177436099879,
1.66292560962949));
#26926=CARTESIAN_POINT('Ctrl Pts',(-0.192362995431554,0.052655606040559,
1.67404032251127));
#26927=CARTESIAN_POINT('Ctrl Pts',(-0.148554885612024,-0.133069834371645,
1.68515503539304));
#26928=CARTESIAN_POINT('Ctrl Pts',(0.0312478952505764,-0.196976404427808,
1.69626974827482));
#26929=CARTESIAN_POINT('Ctrl Pts',(0.182444769159104,-0.0805607911168946,
1.7073844611566));
#26930=CARTESIAN_POINT('Ctrl Pts',(0.166622455088041,0.1096042531991,1.71849917403837));
#26931=CARTESIAN_POINT('Ctrl Pts',(-0.00173449878791257,0.199432009398825,
1.72961388692015));
#26932=CARTESIAN_POINT('Ctrl Pts',(-0.168503604569103,0.106689596991075,
1.74072859980192));
#26933=CARTESIAN_POINT('Ctrl Pts',(-0.181015970973881,-0.0837218795254947,
1.7518433126837));
#26934=CARTESIAN_POINT('Ctrl Pts',(-0.0278171436692394,-0.197490104503956,
1.76295802556548));
#26935=CARTESIAN_POINT('Ctrl Pts',(0.150846906721609,-0.130465879031342,
1.77407273844725));
#26936=CARTESIAN_POINT('Ctrl Pts',(0.191418053786163,0.0559934241104793,
1.78518745132903));
#26937=CARTESIAN_POINT('Ctrl Pts',(0.0567554133579225,0.191193509077766,
1.79630216421081));
#26938=CARTESIAN_POINT('Ctrl Pts',(-0.129864008819537,0.151365366158238,
1.80741687709258));
#26939=CARTESIAN_POINT('Ctrl Pts',(-0.197599335822427,-0.0270303041313708,
1.81853158997436));
#26940=CARTESIAN_POINT('Ctrl Pts',(-0.084442216489475,-0.180681064124725,
1.82964630285613));
#26941=CARTESIAN_POINT('Ctrl Pts',(0.106017587345052,-0.168927221111439,
1.84076101573791));
#26942=CARTESIAN_POINT('Ctrl Pts',(0.199423518758144,-0.0025288386700214,
1.85187572861969));
#26943=CARTESIAN_POINT('Ctrl Pts',(0.110267054326543,0.166184570851345,
1.86299044150146));
#26944=CARTESIAN_POINT('Ctrl Pts',(-0.079833459964113,0.182764201990043,
1.87410515438324));
#26945=CARTESIAN_POINT('Ctrl Pts',(-0.19685037904805,0.0320322201468692,
1.88521986726501));
#26946=CARTESIAN_POINT('Ctrl Pts',(-0.133660484784501,-0.148023679409987,
1.89633458014679));
#26947=CARTESIAN_POINT('Ctrl Pts',(0.0518889911571499,-0.19257120100262,
1.90744929302857));
#26948=CARTESIAN_POINT('Ctrl Pts',(0.189936654862191,-0.0608292856990732,
1.91856400591034));
#26949=CARTESIAN_POINT('Ctrl Pts',(0.154106678726662,0.12659884055842,1.92967871879212));
#26950=CARTESIAN_POINT('Ctrl Pts',(-0.0228003612336629,0.198131972146125,
1.9407934316739));
#26951=CARTESIAN_POINT('Ctrl Pts',(-0.178834794999575,0.0882850551132964,
1.95190814455567));
#26952=CARTESIAN_POINT('Ctrl Pts',(-0.171154794084838,-0.102382475652217,
1.96302285743745));
#26953=CARTESIAN_POINT('Ctrl Pts',(-0.00679102054882718,-0.19932389946718,
1.97413757031922));
#26954=CARTESIAN_POINT('Ctrl Pts',(0.163789597366124,-0.11379412398511,
1.985252283201));
#26955=CARTESIAN_POINT('Ctrl Pts',(0.184428917003948,0.0759085596731913,
1.99636699608278));
#26956=CARTESIAN_POINT('Ctrl Pts',(0.0362326591684271,0.196120700764793,
2.00748170896455));
#26957=CARTESIAN_POINT('Ctrl Pts',(-0.145132811138998,0.136794012989519,
2.01859642184633));
#26958=CARTESIAN_POINT('Ctrl Pts',(-0.19363635080679,-0.0477608469898892,
2.02971113472811));
#26959=CARTESIAN_POINT('Ctrl Pts',(-0.0648753614654078,-0.188593007117311,
2.04082584760988));
#26960=CARTESIAN_POINT('Ctrl Pts',(0.123275821640341,-0.156777570646236,
2.05194056049166));
#26961=CARTESIAN_POINT('Ctrl Pts',(0.198574070006218,0.0185599994742601,
2.06305527337343));
#26962=CARTESIAN_POINT('Ctrl Pts',(0.0920875509613561,0.176906805454723,
2.07416998625521));
#26963=CARTESIAN_POINT('Ctrl Pts',(-0.0987005792189857,0.173304156097139,
2.08528469913698));
#26964=CARTESIAN_POINT('Ctrl Pts',(-0.199133197055029,0.0110500991972711,
2.09639941201877));
#26965=CARTESIAN_POINT('Ctrl Pts',(-0.117269194222271,-0.161319778515938,
2.10751412490054));
#26966=CARTESIAN_POINT('Ctrl Pts',(0.0719489721513163,-0.186009355317303,
2.11862883778232));
#26967=CARTESIAN_POINT('Ctrl Pts',(0.195301403136589,-0.0404165412795961,
2.12974355066409));
#26968=CARTESIAN_POINT('Ctrl Pts',(0.139865031656166,0.142175622882825,
2.14085826354587));
#26969=CARTESIAN_POINT('Ctrl Pts',(-0.0436108778321787,0.194613016539923,
2.15197297642764));
#26970=CARTESIAN_POINT('Ctrl Pts',(-0.187163180169686,0.068891791622564,
2.16308768930942));
#26971=CARTESIAN_POINT('Ctrl Pts',(-0.159376820792098,-0.119896470290846,
2.1742024021912));
#26972=CARTESIAN_POINT('Ctrl Pts',(0.0143111553262565,-0.198925427880866,
2.18531711507297));
#26973=CARTESIAN_POINT('Ctrl Pts',(0.174897978796096,-0.0958479654936306,
2.19643182795475));
#26974=CARTESIAN_POINT('Ctrl Pts',(0.175374320616466,0.0949735787188828,
2.20754654083652));
#26975=CARTESIAN_POINT('Ctrl Pts',(0.0153041366768783,0.198851502103424,
2.2186612537183));
#26976=CARTESIAN_POINT('Ctrl Pts',(-0.158776258684615,0.120690670527502,
2.22977596660007));
#26977=CARTESIAN_POINT('Ctrl Pts',(-0.187504764722873,-0.0679564943293847,
2.24089067948186));
#26978=CARTESIAN_POINT('Ctrl Pts',(-0.0445820117024905,-0.19439288422328,
2.25200539236363));
#26979=CARTESIAN_POINT('Ctrl Pts',(0.139153574569345,-0.142872092414138,
2.26312010524541));
#26980=CARTESIAN_POINT('Ctrl Pts',(0.195500545283218,0.0394408943776638,
2.27423481812718));
#26981=CARTESIAN_POINT('Ctrl Pts',(0.0728771339004392,0.185647990388598,
2.28534953100895));
#26982=CARTESIAN_POINT('Ctrl Pts',(-0.116463078540096,0.161902931325674,
2.29646424389074));
#26983=CARTESIAN_POINT('Ctrl Pts',(-0.199184462585767,-0.0100551804340931,
2.30757895677251));
#26984=CARTESIAN_POINT('Ctrl Pts',(-0.0995672867839686,-0.172810355231288,
2.31869366965429));
#26985=CARTESIAN_POINT('Ctrl Pts',(0.0912083260544317,-0.177362206656727,
2.32980838253606));
#26986=CARTESIAN_POINT('Ctrl Pts',(0.198469147741369,-0.0195552508166324,
2.34092309541784));
#26987=CARTESIAN_POINT('Ctrl Pts',(0.124075628301739,0.156167928109233,
2.35203780829962));
#26988=CARTESIAN_POINT('Ctrl Pts',(-0.0639684403873645,0.188899753202837,
2.36315252118139));
#26989=CARTESIAN_POINT('Ctrl Pts',(-0.193327777263944,0.048755208388864,
2.37426723406317));
#26990=CARTESIAN_POINT('Ctrl Pts',(-0.145945054211769,-0.136121904799952,
2.38538194694494));
#26991=CARTESIAN_POINT('Ctrl Pts',(0.035541380233941,-0.196198048639552,
2.39649784749138));
#26992=CARTESIAN_POINT('Ctrl Pts',(0.134127016378589,-0.116756184445853,
2.40390884374389));
#26993=CARTESIAN_POINT('Ctrl Pts',(0.155731932497757,-0.0649498743984335,
2.40761493570248));
#26994=CARTESIAN_POINT('Ctrl Pts',(-0.0803060145807513,0.163540295435979,
-0.00762637684555866));
#26995=CARTESIAN_POINT('Ctrl Pts',(-0.134699947516894,0.136831074835686,
-0.00392093227453097));
#26996=CARTESIAN_POINT('Ctrl Pts',(-0.213794254954446,0.0253455914803241,
0.00348941659042212));
#26997=CARTESIAN_POINT('Ctrl Pts',(-0.137074231300261,-0.166276191191372,
0.0146046697493006));
#26998=CARTESIAN_POINT('Ctrl Pts',(0.0653047823526677,-0.205142119834331,
0.0257193826310768));
#26999=CARTESIAN_POINT('Ctrl Pts',(0.207809004042586,-0.0564757721103276,
0.0368340955128529));
#27000=CARTESIAN_POINT('Ctrl Pts',(0.160122180567089,0.144029275451672,
0.0479488083946291));
#27001=CARTESIAN_POINT('Ctrl Pts',(-0.0341737257862836,0.212610303572477,
0.0590635212764054));
#27002=CARTESIAN_POINT('Ctrl Pts',(-0.197172068603809,0.0865950800252895,
0.0701782341581814));
#27003=CARTESIAN_POINT('Ctrl Pts',(-0.179676046914621,-0.11871363819871,
0.0812929470399578));
#27004=CARTESIAN_POINT('Ctrl Pts',(0.00230818191877068,-0.215335378817728,
0.0924076599217337));
#27005=CARTESIAN_POINT('Ctrl Pts',(0.182177466579471,-0.114833718065218,
0.10352237280351));
#27006=CARTESIAN_POINT('Ctrl Pts',(0.195273273499442,0.0907954482718646,
0.114637085685286));
#27007=CARTESIAN_POINT('Ctrl Pts',(0.0296054996130767,0.213304335216675,
0.125751798567062));
#27008=CARTESIAN_POINT('Ctrl Pts',(-0.163164370533217,0.140544424819997,
0.136866511448838));
#27009=CARTESIAN_POINT('Ctrl Pts',(-0.206565453119791,-0.0608773960783323,
0.147981224330614));
#27010=CARTESIAN_POINT('Ctrl Pts',(-0.0608659742455931,-0.206568741920933,
0.159095937212391));
#27011=CARTESIAN_POINT('Ctrl Pts',(0.14055326168958,-0.163156708906222,
0.170210650094167));
#27012=CARTESIAN_POINT('Ctrl Pts',(0.213302939903473,0.0296173053948973,
0.181325362975943));
#27013=CARTESIAN_POINT('Ctrl Pts',(0.0907842855719502,0.195278105174824,
0.192440075857719));
#27014=CARTESIAN_POINT('Ctrl Pts',(-0.114842898840363,0.182171447697987,
0.203554788739495));
#27015=CARTESIAN_POINT('Ctrl Pts',(-0.215337076510083,0.0022958056732197,
0.214669501621272));
#27016=CARTESIAN_POINT('Ctrl Pts',(-0.118700779447527,-0.179681528545344,
0.225784214503048));
#27017=CARTESIAN_POINT('Ctrl Pts',(0.0866002260173578,-0.197169287738227,
0.236898927384824));
#27018=CARTESIAN_POINT('Ctrl Pts',(0.212622996139529,-0.0341582871157983,
0.2480136402666));
#27019=CARTESIAN_POINT('Ctrl Pts',(0.143999899637515,0.160122939994254,
0.259128353148376));
#27020=CARTESIAN_POINT('Ctrl Pts',(-0.0564480027761305,0.207819513167942,
0.270243066030152));
#27021=CARTESIAN_POINT('Ctrl Pts',(-0.205220542731821,0.0652675715182113,
0.281357778911928));
#27022=CARTESIAN_POINT('Ctrl Pts',(-0.166123797270203,-0.137033612757868,
0.292472491793705));
#27023=CARTESIAN_POINT('Ctrl Pts',(0.0250510913399055,-0.213887283110868,
0.303587204675481));
#27024=CARTESIAN_POINT('Ctrl Pts',(0.193292941358929,-0.0949376946806482,
0.314701917557257));
#27025=CARTESIAN_POINT('Ctrl Pts',(0.18458463677687,0.110922670883321,0.325816630439033));
#27026=CARTESIAN_POINT('Ctrl Pts',(0.00689820095215295,0.21523880197307,
0.336931343320809));
#27027=CARTESIAN_POINT('Ctrl Pts',(-0.177103197626001,0.122514425441503,
0.348046056202586));
#27028=CARTESIAN_POINT('Ctrl Pts',(-0.198975353515812,-0.082365865161802,
0.359160769084362));
#27029=CARTESIAN_POINT('Ctrl Pts',(-0.0386953867371307,-0.211844268499353,
0.370275481966138));
#27030=CARTESIAN_POINT('Ctrl Pts',(0.157008298141093,-0.147389692195589,
0.381390194847914));
#27031=CARTESIAN_POINT('Ctrl Pts',(0.208978629728527,0.0519928780455977,
0.392504907729691));
#27032=CARTESIAN_POINT('Ctrl Pts',(0.0696393326365127,0.203778532727666,
0.403619620611466));
#27033=CARTESIAN_POINT('Ctrl Pts',(-0.133451338868726,0.169014991065379,
0.414734333493244));
#27034=CARTESIAN_POINT('Ctrl Pts',(-0.214373891466652,-0.0204734390890087,
0.425849046375019));
#27035=CARTESIAN_POINT('Ctrl Pts',(-0.0990477193584199,-0.19121944550852,
0.436963759256795));
#27036=CARTESIAN_POINT('Ctrl Pts',(0.106951754783744,-0.186913480518035,
0.448078472138571));
#27037=CARTESIAN_POINT('Ctrl Pts',(0.215042172287536,-0.0114974426959434,
0.459193185020347));
#27038=CARTESIAN_POINT('Ctrl Pts',(0.126272086953288,0.174443936859812,
0.470307897902124));
#27039=CARTESIAN_POINT('Ctrl Pts',(-0.0780938662407537,0.200690495804509,
0.4814226107839));
#27040=CARTESIAN_POINT('Ctrl Pts',(-0.210968736484958,0.0432148039059421,
0.492537323665676));
#27041=CARTESIAN_POINT('Ctrl Pts',(-0.150712133466315,-0.153821909612123,
0.503652036547452));
#27042=CARTESIAN_POINT('Ctrl Pts',(0.0475139946104238,-0.210042251384927,
0.514766749429229));
#27043=CARTESIAN_POINT('Ctrl Pts',(0.202243404014021,-0.0739792713096693,
0.525881462311004));
#27044=CARTESIAN_POINT('Ctrl Pts',(0.171828951698061,0.129808082988056,
0.536996175192781));
#27045=CARTESIAN_POINT('Ctrl Pts',(-0.0158864312845783,0.214762539451667,
0.548110888074557));
#27046=CARTESIAN_POINT('Ctrl Pts',(-0.189058569945809,0.10311248314697,
0.559225600956334));
#27047=CARTESIAN_POINT('Ctrl Pts',(-0.189156912200222,-0.102931965965709,
0.570340313838109));
#27048=CARTESIAN_POINT('Ctrl Pts',(-0.0160914305641474,-0.214747276846734,
0.581455026719887));
#27049=CARTESIAN_POINT('Ctrl Pts',(0.171704962123206,-0.129972047121513,
0.59256973960166));
#27050=CARTESIAN_POINT('Ctrl Pts',(0.202313930484488,0.0737861815152819,
0.603684452483439));
#27051=CARTESIAN_POINT('Ctrl Pts',(0.0477144736208678,0.209996800113174,
0.614799165365213));
#27052=CARTESIAN_POINT('Ctrl Pts',(-0.150565230562319,0.153965705260633,
0.625913878246991));
#27053=CARTESIAN_POINT('Ctrl Pts',(-0.211009892050759,-0.04301339916137,
0.637028591128766));
#27054=CARTESIAN_POINT('Ctrl Pts',(-0.0782854043856557,-0.200615858074238,
0.648143304010544));
#27055=CARTESIAN_POINT('Ctrl Pts',(0.126105509954272,-0.174564393304767,
0.659258016892318));
#27056=CARTESIAN_POINT('Ctrl Pts',(0.215053049461418,0.0112921640101984,
0.670372729774096));
#27057=CARTESIAN_POINT('Ctrl Pts',(0.107130128614298,0.186811302103948,
0.68148744265587));
#27058=CARTESIAN_POINT('Ctrl Pts',(-0.0988651413156588,0.191313906664736,
0.692602155537648));
#27059=CARTESIAN_POINT('Ctrl Pts',(-0.214354250405077,0.0206780652858537,
0.703716868419422));
#27060=CARTESIAN_POINT('Ctrl Pts',(-0.133612615211503,-0.168887525018965,
0.714831581301201));
#27061=CARTESIAN_POINT('Ctrl Pts',(0.069444779427023,-0.203844915710499,
0.725946294182974));
#27062=CARTESIAN_POINT('Ctrl Pts',(0.208928903520267,-0.0521923397109899,
0.737061007064754));
#27063=CARTESIAN_POINT('Ctrl Pts',(0.15714892082517,0.147239749165004,0.748175719946527));
#27064=CARTESIAN_POINT('Ctrl Pts',(-0.0384931482923659,0.211881109552576,
0.759290432828306));
#27065=CARTESIAN_POINT('Ctrl Pts',(-0.19889663863233,0.082555764132184,
0.770405145710079));
#27066=CARTESIAN_POINT('Ctrl Pts',(-0.177220065897029,-0.122345311696611,
0.781519858591858));
#27067=CARTESIAN_POINT('Ctrl Pts',(0.00669273666407072,-0.215245288744339,
0.792634571473632));
#27068=CARTESIAN_POINT('Ctrl Pts',(0.184478668895337,-0.111098819855537,
0.803749284355411));
#27069=CARTESIAN_POINT('Ctrl Pts',(0.193383478250533,0.0947531392113955,
0.814863997237184));
#27070=CARTESIAN_POINT('Ctrl Pts',(0.0252552509506406,0.213863272560084,
0.825978710118963));
#27071=CARTESIAN_POINT('Ctrl Pts',(-0.165992913004264,0.137192127627818,
0.837093423000737));
#27072=CARTESIAN_POINT('Ctrl Pts',(-0.205282751882926,-0.0650716438247963,
0.848208135882515));
#27073=CARTESIAN_POINT('Ctrl Pts',(-0.0566463559688438,-0.20776553469269,
0.859322848764289));
#27074=CARTESIAN_POINT('Ctrl Pts',(0.143846985033473,-0.160260325556478,
0.870437561646068));
#27075=CARTESIAN_POINT('Ctrl Pts',(0.21265550577848,0.033955307579041,0.881552274527841));
#27076=CARTESIAN_POINT('Ctrl Pts',(0.0867883991639702,0.197086531303496,
0.892666987409619));
#27077=CARTESIAN_POINT('Ctrl Pts',(-0.118529206476762,0.179794755937645,
0.903781700291395));
#27078=CARTESIAN_POINT('Ctrl Pts',(-0.21533916945469,-0.00209025100234086,
0.91489641317317));
#27079=CARTESIAN_POINT('Ctrl Pts',(-0.115016743335963,-0.182061736240973,
0.926011126054948));
#27080=CARTESIAN_POINT('Ctrl Pts',(0.0905978386750332,-0.19536468124536,
0.937125838936722));
#27081=CARTESIAN_POINT('Ctrl Pts',(0.213274567669185,-0.0298208959659301,
0.9482405518185));
#27082=CARTESIAN_POINT('Ctrl Pts',(0.140708948675044,0.163022448802159,
0.959355264700275));
#27083=CARTESIAN_POINT('Ctrl Pts',(-0.060668773058382,0.206626781967583,
0.970469977582052));
#27084=CARTESIAN_POINT('Ctrl Pts',(-0.206507225243924,0.0610744870853927,
0.981584690463829));
#27085=CARTESIAN_POINT('Ctrl Pts',(-0.163298497665817,-0.140388488526573,
0.992699403345604));
#27086=CARTESIAN_POINT('Ctrl Pts',(0.0294019506348888,-0.213332726860067,
1.00381411622738));
#27087=CARTESIAN_POINT('Ctrl Pts',(0.195186363235098,-0.0909813753344305,
1.01492882910915));
#27088=CARTESIAN_POINT('Ctrl Pts',(0.182287286895232,0.11465893810368,1.02604354199093));
#27089=CARTESIAN_POINT('Ctrl Pts',(0.00251318982131648,0.215334648692705,
1.03715825487271));
#27090=CARTESIAN_POINT('Ctrl Pts',(-0.17956160858336,0.118882108719708,
1.04827296775448));
#27091=CARTESIAN_POINT('Ctrl Pts',(-0.197256610317911,-0.086401138514352,
1.05938768063626));
#27092=CARTESIAN_POINT('Ctrl Pts',(-0.0343729140127666,-0.2125884047472,
1.07050239351803));
#27093=CARTESIAN_POINT('Ctrl Pts',(0.159977489797147,-0.144161471305243,
1.08161710639981));
#27094=CARTESIAN_POINT('Ctrl Pts',(0.207876391795947,0.0562381790653505,
1.09273181928158));
#27095=CARTESIAN_POINT('Ctrl Pts',(0.0654747095800873,0.205154550171551,
1.10384653216336));
#27096=CARTESIAN_POINT('Ctrl Pts',(-0.136865840040237,0.166262048828855,
1.11496124504514));
#27097=CARTESIAN_POINT('Ctrl Pts',(-0.213912463334123,-0.0248351581637025,
1.12607595792691));
#27098=CARTESIAN_POINT('Ctrl Pts',(-0.0951327766195131,-0.193197002728692,
1.13719067080869));
#27099=CARTESIAN_POINT('Ctrl Pts',(0.110736275136736,-0.184696519781856,
1.14830538369047));
#27100=CARTESIAN_POINT('Ctrl Pts',(0.215231728524192,-0.00711548221675883,
1.15942009657224));
#27101=CARTESIAN_POINT('Ctrl Pts',(0.122693149687873,0.176979428381826,
1.17053480945402));
#27102=CARTESIAN_POINT('Ctrl Pts',(-0.0821649564551263,0.199058400931525,
1.18164952233579));
#27103=CARTESIAN_POINT('Ctrl Pts',(-0.211805097343413,0.0389092249991713,
1.19276423521757));
#27104=CARTESIAN_POINT('Ctrl Pts',(-0.147548117852297,-0.156859427414909,
1.20387894809935));
#27105=CARTESIAN_POINT('Ctrl Pts',(0.0517818864516966,-0.209031010345815,
1.21499366098112));
#27106=CARTESIAN_POINT('Ctrl Pts',(0.203708127594514,-0.069845012725504,
1.2261083738629));
#27107=CARTESIAN_POINT('Ctrl Pts',(0.169149624820075,0.13328064928532,1.23722308674468));
#27108=CARTESIAN_POINT('Ctrl Pts',(-0.0202570170087886,0.214394450284037,
1.24833779962645));
#27109=CARTESIAN_POINT('Ctrl Pts',(-0.191119358843245,0.0992407059932329,
1.25945251250823));
#27110=CARTESIAN_POINT('Ctrl Pts',(-0.187021353673497,-0.106763010077559,
1.27056722539));
#27111=CARTESIAN_POINT('Ctrl Pts',(-0.0117145231186205,-0.215030455979593,
1.28168193827178));
#27112=CARTESIAN_POINT('Ctrl Pts',(0.17431637559046,-0.12644812474566,1.29279665115356));
#27113=CARTESIAN_POINT('Ctrl Pts',(0.200769229739247,0.0778912282647907,
1.30391136403533));
#27114=CARTESIAN_POINT('Ctrl Pts',(0.0434277560106783,0.210925003398282,
1.31502607691711));
#27115=CARTESIAN_POINT('Ctrl Pts',(-0.153669686486467,0.150867340752861,
1.32614078979889));
#27116=CARTESIAN_POINT('Ctrl Pts',(-0.210090110002236,-0.0473019315666589,
1.33725550268066));
#27117=CARTESIAN_POINT('Ctrl Pts',(-0.074183399466186,-0.202168618470644,
1.34837021556244));
#27118=CARTESIAN_POINT('Ctrl Pts',(0.12963455455201,-0.171959906131605,
1.35948492844422));
#27119=CARTESIAN_POINT('Ctrl Pts',(0.214778467460861,0.0156696191993429,
1.37059964132599));
#27120=CARTESIAN_POINT('Ctrl Pts',(0.103303286294556,0.188954380979731,
1.38171435420777));
#27121=CARTESIAN_POINT('Ctrl Pts',(-0.102740958550925,0.189260726213141,
1.39282906708954));
#27122=CARTESIAN_POINT('Ctrl Pts',(-0.21473092303249,0.0163082109473484,
1.40394377997132));
#27123=CARTESIAN_POINT('Ctrl Pts',(-0.13014531801818,-0.171573667118924,
1.41505849285309));
#27124=CARTESIAN_POINT('Ctrl Pts',(0.0735819068678742,-0.202388314960068,
1.42617320573487));
#27125=CARTESIAN_POINT('Ctrl Pts',(0.209948525079889,-0.0479264422575633,
1.43728791861665));
#27126=CARTESIAN_POINT('Ctrl Pts',(0.154117623253518,0.150409724597099,
1.44840263149842));
#27127=CARTESIAN_POINT('Ctrl Pts',(-0.0428003615721995,0.211053206798612,
1.4595173443802));
#27128=CARTESIAN_POINT('Ctrl Pts',(-0.200536726294642,0.0784878873312067,
1.47063205726198));
#27129=CARTESIAN_POINT('Ctrl Pts',(-0.174691608576182,-0.125929221961204,
1.48174677014375));
#27130=CARTESIAN_POINT('Ctrl Pts',(0.0110750609944887,-0.215064339383955,
1.49286148302553));
#27131=CARTESIAN_POINT('Ctrl Pts',(0.186703058447294,-0.107318661085176,
1.5039761959073));
#27132=CARTESIAN_POINT('Ctrl Pts',(0.191413614096222,0.0986719584750968,
1.51509090878908));
#27133=CARTESIAN_POINT('Ctrl Pts',(0.0208944465695296,0.214333266557577,
1.52620562167086));
#27134=CARTESIAN_POINT('Ctrl Pts',(-0.168752556276368,0.133783040034527,
1.53732033455263));
#27135=CARTESIAN_POINT('Ctrl Pts',(-0.203914916736164,-0.0692389614535924,
1.54843504743441));
#27136=CARTESIAN_POINT('Ctrl Pts',(-0.0524032280183736,-0.208876108600153,
1.55954976031619));
#27137=CARTESIAN_POINT('Ctrl Pts',(0.147081031420287,-0.157297480103887,
1.57066447319796));
#27138=CARTESIAN_POINT('Ctrl Pts',(0.211919860637847,0.0382792335075298,
1.58177918607974));
#27139=CARTESIAN_POINT('Ctrl Pts',(0.0827565093400825,0.198813196776606,
1.59289389896151));
#27140=CARTESIAN_POINT('Ctrl Pts',(-0.122166344703153,0.177343483873975,
1.60400861184329));
#27141=CARTESIAN_POINT('Ctrl Pts',(-0.21525193542117,-0.0064754419253672,
1.61512332472507));
#27142=CARTESIAN_POINT('Ctrl Pts',(-0.111284995497834,-0.184366420011171,
1.62623803760684));
#27143=CARTESIAN_POINT('Ctrl Pts',(0.0945578692219636,-0.193479033538237,
1.63735275048862));
#27144=CARTESIAN_POINT('Ctrl Pts',(0.213837668268116,-0.0254711342571139,
1.6484674633704));
#27145=CARTESIAN_POINT('Ctrl Pts',(0.137359628499805,0.165854332198722,
1.65958217625217));
#27146=CARTESIAN_POINT('Ctrl Pts',(-0.0648643765760059,0.205348337470978,
1.67069688913395));
#27147=CARTESIAN_POINT('Ctrl Pts',(-0.207708244010933,0.0568560675793112,
1.68181160201572));
#27148=CARTESIAN_POINT('Ctrl Pts',(-0.160405458235323,-0.143685128036984,
1.6929263148975));
#27149=CARTESIAN_POINT('Ctrl Pts',(0.0337406133491248,-0.21268967549346,
1.70404102777928));
#27150=CARTESIAN_POINT('Ctrl Pts',(0.196998817501266,-0.0869873149016069,
1.71515574066105));
#27151=CARTESIAN_POINT('Ctrl Pts',(0.179914320222994,0.118347642263741,
1.72627045354283));
#27152=CARTESIAN_POINT('Ctrl Pts',(-0.00187286383573374,0.215341169848548,
1.73738516642461));
#27153=CARTESIAN_POINT('Ctrl Pts',(-0.18194553342259,0.115200477074783,
1.74849987930638));
#27154=CARTESIAN_POINT('Ctrl Pts',(-0.195456040724301,-0.0904005707673835,
1.75961459218816));
#27155=CARTESIAN_POINT('Ctrl Pts',(-0.0300361826450795,-0.213244354632895,
1.77072930506993));
#27156=CARTESIAN_POINT('Ctrl Pts',(0.162880319259612,-0.140873449054729,
1.78184401795171));
#27157=CARTESIAN_POINT('Ctrl Pts',(0.206687922148005,0.0604601512471564,
1.79295873083348));
#27158=CARTESIAN_POINT('Ctrl Pts',(0.0612829261690431,0.206445464980096,
1.80407344371526));
#27159=CARTESIAN_POINT('Ctrl Pts',(-0.140223566240549,0.163440137424902,
1.81518815659704));
#27160=CARTESIAN_POINT('Ctrl Pts',(-0.213362299590549,-0.0291865750666529,
1.82630286947881));
#27161=CARTESIAN_POINT('Ctrl Pts',(-0.0911783707051906,-0.195094417568098,
1.83741758236059));
#27162=CARTESIAN_POINT('Ctrl Pts',(0.114474859638751,-0.18240294285284,
1.84853229524236));
#27163=CARTESIAN_POINT('Ctrl Pts',(0.215332001889489,-0.00273057007850146,
1.85964700812414));
#27164=CARTESIAN_POINT('Ctrl Pts',(0.11906331659601,0.179441504930847,1.87076172100592));
#27165=CARTESIAN_POINT('Ctrl Pts',(-0.0862019628321077,0.197343732240425,
1.88187643388769));
#27166=CARTESIAN_POINT('Ctrl Pts',(-0.212553596772751,0.0345875056871029,
1.89299114676947));
#27167=CARTESIAN_POINT('Ctrl Pts',(-0.144322896022465,-0.15983187646517,
1.90410585965125));
#27168=CARTESIAN_POINT('Ctrl Pts',(0.0560282980235981,-0.207933058630097,
1.91522057253302));
#27169=CARTESIAN_POINT('Ctrl Pts',(0.205088348547649,-0.0656817808885113,
1.9263352854148));
#27170=CARTESIAN_POINT('Ctrl Pts',(0.166400130944419,0.136697927827634,
1.93744999829658));
#27171=CARTESIAN_POINT('Ctrl Pts',(-0.024619199675256,0.213937425566538,
1.94856471117835));
#27172=CARTESIAN_POINT('Ctrl Pts',(-0.193100867212448,0.0953277616043114,
1.95967942406013));
#27173=CARTESIAN_POINT('Ctrl Pts',(-0.184808214561534,-0.110549766536471,
1.9707941369419));
#27174=CARTESIAN_POINT('Ctrl Pts',(-0.00733275623034357,-0.215224435733384,
1.98190884982368));
#27175=CARTESIAN_POINT('Ctrl Pts',(0.176855478777783,-0.122871748896835,
1.99302356270546));
#27176=CARTESIAN_POINT('Ctrl Pts',(0.199141245486367,0.0819639640136945,
2.00413827558723));
#27177=CARTESIAN_POINT('Ctrl Pts',(0.0391230236087566,0.211765710336649,
2.01525298846901));
#27178=CARTESIAN_POINT('Ctrl Pts',(-0.156710396832941,0.147706393142391,
2.02636770135079));
#27179=CARTESIAN_POINT('Ctrl Pts',(-0.209083177939355,-0.0515708420868051,
2.03748241423256));
#27180=CARTESIAN_POINT('Ctrl Pts',(-0.0700506216350135,-0.203637514861929,
2.04859712711434));
#27181=CARTESIAN_POINT('Ctrl Pts',(0.133109823874788,-0.1692840861943,2.05971183999611));
#27182=CARTESIAN_POINT('Ctrl Pts',(0.214414790612736,0.0200405742850625,
2.0708265528779));
#27183=CARTESIAN_POINT('Ctrl Pts',(0.0994335914895629,0.19101907740701,
2.08194126575967));
#27184=CARTESIAN_POINT('Ctrl Pts',(-0.106574156565017,0.187129036236811,
2.09305597864144));
#27185=CARTESIAN_POINT('Ctrl Pts',(-0.215018520541286,0.0119315915998391,
2.10417069152322));
#27186=CARTESIAN_POINT('Ctrl Pts',(-0.126624033660108,-0.174188636668953,
2.11528540440499));
#27187=CARTESIAN_POINT('Ctrl Pts',(0.077688510882331,-0.200847759081134,
2.12640011728678));
#27188=CARTESIAN_POINT('Ctrl Pts',(0.210881055409674,-0.0436406638363383,
2.13751483016855));
#27189=CARTESIAN_POINT('Ctrl Pts',(0.15102239419105,0.153517306714328,2.14862954305032));
#27190=CARTESIAN_POINT('Ctrl Pts',(-0.0470898201287418,0.210137754595118,
2.1597442559321));
#27191=CARTESIAN_POINT('Ctrl Pts',(-0.202093627255768,0.0743874518723669,
2.17085896881387));
#27192=CARTESIAN_POINT('Ctrl Pts',(-0.172090684637681,-0.129460893719979,
2.18197368169565));
#27193=CARTESIAN_POINT('Ctrl Pts',(0.0154527898461788,-0.214794177131431,
2.19308839457743));
#27194=CARTESIAN_POINT('Ctrl Pts',(0.188850001921107,-0.103493983133494,
2.2042031074592));
#27195=CARTESIAN_POINT('Ctrl Pts',(0.189364342648829,0.102549844469193,
2.21531782034099));
#27196=CARTESIAN_POINT('Ctrl Pts',(0.0165249836546031,0.21471435412085,
2.22643253322275));
#27197=CARTESIAN_POINT('Ctrl Pts',(-0.171442214278381,0.130318449177449,
2.23754724610453));
#27198=CARTESIAN_POINT('Ctrl Pts',(-0.20246246081216,-0.0733775437143184,
2.24866195898631));
#27199=CARTESIAN_POINT('Ctrl Pts',(-0.0481384236319674,-0.209900061805832,
2.25977667186808));
#27200=CARTESIAN_POINT('Ctrl Pts',(0.150254182499086,-0.154269335258229,
2.27089138474987));
#27201=CARTESIAN_POINT('Ctrl Pts',(0.211096083593716,0.0425871872863454,
2.28200609763164));
#27202=CARTESIAN_POINT('Ctrl Pts',(0.0786907142771913,0.200457567222148,
2.29312081051341));
#27203=CARTESIAN_POINT('Ctrl Pts',(-0.125753612234005,0.174818308949879,
2.30423552339519));
#27204=CARTESIAN_POINT('Ctrl Pts',(-0.215073875643988,-0.010857305826902,
2.31535023627696));
#27205=CARTESIAN_POINT('Ctrl Pts',(-0.10751000343093,-0.186595843714485,
2.32646494915874));
#27206=CARTESIAN_POINT('Ctrl Pts',(0.0984842287439015,-0.19151080703399,
2.33757966204052));
#27207=CARTESIAN_POINT('Ctrl Pts',(0.214301498452045,-0.0211152191678184,
2.34869437492229));
#27208=CARTESIAN_POINT('Ctrl Pts',(0.133973432994688,0.168625811038259,
2.35980908780407));
#27209=CARTESIAN_POINT('Ctrl Pts',(-0.0690713533295226,0.203968730804155,
2.37092380068584));
#27210=CARTESIAN_POINT('Ctrl Pts',(-0.20874998875924,0.0526445260332857,
2.38203851356764));
#27211=CARTESIAN_POINT('Ctrl Pts',(-0.157587434446001,-0.146980669301764,
2.3931532264494));
#27212=CARTESIAN_POINT('Ctrl Pts',(0.0383765997278007,-0.211849228433297,
2.40426912699585));
#27213=CARTESIAN_POINT('Ctrl Pts',(0.144826643939091,-0.126070099887236,
2.41168012324836));
#27214=CARTESIAN_POINT('Ctrl Pts',(0.168155035031402,-0.07013107863996,
2.41538621520694));
#27215=CARTESIAN_POINT('Ctrl Pts',(-0.0862389315048216,0.175622466262465,
0.0001449026589043));
#27216=CARTESIAN_POINT('Ctrl Pts',(-0.144651426275569,0.146939998854253,
0.00385034722993199));
#27217=CARTESIAN_POINT('Ctrl Pts',(-0.229589131093048,0.0272180949214282,
0.011260696094885));
#27218=CARTESIAN_POINT('Ctrl Pts',(-0.147201119441583,-0.178560486881291,
0.0223759492537636));
#27219=CARTESIAN_POINT('Ctrl Pts',(0.0701294253195201,-0.220297786081225,
0.0334906621355397));
#27220=CARTESIAN_POINT('Ctrl Pts',(0.223161696658383,-0.0606481378528203,
0.0446053750173159));
#27221=CARTESIAN_POINT('Ctrl Pts',(0.171951824958788,0.154669994336176,
0.055720087899092));
#27222=CARTESIAN_POINT('Ctrl Pts',(-0.0366984417385652,0.228317710730976,
0.0668348007808684));
#27223=CARTESIAN_POINT('Ctrl Pts',(-0.211738916540169,0.092992625943922,
0.0779495136626443));
#27224=CARTESIAN_POINT('Ctrl Pts',(-0.192950308688839,-0.12748406662632,
0.0890642265444207));
#27225=CARTESIAN_POINT('Ctrl Pts',(0.00247870777093128,-0.231244111432686,
0.100178939426197));
#27226=CARTESIAN_POINT('Ctrl Pts',(0.195636530390518,-0.123317502410877,
0.111293652307973));
#27227=CARTESIAN_POINT('Ctrl Pts',(0.209699840615381,0.0975033126141929,
0.122408365189749));
#27228=CARTESIAN_POINT('Ctrl Pts',(0.0317927202168705,0.229063016642852,
0.133523078071525));
#27229=CARTESIAN_POINT('Ctrl Pts',(-0.175218768455904,0.150927686907536,
0.144637790953302));
#27230=CARTESIAN_POINT('Ctrl Pts',(-0.221826273609266,-0.0653749487880787,
0.155752503835078));
#27231=CARTESIAN_POINT('Ctrl Pts',(-0.0653626831233337,-0.221829805383293,
0.166867216716854));
#27232=CARTESIAN_POINT('Ctrl Pts',(0.150937176634988,-0.175210540796626,
0.17798192959863));
#27233=CARTESIAN_POINT('Ctrl Pts',(0.229061518245498,0.0318053981964183,
0.189096642480406));
#27234=CARTESIAN_POINT('Ctrl Pts',(0.0974913252267112,0.209705029249441,
0.200211355362183));
#27235=CARTESIAN_POINT('Ctrl Pts',(-0.123327361451243,0.195630066840919,
0.211326068243959));
#27236=CARTESIAN_POINT('Ctrl Pts',(-0.23124593454862,0.00246541718244239,
0.222440781125735));
#27237=CARTESIAN_POINT('Ctrl Pts',(-0.127470257885232,-0.192956195296204,
0.233555494007511));
#27238=CARTESIAN_POINT('Ctrl Pts',(0.0929981521160323,-0.211735930227402,
0.244670206889288));
#27239=CARTESIAN_POINT('Ctrl Pts',(0.228331341010431,-0.0366818624766748,
0.255784919771063));
#27240=CARTESIAN_POINT('Ctrl Pts',(0.15463844827031,0.171952640491572,0.26689963265284));
#27241=CARTESIAN_POINT('Ctrl Pts',(-0.0606183169518371,0.223172982185952,
0.278014345534616));
#27242=CARTESIAN_POINT('Ctrl Pts',(-0.220382002773095,0.0700894653909738,
0.289129058416392));
#27243=CARTESIAN_POINT('Ctrl Pts',(-0.178396834270733,-0.14715750004753,
0.300243771298168));
#27244=CARTESIAN_POINT('Ctrl Pts',(0.0269018374459491,-0.229689032063747,
0.311358484179945));
#27245=CARTESIAN_POINT('Ctrl Pts',(0.207573203791055,-0.101951583471458,
0.32247319706172));
#27246=CARTESIAN_POINT('Ctrl Pts',(0.198221539581392,0.119117511516148,
0.333587909943497));
#27247=CARTESIAN_POINT('Ctrl Pts',(0.00740783218448367,0.231140399600704,
0.344702622825273));
#27248=CARTESIAN_POINT('Ctrl Pts',(-0.190187380224124,0.131565651703181,
0.355817335707049));
#27249=CARTESIAN_POINT('Ctrl Pts',(-0.213675426088322,-0.0884509615015388,
0.366932048588825));
#27250=CARTESIAN_POINT('Ctrl Pts',(-0.0415541578522746,-0.227495081858827,
0.378046761470602));
#27251=CARTESIAN_POINT('Ctrl Pts',(0.168607892444504,-0.158278674843094,
0.389161474352377));
#27252=CARTESIAN_POINT('Ctrl Pts',(0.22441773295831,0.0558340526786359,
0.400276187234154));
#27253=CARTESIAN_POINT('Ctrl Pts',(0.0747842072431861,0.218833458711647,
0.41139090011593));
#27254=CARTESIAN_POINT('Ctrl Pts',(-0.143310571842089,0.181501626171699,
0.422505612997706));
#27255=CARTESIAN_POINT('Ctrl Pts',(-0.230211590490823,-0.021985993458684,
0.433620325879483));
#27256=CARTESIAN_POINT('Ctrl Pts',(-0.106365252092917,-0.205346520428016,
0.444735038761259));
#27257=CARTESIAN_POINT('Ctrl Pts',(0.114853228656257,-0.200722435646626,
0.455849751643035));
#27258=CARTESIAN_POINT('Ctrl Pts',(0.230929243137877,-0.0123468606717962,
0.466964464524811));
#27259=CARTESIAN_POINT('Ctrl Pts',(0.135600924969137,0.187331656300253,
0.478079177406587));
#27260=CARTESIAN_POINT('Ctrl Pts',(-0.0838633521641277,0.215517281136517,
0.489193890288364));
#27261=CARTESIAN_POINT('Ctrl Pts',(-0.226554866536053,0.0464074644158934,
0.500308603170139));
#27262=CARTESIAN_POINT('Ctrl Pts',(-0.161846574292104,-0.165186097158907,
0.511423316051917));
#27263=CARTESIAN_POINT('Ctrl Pts',(0.0510242744347459,-0.22555993377169,
0.522538028933691));
#27264=CARTESIAN_POINT('Ctrl Pts',(0.217184916436474,-0.079444775644238,
0.533652741815469));
#27265=CARTESIAN_POINT('Ctrl Pts',(0.184523479012063,0.139398156365019,
0.544767454697244));
#27266=CARTESIAN_POINT('Ctrl Pts',(-0.0170601027402429,0.230628951346473,
0.555882167579021));
#27267=CARTESIAN_POINT('Ctrl Pts',(-0.203026001839017,0.110730316002189,
0.566996880460796));
#27268=CARTESIAN_POINT('Ctrl Pts',(-0.203131609507214,-0.110536462417114,
0.578111593342573));
#27269=CARTESIAN_POINT('Ctrl Pts',(-0.017280247133175,-0.230612561157665,
0.589226306224349));
#27270=CARTESIAN_POINT('Ctrl Pts',(0.184390329228592,-0.139574233981967,
0.600341019106125));
#27271=CARTESIAN_POINT('Ctrl Pts',(0.217260653322277,0.0792374205956927,
0.611455731987902));
#27272=CARTESIAN_POINT('Ctrl Pts',(0.0512395646062169,0.225511124611729,
0.622570444869677));
#27273=CARTESIAN_POINT('Ctrl Pts',(-0.161688818368825,0.165340516266203,
0.633685157751454));
#27274=CARTESIAN_POINT('Ctrl Pts',(-0.226599062628197,-0.0461911801181109,
0.644799870633229));
#27275=CARTESIAN_POINT('Ctrl Pts',(-0.0840690409290904,-0.215437129255717,
0.655914583515006));
#27276=CARTESIAN_POINT('Ctrl Pts',(0.135422041451098,-0.18746101193021,
0.667029296396782));
#27277=CARTESIAN_POINT('Ctrl Pts',(0.230940923904982,0.0121264162304775,
0.678144009278559));
#27278=CARTESIAN_POINT('Ctrl Pts',(0.115044780542316,0.200612708407647,
0.689258722160335));
#27279=CARTESIAN_POINT('Ctrl Pts',(-0.106169185392238,0.2054479602669,0.700373435042111));
#27280=CARTESIAN_POINT('Ctrl Pts',(-0.230190498369983,0.0222057372059658,
0.711488147923888));
#27281=CARTESIAN_POINT('Ctrl Pts',(-0.143483763097442,-0.181364743078909,
0.722602860805663));
#27282=CARTESIAN_POINT('Ctrl Pts',(0.0745752806640969,-0.218904745993668,
0.73371757368744));
#27283=CARTESIAN_POINT('Ctrl Pts',(0.224364333034403,-0.0560482503447613,
0.744832286569215));
#27284=CARTESIAN_POINT('Ctrl Pts',(0.168758904172368,0.158117654192133,
0.755946999450992));
#27285=CARTESIAN_POINT('Ctrl Pts',(-0.0413369782614782,0.227534644687114,
0.767061712332768));
#27286=CARTESIAN_POINT('Ctrl Pts',(-0.213590895838874,0.0886548899916345,
0.778176425214544));
#27287=CARTESIAN_POINT('Ctrl Pts',(-0.190312882589949,-0.131384044027369,
0.78929113809632));
#27288=CARTESIAN_POINT('Ctrl Pts',(0.00718718842873861,-0.231147365607249,
0.800405850978096));
#27289=CARTESIAN_POINT('Ctrl Pts',(0.198107742913426,-0.119306674173869,
0.811520563859873));
#27290=CARTESIAN_POINT('Ctrl Pts',(0.207670429445126,0.101753393254271,
0.822635276741649));
#27291=CARTESIAN_POINT('Ctrl Pts',(0.0271210801362698,0.229663247640808,
0.833749989623426));
#27292=CARTESIAN_POINT('Ctrl Pts',(-0.178256280424249,0.147327725815587,
0.8448647025052));
#27293=CARTESIAN_POINT('Ctrl Pts',(-0.220448807865454,-0.0698790627826517,
0.855979415386978));
#27294=CARTESIAN_POINT('Ctrl Pts',(-0.0608313242525837,-0.223115015842409,
0.867094128268752));
#27295=CARTESIAN_POINT('Ctrl Pts',(0.154474236509428,-0.172100175942706,
0.878208841150531));
#27296=CARTESIAN_POINT('Ctrl Pts',(0.228366252424493,0.0364638870428536,
0.889323554032305));
#27297=CARTESIAN_POINT('Ctrl Pts',(0.0932002272804631,0.2116470598415,0.900438266914083));
#27298=CARTESIAN_POINT('Ctrl Pts',(-0.12728600929874,0.193077787799328,
0.911552979795857));
#27299=CARTESIAN_POINT('Ctrl Pts',(-0.231248182117593,-0.00224467636652307,
0.922667692677635));
#27300=CARTESIAN_POINT('Ctrl Pts',(-0.123514049380241,-0.195512250026378,
0.93378240555941));
#27301=CARTESIAN_POINT('Ctrl Pts',(0.0972911038453378,-0.209798001461494,
0.944897118441188));
#27302=CARTESIAN_POINT('Ctrl Pts',(0.229031049902846,-0.0320240298070313,
0.956011831322962));
#27303=CARTESIAN_POINT('Ctrl Pts',(0.151104365597674,0.175066361708942,
0.96712654420474));
#27304=CARTESIAN_POINT('Ctrl Pts',(-0.0651509129369443,0.221892133362506,
0.978241257086515));
#27305=CARTESIAN_POINT('Ctrl Pts',(-0.221763743924227,0.0655866006543337,
0.989355969968292));
#27306=CARTESIAN_POINT('Ctrl Pts',(-0.175362804748344,-0.150760230218302,
1.00047068285007));
#27307=CARTESIAN_POINT('Ctrl Pts',(0.0315741332719343,-0.229093505828532,
1.01158539573184));
#27308=CARTESIAN_POINT('Ctrl Pts',(0.209606509519663,-0.0977029757564454,
1.02270010861362));
#27309=CARTESIAN_POINT('Ctrl Pts',(0.195754464106167,0.123129809904786,
1.03381482149539));
#27310=CARTESIAN_POINT('Ctrl Pts',(0.00269886142389581,0.231243327366859,
1.04492953437717));
#27311=CARTESIAN_POINT('Ctrl Pts',(-0.192827415783965,0.127664983557588,
1.05604424725895));
#27312=CARTESIAN_POINT('Ctrl Pts',(-0.211829704099851,-0.0927843562549774,
1.06715896014072));
#27313=CARTESIAN_POINT('Ctrl Pts',(-0.0369123457644256,-0.228294194045422,
1.0782736730225));
#27314=CARTESIAN_POINT('Ctrl Pts',(0.171796444599506,-0.15481195666889,
1.08938838590428));
#27315=CARTESIAN_POINT('Ctrl Pts',(0.223234062942235,0.0603929917042014,
1.10050309878605));
#27316=CARTESIAN_POINT('Ctrl Pts',(0.0703119065770221,0.220311134757609,
1.11161781166783));
#27317=CARTESIAN_POINT('Ctrl Pts',(-0.14697733247254,0.17854529969713,1.1227325245496));
#27318=CARTESIAN_POINT('Ctrl Pts',(-0.229716072573226,-0.0266699513725409,
1.13384723743138));
#27319=CARTESIAN_POINT('Ctrl Pts',(-0.102161077841853,-0.207470177324048,
1.14496195031315));
#27320=CARTESIAN_POINT('Ctrl Pts',(0.118917345064028,-0.1983416883754,1.15607666319493));
#27321=CARTESIAN_POINT('Ctrl Pts',(0.231132803573477,-0.00764116594153085,
1.16719137607671));
#27322=CARTESIAN_POINT('Ctrl Pts',(0.131757579893385,0.190054467049106,
1.17830608895849));
#27323=CARTESIAN_POINT('Ctrl Pts',(-0.0882352098883608,0.213764608952554,
1.18942080184026));
#27324=CARTESIAN_POINT('Ctrl Pts',(-0.227453016782484,0.041783794241647,
1.20053551472204));
#27325=CARTESIAN_POINT('Ctrl Pts',(-0.158448804806942,-0.168448023318568,
1.21165022760381));
#27326=CARTESIAN_POINT('Ctrl Pts',(0.0556074732660041,-0.224473983395965,
1.22276494048559));
#27327=CARTESIAN_POINT('Ctrl Pts',(0.218757852127418,-0.0750050827429731,
1.23387965336737));
#27328=CARTESIAN_POINT('Ctrl Pts',(0.181646206514904,0.143127271906602,
1.24499436624914));
#27329=CARTESIAN_POINT('Ctrl Pts',(-0.0217535823615871,0.230233668170229,
1.25610907913092));
#27330=CARTESIAN_POINT('Ctrl Pts',(-0.205239039473866,0.106572496360582,
1.2672237920127));
#27331=CARTESIAN_POINT('Ctrl Pts',(-0.200838278347996,-0.114650539706076,
1.27833850489447));
#27332=CARTESIAN_POINT('Ctrl Pts',(-0.012579978748941,-0.230916661242444,
1.28945321777625));
#27333=CARTESIAN_POINT('Ctrl Pts',(0.187194670949558,-0.13578996823318,
1.30056793065802));
#27334=CARTESIAN_POINT('Ctrl Pts',(0.215601831844711,0.0836457435252159,
1.3116826435398));
#27335=CARTESIAN_POINT('Ctrl Pts',(0.0466361491796686,0.226507902498727,
1.32279735642157));
#27336=CARTESIAN_POINT('Ctrl Pts',(-0.165022627962041,0.162013248116267,
1.33391206930335));
#27337=CARTESIAN_POINT('Ctrl Pts',(-0.225611328129155,-0.050796544414754,
1.34502678218513));
#27338=CARTESIAN_POINT('Ctrl Pts',(-0.079663984556546,-0.217104605822299,
1.3561414950669));
#27339=CARTESIAN_POINT('Ctrl Pts',(0.13921180784569,-0.184664108210057,
1.36725620794868));
#27340=CARTESIAN_POINT('Ctrl Pts',(0.230646056098852,0.0168272728250036,
1.37837092083046));
#27341=CARTESIAN_POINT('Ctrl Pts',(0.110935215469079,0.202914115510752,
1.38948563371223));
#27342=CARTESIAN_POINT('Ctrl Pts',(-0.110331343591998,0.203243093181209,
1.40060034659401));
#27343=CARTESIAN_POINT('Ctrl Pts',(-0.230594999142245,0.0175130430042696,
1.41171505947578));
#27344=CARTESIAN_POINT('Ctrl Pts',(-0.139760305935199,-0.184249334298881,
1.42282977235756));
#27345=CARTESIAN_POINT('Ctrl Pts',(0.079018054369913,-0.217340533238222,
1.43394448523934));
#27346=CARTESIAN_POINT('Ctrl Pts',(0.22545928307395,-0.0514671932444525,
1.44505919812111));
#27347=CARTESIAN_POINT('Ctrl Pts',(0.165503657787434,0.161521823799947,
1.45617391100289));
#27348=CARTESIAN_POINT('Ctrl Pts',(-0.0459624035544085,0.226645577420305,
1.46728862388466));
#27349=CARTESIAN_POINT('Ctrl Pts',(-0.215352151310341,0.0842864830841198,
1.47840333676644));
#27350=CARTESIAN_POINT('Ctrl Pts',(-0.187597625721037,-0.135232729501817,
1.48951804964822));
#27351=CARTESIAN_POINT('Ctrl Pts',(0.011893273891152,-0.230953047914141,
1.50063276252999));
#27352=CARTESIAN_POINT('Ctrl Pts',(0.200496467832881,-0.115247241577487,
1.51174747541177));
#27353=CARTESIAN_POINT('Ctrl Pts',(0.205555033969902,0.105961730423366,
1.52286218829354));
#27354=CARTESIAN_POINT('Ctrl Pts',(0.0224381044925165,0.230167964259722,
1.53397690117532));
#27355=CARTESIAN_POINT('Ctrl Pts',(-0.181219802999278,0.143666778712352,
1.5450916140571));
#27356=CARTESIAN_POINT('Ctrl Pts',(-0.218979918615408,-0.0743542570931251,
1.55620632693887));
#27357=CARTESIAN_POINT('Ctrl Pts',(-0.0562747188401855,-0.224307637685701,
1.56732103982065));
#27358=CARTESIAN_POINT('Ctrl Pts',(0.157947210561147,-0.168918438841454,
1.57843575270243));
#27359=CARTESIAN_POINT('Ctrl Pts',(0.227576258658446,0.0411072596958934,
1.5895504655842));
#27360=CARTESIAN_POINT('Ctrl Pts',(0.0888704660269324,0.213501289393851,
1.60066517846598));
#27361=CARTESIAN_POINT('Ctrl Pts',(-0.131191855156199,0.190445418546512,
1.61177989134775));
#27362=CARTESIAN_POINT('Ctrl Pts',(-0.231154503332997,-0.00695384020214284,
1.62289460422953));
#27363=CARTESIAN_POINT('Ctrl Pts',(-0.119506604260646,-0.197987201209499,
1.63400931711131));
#27364=CARTESIAN_POINT('Ctrl Pts',(0.101543696940346,-0.207773044248692,
1.64512402999308));
#27365=CARTESIAN_POINT('Ctrl Pts',(0.229635751732902,-0.0273529126556294,
1.65623874287486));
#27366=CARTESIAN_POINT('Ctrl Pts',(0.147507601461287,0.178107461426576,
1.66735345575664));
#27367=CARTESIAN_POINT('Ctrl Pts',(-0.0696564828655069,0.220519238842077,
1.67846816863841));
#27368=CARTESIAN_POINT('Ctrl Pts',(-0.223053492590313,0.0610565291180635,
1.68958288152019));
#27369=CARTESIAN_POINT('Ctrl Pts',(-0.172256030858622,-0.154300421702323,
1.70069759440197));
#27370=CARTESIAN_POINT('Ctrl Pts',(0.0362333314476733,-0.228402946559112,
1.71181230728374));
#27371=CARTESIAN_POINT('Ctrl Pts',(0.211552865843429,-0.0934138386863192,
1.72292702016552));
#27372=CARTESIAN_POINT('Ctrl Pts',(0.193206185357947,0.127091031328383,
1.73404173304729));
#27373=CARTESIAN_POINT('Ctrl Pts',(-0.00201122888355521,0.23125033029827,
1.74515644592907));
#27374=CARTESIAN_POINT('Ctrl Pts',(-0.195387462276077,0.123711357158493,
1.75627115881084));
#27375=CARTESIAN_POINT('Ctrl Pts',(-0.209896110474722,-0.0970792620092718,
1.76738587169262));
#27376=CARTESIAN_POINT('Ctrl Pts',(-0.0322552216209195,-0.228998604761835,
1.7785005845744));
#27377=CARTESIAN_POINT('Ctrl Pts',(0.174913731797615,-0.151281019078116,
1.78961529745618));
#27378=CARTESIAN_POINT('Ctrl Pts',(0.221957790509845,0.0649268783838334,
1.80073001033795));
#27379=CARTESIAN_POINT('Ctrl Pts',(0.0658104389801637,0.221697420882426,
1.81184472321973));
#27380=CARTESIAN_POINT('Ctrl Pts',(-0.15058312366156,0.175514908691566,
1.8229594361015));
#27381=CARTESIAN_POINT('Ctrl Pts',(-0.229125263358671,-0.0313428460019351,
1.83407414898328));
#27382=CARTESIAN_POINT('Ctrl Pts',(-0.097914524920906,-0.20950777101147,
1.84518886186505));
#27383=CARTESIAN_POINT('Ctrl Pts',(0.122932131932451,-0.195878664594243,
1.85630357474683));
#27384=CARTESIAN_POINT('Ctrl Pts',(0.231240485020835,-0.0029323014869812,
1.86741828762861));
#27385=CARTESIAN_POINT('Ctrl Pts',(0.127859578865474,0.192698439010348,
1.87853300051039));
#27386=CARTESIAN_POINT('Ctrl Pts',(-0.0925704657001019,0.211923262490807,
1.88964771339216));
#27387=CARTESIAN_POINT('Ctrl Pts',(-0.228256814497451,0.0371427912273366,
1.90076242627394));
#27388=CARTESIAN_POINT('Ctrl Pts',(-0.154985307260428,-0.171640073520352,
1.91187713915571));
#27389=CARTESIAN_POINT('Ctrl Pts',(0.0601676048900462,-0.223294916257574,
1.92299185203749));
#27390=CARTESIAN_POINT('Ctrl Pts',(0.220240042233107,-0.0705342760779494,
1.93410656491926));
#27391=CARTESIAN_POINT('Ctrl Pts',(0.178693583162176,0.146797015096847,
1.94522127780104));
#27392=CARTESIAN_POINT('Ctrl Pts',(-0.0264380381168497,0.229742878986952,
1.95633599068282));
#27393=CARTESIAN_POINT('Ctrl Pts',(-0.207366939425321,0.102370468095326,
1.96745070356459));
#27394=CARTESIAN_POINT('Ctrl Pts',(-0.19846163503823,-0.118717057420726,
1.97856541644637));
#27395=CARTESIAN_POINT('Ctrl Pts',(-0.00787449191185959,-0.231124971999587,
1.98968012932815));
#27396=CARTESIAN_POINT('Ctrl Pts',(0.189921360189439,-0.13194937380856,
2.00079484220992));
#27397=CARTESIAN_POINT('Ctrl Pts',(0.213853573968784,0.0880193683541974,
2.0119095550917));
#27398=CARTESIAN_POINT('Ctrl Pts',(0.0420133880490859,0.227410719908507,
2.02302426797347));
#27399=CARTESIAN_POINT('Ctrl Pts',(-0.168287982526885,0.158618773295263,
2.03413898085525));
#27400=CARTESIAN_POINT('Ctrl Pts',(-0.22453000507192,-0.0553808371837207,
2.04525369373703));
#27401=CARTESIAN_POINT('Ctrl Pts',(-0.075225881804619,-0.218682022606547,
2.0563684066188));
#27402=CARTESIAN_POINT('Ctrl Pts',(0.142943826109234,-0.181790601742365,
2.06748311950058));
#27403=CARTESIAN_POINT('Ctrl Pts',(0.230255511219254,0.0215211490958647,
2.07859783238236));
#27404=CARTESIAN_POINT('Ctrl Pts',(0.106779632017769,0.205131349359298,
2.08971254526413));
#27405=CARTESIAN_POINT('Ctrl Pts',(-0.114447733911049,0.200953916376482,
2.10082725814591));
#27406=CARTESIAN_POINT('Ctrl Pts',(-0.230903844027544,0.0128130840024069,
2.11194197102768));
#27407=CARTESIAN_POINT('Ctrl Pts',(-0.135978873097944,-0.187057494821968,
2.12305668390946));
#27408=CARTESIAN_POINT('Ctrl Pts',(0.0834280496133461,-0.215686162844967,
2.13417139679123));
#27409=CARTESIAN_POINT('Ctrl Pts',(0.226460707682758,-0.0468647863930802,
2.14528610967301));
#27410=CARTESIAN_POINT('Ctrl Pts',(0.162179756725932,0.164858990545831,
2.15640082255479));
#27411=CARTESIAN_POINT('Ctrl Pts',(-0.0505687624253055,0.225662492650313,
2.16751553543657));
#27412=CARTESIAN_POINT('Ctrl Pts',(-0.21702407434185,0.0798831121221699,
2.17863024831834));
#27413=CARTESIAN_POINT('Ctrl Pts',(-0.184804548483264,-0.139025317149112,
2.18974496120012));
#27414=CARTESIAN_POINT('Ctrl Pts',(0.016594424366101,-0.230662926381996,
2.20085967408189));
#27415=CARTESIAN_POINT('Ctrl Pts',(0.202802025046116,-0.111140000773359,
2.21197438696367));
#27416=CARTESIAN_POINT('Ctrl Pts',(0.203354364681193,0.110126110219503,
2.22308909984544));
#27417=CARTESIAN_POINT('Ctrl Pts',(0.0177458306323277,0.230577206138279,
2.23420381272722));
#27418=CARTESIAN_POINT('Ctrl Pts',(-0.184108169872144,0.139946227827396,
2.245318525609));
#27419=CARTESIAN_POINT('Ctrl Pts',(-0.217420156901447,-0.0787985930992519,
2.25643323849078));
#27420=CARTESIAN_POINT('Ctrl Pts',(-0.0516948355614441,-0.225407239388384,
2.26754795137255));
#27421=CARTESIAN_POINT('Ctrl Pts',(0.161354790428826,-0.16566657810232,
2.27866266425433));
#27422=CARTESIAN_POINT('Ctrl Pts',(0.226691621904214,0.0457334801950268,
2.2897773771361));
#27423=CARTESIAN_POINT('Ctrl Pts',(0.0845042946539431,0.215267144055698,
2.30089209001788));
#27424=CARTESIAN_POINT('Ctrl Pts',(-0.135044145927914,0.187733686574086,
2.31200680289966));
#27425=CARTESIAN_POINT('Ctrl Pts',(-0.230963288702208,-0.011659431219711,
2.32312151578143));
#27426=CARTESIAN_POINT('Ctrl Pts',(-0.115452720077891,-0.200381332197683,
2.33423622866321));
#27427=CARTESIAN_POINT('Ctrl Pts',(0.105760131433371,-0.205659407411252,
2.34535094154498));
#27428=CARTESIAN_POINT('Ctrl Pts',(0.230133849162723,-0.0226751875190042,
2.35646565442676));
#27429=CARTESIAN_POINT('Ctrl Pts',(0.143871237687637,0.181083693967286,
2.36758036730854));
#27430=CARTESIAN_POINT('Ctrl Pts',(-0.0741742662716807,0.219037708405472,
2.37869508019031));
#27431=CARTESIAN_POINT('Ctrl Pts',(-0.224172200254536,0.0565338436777074,
2.38980979307209));
#27432=CARTESIAN_POINT('Ctrl Pts',(-0.169229814680232,-0.157839433803576,
2.40092450595386));
#27433=CARTESIAN_POINT('Ctrl Pts',(0.0412118192216604,-0.227500408227043,
2.4120404065003));
#27434=CARTESIAN_POINT('Ctrl Pts',(0.155526271499594,-0.13538401532862,
2.41945140275281));
#27435=CARTESIAN_POINT('Ctrl Pts',(0.180578137565047,-0.0753122828814866,
2.4231574947114));
#27436=CARTESIAN_POINT('Ctrl Pts',(-0.15199516870275,-0.123304110510785,
2.4));
#27437=CARTESIAN_POINT('Ctrl Pts',(-0.148824665831025,-0.126538769486475,
2.4));
#27438=CARTESIAN_POINT('Ctrl Pts',(-0.145540355431101,-0.129648441844686,
2.4));
#27439=CARTESIAN_POINT('Ctrl Pts',(-0.142144069729336,-0.132625074476752,
2.4));
#27440=CARTESIAN_POINT('Ctrl Pts',(-0.132540690324889,-0.141041837677364,
2.4));
#27441=CARTESIAN_POINT('Ctrl Pts',(-0.122043505462798,-0.148398554468019,
2.4));
#27442=CARTESIAN_POINT('Ctrl Pts',(-0.110860112905452,-0.154651338932229,
2.4));
#27443=CARTESIAN_POINT('Ctrl Pts',(-0.105435415437936,-0.157684359893801,
2.4));
#27444=CARTESIAN_POINT('Ctrl Pts',(-0.099848934821215,-0.160456894218315,
2.4));
#27445=CARTESIAN_POINT('Ctrl Pts',(-0.0941236483875528,-0.162959592659119,
2.4));
#27446=CARTESIAN_POINT('Ctrl Pts',(-0.0907590799609226,-0.164430348795581,
2.4));
#27447=CARTESIAN_POINT('Ctrl Pts',(-0.0873466982488514,-0.16580752592612,
2.4));
#27448=CARTESIAN_POINT('Ctrl Pts',(-0.0839043527287589,-0.167084756767952,
2.4));
#27449=CARTESIAN_POINT('Ctrl Pts',(-0.0722287249452664,-0.171416823905253,
2.4));
#27450=CARTESIAN_POINT('Ctrl Pts',(-0.0601713335654445,-0.174620056925232,
2.4));
#27451=CARTESIAN_POINT('Ctrl Pts',(-0.0479233473597519,-0.176639901583043,
2.4));
#27452=CARTESIAN_POINT('Ctrl Pts',(-0.0398564206582088,-0.177970237732139,
2.4));
#27453=CARTESIAN_POINT('Ctrl Pts',(-0.0317065647200675,-0.178786199153318,
2.4));
#27454=CARTESIAN_POINT('Ctrl Pts',(-0.0235309431251825,-0.179059833327106,
2.4));
#27455=CARTESIAN_POINT('Ctrl Pts',(-0.0192489471657408,-0.179203149699191,
2.4));
#27456=CARTESIAN_POINT('Ctrl Pts',(-0.0149655652356923,-0.179197037719655,
2.4));
#27457=CARTESIAN_POINT('Ctrl Pts',(-0.0107021384747464,-0.179038942029942,
2.4));
#27458=CARTESIAN_POINT('Ctrl Pts',(-0.00225095961565695,-0.178725556805913,
2.4));
#27459=CARTESIAN_POINT('Ctrl Pts',(0.00613674255370757,-0.177816520060091,
2.4));
#27460=CARTESIAN_POINT('Ctrl Pts',(0.014397712940729,-0.176286708862887,
2.4));
#27461=CARTESIAN_POINT('Ctrl Pts',(0.0175977987980585,-0.175694099647843,
2.4));
#27462=CARTESIAN_POINT('Ctrl Pts',(0.0207787832759882,-0.175008200507475,
2.4));
#27463=CARTESIAN_POINT('Ctrl Pts',(0.0239367001203762,-0.174227024096589,
2.4));
#27464=CARTESIAN_POINT('Ctrl Pts',(0.0263036255441011,-0.173641515864912,
2.4));
#27465=CARTESIAN_POINT('Ctrl Pts',(0.0286575889694442,-0.173002476522167,
2.4));
#27466=CARTESIAN_POINT('Ctrl Pts',(0.0309968484005305,-0.172308959609583,
2.4));
#27467=CARTESIAN_POINT('Ctrl Pts',(0.0360874731122647,-0.170799749350007,
2.4));
#27468=CARTESIAN_POINT('Ctrl Pts',(0.0411108443148083,-0.16903165817095,
2.4));
#27469=CARTESIAN_POINT('Ctrl Pts',(0.0460449062726198,-0.16701820095113,
2.4));
#27470=CARTESIAN_POINT('Ctrl Pts',(0.0500648589951711,-0.16537776698379,
2.4));
#27471=CARTESIAN_POINT('Ctrl Pts',(0.0540173393440258,-0.163577829383814,
2.4));
#27472=CARTESIAN_POINT('Ctrl Pts',(0.0578908054835579,-0.161628640771827,
2.4));
#27473=CARTESIAN_POINT('Ctrl Pts',(0.0680358083015658,-0.156523517027585,
2.4));
#27474=CARTESIAN_POINT('Ctrl Pts',(0.0776550402843555,-0.150390999806698,
2.4));
#27475=CARTESIAN_POINT('Ctrl Pts',(0.086613738132899,-0.143350130393655,
2.4));
#27476=CARTESIAN_POINT('Ctrl Pts',(0.0907533250321785,-0.140096723338911,
2.4));
#27477=CARTESIAN_POINT('Ctrl Pts',(0.0947518982198043,-0.136648454397042,
2.4));
#27478=CARTESIAN_POINT('Ctrl Pts',(0.09859173507754,-0.133016695765916,
2.4));
#27479=CARTESIAN_POINT('Ctrl Pts',(0.102112604578935,-0.129686619860478,
2.4));
#27480=CARTESIAN_POINT('Ctrl Pts',(0.105494621732796,-0.126206936464483,
2.4));
#27481=CARTESIAN_POINT('Ctrl Pts',(0.108717820867798,-0.122595988102291,
2.4));
#27482=CARTESIAN_POINT('Ctrl Pts',(0.1145699112897,-0.116039894159817,2.4));
#27483=CARTESIAN_POINT('Ctrl Pts',(0.119909157676967,-0.109042420774433,
2.4));
#27484=CARTESIAN_POINT('Ctrl Pts',(0.124658963353444,-0.101655155004293,
2.4));
#27485=CARTESIAN_POINT('Ctrl Pts',(0.127026507874596,-0.097972966344028,
2.4));
#27486=CARTESIAN_POINT('Ctrl Pts',(0.129246602375859,-0.0941942185358602,
2.4));
#27487=CARTESIAN_POINT('Ctrl Pts',(0.131302274414547,-0.0903383755883276,
2.4));
#27488=CARTESIAN_POINT('Ctrl Pts',(0.13645721812277,-0.0806692002684345,
2.4));
#27489=CARTESIAN_POINT('Ctrl Pts',(0.140595547790541,-0.0704960807205455,
2.4));
#27490=CARTESIAN_POINT('Ctrl Pts',(0.143545299885864,-0.0599211930845618,
2.4));
#27491=CARTESIAN_POINT('',(-0.0904498980258696,-0.126704579043882,-7.30113716837731E-5));
#27492=CARTESIAN_POINT('Ctrl Pts',(-0.0905547187627354,-0.126790994435269,
1.91686944095437E-16));
#27493=CARTESIAN_POINT('Ctrl Pts',(-0.0937786982673176,-0.125067385071004,
-8.80357328303703E-17));
#27494=CARTESIAN_POINT('Ctrl Pts',(-0.0969317870940272,-0.123225562125392,
7.25923314697896E-17));
#27495=CARTESIAN_POINT('Ctrl Pts',(-0.100006715605072,-0.121266986978485,
7.89299181569447E-17));
#27496=CARTESIAN_POINT('Ctrl Pts',(-0.107443591426572,-0.116530070298209,
9.7298243307645E-17));
#27497=CARTESIAN_POINT('Ctrl Pts',(-0.114423960357986,-0.111111926712851,
-8.60222442940798E-17));
#27498=CARTESIAN_POINT('Ctrl Pts',(-0.120920626723875,-0.105114084706488,
1.07552855510562E-16));
#27499=CARTESIAN_POINT('Ctrl Pts',(-0.124692476039581,-0.101631843970501,
1.99916285244735E-16));
#27500=CARTESIAN_POINT('Ctrl Pts',(-0.128299160177052,-0.0979546858534835,
1.21953705927638E-16));
#27501=CARTESIAN_POINT('Ctrl Pts',(-0.131721852029444,-0.0941163405780606,
1.34441069388203E-16));
#27502=CARTESIAN_POINT('Ctrl Pts',(-0.137478284443309,-0.0876608441115559,
1.55442861804271E-16));
#27503=CARTESIAN_POINT('Ctrl Pts',(-0.142725690997129,-0.0807408650802736,
3.13072395126118E-16));
#27504=CARTESIAN_POINT('Ctrl Pts',(-0.147437251084092,-0.0734399138115947,
2.74086309204336E-16));
#27505=CARTESIAN_POINT('Ctrl Pts',(-0.150181027130752,-0.069188206343348,
2.51382770093966E-16));
#27506=CARTESIAN_POINT('Ctrl Pts',(-0.152742174737604,-0.0648067631725966,
1.97653338405712E-16));
#27507=CARTESIAN_POINT('Ctrl Pts',(-0.155103784497403,-0.0603327855088824,
1.76074432811646E-16));
#27508=CARTESIAN_POINT('Ctrl Pts',(-0.160567427408146,-0.0499821269194385,
1.26151098068711E-16));
#27509=CARTESIAN_POINT('Ctrl Pts',(-0.164980553993685,-0.0391180362903603,
8.13475317118353E-18));
#27510=CARTESIAN_POINT('Ctrl Pts',(-0.168274787260813,-0.0279332056041401,
4.68375338513738E-17));
#27511=CARTESIAN_POINT('Ctrl Pts',(-0.169906523489982,-0.0223930109767741,
6.60082252640462E-17));
#27512=CARTESIAN_POINT('Ctrl Pts',(-0.171263202886852,-0.0167734941869636,
1.43754342025142E-16));
#27513=CARTESIAN_POINT('Ctrl Pts',(-0.17233265600195,-0.0110954126933409,
2.48065457064683E-16));
#27514=CARTESIAN_POINT('Ctrl Pts',(-0.173163133015681,-0.00668613462778462,
3.290675899249E-16));
#27515=CARTESIAN_POINT('Ctrl Pts',(-0.173819585336133,-0.0022423248069032,
-2.23512275233336E-18));
#27516=CARTESIAN_POINT('Ctrl Pts',(-0.174294602869972,0.00220394339803012,
-1.73472347597681E-18));
#27517=CARTESIAN_POINT('Ctrl Pts',(-0.174947783696855,0.00831785906587972,
-1.04664105834344E-18));
#27518=CARTESIAN_POINT('Ctrl Pts',(-0.175260256565538,0.0144468401589108,
2.92331180691467E-16));
#27519=CARTESIAN_POINT('Ctrl Pts',(-0.175221744250391,0.0205647925020219,
2.39391839684799E-16));
#27520=CARTESIAN_POINT('Ctrl Pts',(-0.175173289109206,0.028262232747164,
1.62396291645263E-16));
#27521=CARTESIAN_POINT('Ctrl Pts',(-0.174569669212428,0.0359422811365845,
-1.12250719804115E-16));
#27522=CARTESIAN_POINT('Ctrl Pts',(-0.173446373975916,0.0435656717636887,
-4.5102810375397E-17));
#27523=CARTESIAN_POINT('Ctrl Pts',(-0.172637904118492,0.0490524586146037,
5.18085424066423E-17));
#27524=CARTESIAN_POINT('Ctrl Pts',(-0.171559653499544,0.0545113728394569,
5.96783951772411E-17));
#27525=CARTESIAN_POINT('Ctrl Pts',(-0.170222848604401,0.0599234158566936,
1.73472347597681E-17));
#27526=CARTESIAN_POINT('Ctrl Pts',(-0.169222922852311,0.0639716065867067,
-1.43163367689382E-17));
#27527=CARTESIAN_POINT('Ctrl Pts',(-0.168079794711886,0.0679869286825006,
9.01404419406027E-17));
#27528=CARTESIAN_POINT('Ctrl Pts',(-0.166801973771595,0.0719549338288062,
9.8879238130678E-17));
#27529=CARTESIAN_POINT('Ctrl Pts',(-0.163394778652899,0.0825352642484763,
1.22180455682585E-16));
#27530=CARTESIAN_POINT('Ctrl Pts',(-0.159027462790524,0.0927996140500163,
1.91178027158399E-16));
#27531=CARTESIAN_POINT('Ctrl Pts',(-0.153795590326359,0.102636459258385,
1.00613961606655E-16));
#27532=CARTESIAN_POINT('Ctrl Pts',(-0.150728825820311,0.108402518722398,
4.75280609736047E-17));
#27533=CARTESIAN_POINT('Ctrl Pts',(-0.147364797318139,0.114021013727962,
-1.44861482947255E-16));
#27534=CARTESIAN_POINT('Ctrl Pts',(-0.143715779143174,0.119470837464023,
3.46944695195361E-18));
#27535=CARTESIAN_POINT('Ctrl Pts',(-0.140547585855608,0.124202547242139,
1.32255063770552E-16));
#27536=CARTESIAN_POINT('Ctrl Pts',(-0.13716418235433,0.128805658068609,
-3.06595871754581E-17));
#27537=CARTESIAN_POINT('Ctrl Pts',(-0.133596163369402,0.13323881795393,
-6.59194920871187E-17));
#27538=CARTESIAN_POINT('Ctrl Pts',(-0.125566297160433,0.143215693332807,
-1.45272298273861E-16));
#27539=CARTESIAN_POINT('Ctrl Pts',(-0.116585657780435,0.152364342920442,
-1.57993899402886E-16));
#27540=CARTESIAN_POINT('Ctrl Pts',(-0.106768224044845,0.160520635554423,
-6.93889390390723E-18));
#27541=CARTESIAN_POINT('Ctrl Pts',(-0.100257772229834,0.165929498156689,
9.32335504643276E-17));
#27542=CARTESIAN_POINT('Ctrl Pts',(-0.093378247512691,0.170901777887464,
2.69387857240372E-16));
#27543=CARTESIAN_POINT('Ctrl Pts',(-0.0861525859670521,0.175382131162754,
-2.42861286636753E-17));
#27544=CARTESIAN_POINT('Ctrl Pts',(-0.0903762848818376,-0.126601459829486,
-7.30113716837788E-5));
#27545=CARTESIAN_POINT('Ctrl Pts',(-0.0898498377495766,-0.126977271736114,
-4.86742477891657E-5));
#27546=CARTESIAN_POINT('Ctrl Pts',(-0.0893210464778968,-0.127349799910583,
-2.43371238945576E-5));
#27547=CARTESIAN_POINT('Ctrl Pts',(-0.0887899522119581,-0.127719015366539,
5.55111512312578E-17));
#27548=CARTESIAN_POINT('Ctrl Pts',(0.113598829883088,-0.159281402661362,
-0.0231499042268511));
#27549=CARTESIAN_POINT('Ctrl Pts',(0.166586312519255,-0.121492960388918,
-0.019443812294868));
#27550=CARTESIAN_POINT('Ctrl Pts',(0.23095150288242,0.0104442927835965,
-0.0120328160689595));
#27551=CARTESIAN_POINT('Ctrl Pts',(0.11621706131274,0.200096033890315,-0.000916915549125608));
#27552=CARTESIAN_POINT('Ctrl Pts',(-0.10499236225076,0.205957905231008,
0.0101977973326507));
#27553=CARTESIAN_POINT('Ctrl Pts',(-0.230035845505828,0.0235725168559611,
0.0213125102144268));
#27554=CARTESIAN_POINT('Ctrl Pts',(-0.144519469099591,-0.180546871179966,
0.032427223096203));
#27555=CARTESIAN_POINT('Ctrl Pts',(0.0733113434475644,-0.219303463105964,
0.0435419359779792));
#27556=CARTESIAN_POINT('Ctrl Pts',(0.224021882516666,-0.0573411296239388,
0.0546566488597554));
#27557=CARTESIAN_POINT('Ctrl Pts',(0.169655302903142,0.157136560254222,
0.0657713617415314));
#27558=CARTESIAN_POINT('Ctrl Pts',(-0.0400243713777188,0.227751714669903,
0.0768860746233078));
#27559=CARTESIAN_POINT('Ctrl Pts',(-0.213062639347379,0.0898775913551375,
0.0880007875050837));
#27560=CARTESIAN_POINT('Ctrl Pts',(-0.191053130847012,-0.13027828503737,
0.0991155003868603));
#27561=CARTESIAN_POINT('Ctrl Pts',(0.00585639141000308,-0.231169107852035,
0.110230213268636));
#27562=CARTESIAN_POINT('Ctrl Pts',(0.197404520979761,-0.120436912062476,
0.121344926150413));
#27563=CARTESIAN_POINT('Ctrl Pts',(0.20823862917329,0.100549809014636,0.132459639032189));
#27564=CARTESIAN_POINT('Ctrl Pts',(0.0284404998142444,0.229487890809628,
0.143574351913965));
#27565=CARTESIAN_POINT('Ctrl Pts',(-0.177393481894344,0.14834125742336,
0.154689064795741));
#27566=CARTESIAN_POINT('Ctrl Pts',(-0.220832491835081,-0.0686045495364922,
0.165803777677517));
#27567=CARTESIAN_POINT('Ctrl Pts',(-0.0621102407412604,-0.222746238913572,
0.176918490559294));
#27568=CARTESIAN_POINT('Ctrl Pts',(0.153470869196092,-0.172974751378497,
0.18803320344107));
#27569=CARTESIAN_POINT('Ctrl Pts',(0.228556969297201,0.035146599885103,
0.199147916322846));
#27570=CARTESIAN_POINT('Ctrl Pts',(0.0944104355434771,0.211092967147494,
0.210262629204622));
#27571=CARTESIAN_POINT('Ctrl Pts',(-0.126164195146967,0.193794136856338,
0.221377342086398));
#27572=CARTESIAN_POINT('Ctrl Pts',(-0.231241727855144,-0.000913669237423759,
0.232492054968175));
#27573=CARTESIAN_POINT('Ctrl Pts',(-0.124628863434608,-0.194785055445563,
0.243606767849951));
#27574=CARTESIAN_POINT('Ctrl Pts',(0.0960755786891363,-0.210340330602452,
0.254721480731727));
#27575=CARTESIAN_POINT('Ctrl Pts',(0.228827567011875,-0.0333394068786314,
0.265836193613503));
#27576=CARTESIAN_POINT('Ctrl Pts',(0.152099203503735,0.174182099430741,
0.27695090649528));
#27577=CARTESIAN_POINT('Ctrl Pts',(-0.0638684792613543,0.222248484439645,
0.288065619377055));
#27578=CARTESIAN_POINT('Ctrl Pts',(-0.221367719264692,0.0668573432203991,
0.299180332258832));
#27579=CARTESIAN_POINT('Ctrl Pts',(-0.176215730145938,-0.149738398293394,
0.310295045140607));
#27580=CARTESIAN_POINT('Ctrl Pts',(0.0302530689509243,-0.229256021283673,
0.321409758022384));
#27581=CARTESIAN_POINT('Ctrl Pts',(0.209026675506927,-0.0989010637032879,
0.33252447090416));
#27582=CARTESIAN_POINT('Ctrl Pts',(0.196446669842519,0.121992939889483,
0.343639183785936));
#27583=CARTESIAN_POINT('Ctrl Pts',(0.00402942669754128,0.231208423712843,
0.354753896667712));
#27584=CARTESIAN_POINT('Ctrl Pts',(-0.192076557857611,0.128763998838017,
0.365868609549488));
#27585=CARTESIAN_POINT('Ctrl Pts',(-0.212345926919954,-0.0915575163255094,
0.376983322431265));
#27586=CARTESIAN_POINT('Ctrl Pts',(-0.0382230727993462,-0.22806264091471,
0.38809803531304));
#27587=CARTESIAN_POINT('Ctrl Pts',(0.170891119305128,-0.155787665807794,
0.399212748194818));
#27588=CARTESIAN_POINT('Ctrl Pts',(0.223562920044702,0.0591032338902731,
0.410327461076593));
#27589=CARTESIAN_POINT('Ctrl Pts',(0.0715738936182804,0.219888037936411,
0.42144217395837));
#27590=CARTESIAN_POINT('Ctrl Pts',(-0.145937502387498,0.179376188141297,
0.432556886840145));
#27591=CARTESIAN_POINT('Ctrl Pts',(-0.22985031260278,-0.0253457150541741,
0.443671599721922));
#27592=CARTESIAN_POINT('Ctrl Pts',(-0.103346497859673,-0.206864866169546,
0.454786312603698));
#27593=CARTESIAN_POINT('Ctrl Pts',(0.117765938619279,-0.19900943489273,
0.465901025485474));
#27594=CARTESIAN_POINT('Ctrl Pts',(0.231069466514541,-0.00897068112737101,
0.477015738367251));
#27595=CARTESIAN_POINT('Ctrl Pts',(0.13284029417393,0.189280288775634,0.488130451249026));
#27596=CARTESIAN_POINT('Ctrl Pts',(-0.0869976157926483,0.2142544896183,
0.499245164130803));
#27597=CARTESIAN_POINT('Ctrl Pts',(-0.227193499228025,0.0430892722580614,
0.510359877012579));
#27598=CARTESIAN_POINT('Ctrl Pts',(-0.159404939315424,-0.167522048689269,
0.521474589894355));
#27599=CARTESIAN_POINT('Ctrl Pts',(0.0543109806804912,-0.224775196257787,
0.532589302776132));
#27600=CARTESIAN_POINT('Ctrl Pts',(0.218307876483828,-0.0762577375767544,
0.543704015657907));
#27601=CARTESIAN_POINT('Ctrl Pts',(0.182454678322123,0.142069918820186,
0.554818728539684));
#27602=CARTESIAN_POINT('Ctrl Pts',(-0.0204267791691959,0.230339571433083,
0.56593344142146));
#27603=CARTESIAN_POINT('Ctrl Pts',(-0.204608527780934,0.107744706758718,
0.577048154303235));
#27604=CARTESIAN_POINT('Ctrl Pts',(-0.201481260512532,-0.113485122978673,
0.588162867185013));
#27605=CARTESIAN_POINT('Ctrl Pts',(-0.0139078363112272,-0.230824919721298,
0.599277580066788));
#27606=CARTESIAN_POINT('Ctrl Pts',(0.186397526097791,-0.136855886756203,
0.610392292948565));
#27607=CARTESIAN_POINT('Ctrl Pts',(0.216065146500031,0.0823979607946937,
0.621507005830341));
#27608=CARTESIAN_POINT('Ctrl Pts',(0.0479357816258322,0.22622053910979,
0.632621718712117));
#27609=CARTESIAN_POINT('Ctrl Pts',(-0.164076427131555,0.162949371078709,
0.643736431593893));
#27610=CARTESIAN_POINT('Ctrl Pts',(-0.225884759107982,-0.0494939095034147,
0.65485114447567));
#27611=CARTESIAN_POINT('Ctrl Pts',(-0.0809067347692004,-0.216627956977371,
0.665965857357445));
#27612=CARTESIAN_POINT('Ctrl Pts',(0.13813741492639,-0.185449793940728,
0.677080570239222));
#27613=CARTESIAN_POINT('Ctrl Pts',(0.230723574201407,0.0154985090551028,
0.688195283120998));
#27614=CARTESIAN_POINT('Ctrl Pts',(0.112093680593801,0.202258691398264,
0.699309996002774));
#27615=CARTESIAN_POINT('Ctrl Pts',(-0.109152449131232,0.203861017175568,
0.71042470888455));
#27616=CARTESIAN_POINT('Ctrl Pts',(-0.230474895081132,0.0188386361646833,
0.721539421766327));
#27617=CARTESIAN_POINT('Ctrl Pts',(-0.14080894161815,-0.183429587132448,
0.732654134648102));
#27618=CARTESIAN_POINT('Ctrl Pts',(0.0777606531918726,-0.217777070166666,
0.743768847529879));
#27619=CARTESIAN_POINT('Ctrl Pts',(0.225144205164223,-0.052760386239807,
0.754883560411655));
#27620=CARTESIAN_POINT('Ctrl Pts',(0.166419341432716,0.160555829144583,
0.765998273293431));
#27621=CARTESIAN_POINT('Ctrl Pts',(-0.0446542215698074,0.226891101569008,
0.777112986175206));
#27622=CARTESIAN_POINT('Ctrl Pts',(-0.21484904707372,0.0855187607880183,
0.788227699056984));
#27623=CARTESIAN_POINT('Ctrl Pts',(-0.188360166347894,-0.134141787704641,
0.79934241193876));
#27624=CARTESIAN_POINT('Ctrl Pts',(0.0105631567361596,-0.231002145433697,
0.810457124820536));
#27625=CARTESIAN_POINT('Ctrl Pts',(0.199816430803703,-0.116391432056113,
0.821571837702312));
#27626=CARTESIAN_POINT('Ctrl Pts',(0.206147617427287,0.104769896937319,
0.832686550584088));
#27627=CARTESIAN_POINT('Ctrl Pts',(0.0237608275074776,0.230019552541438,
0.843801263465864));
#27628=CARTESIAN_POINT('Ctrl Pts',(-0.180377828110171,0.144697652370248,
0.85491597634764));
#27629=CARTESIAN_POINT('Ctrl Pts',(-0.219389478336887,-0.0730878120501113,
0.866030689229417));
#27630=CARTESIAN_POINT('Ctrl Pts',(-0.0575608814467432,-0.223964989233312,
0.877145402111192));
#27631=CARTESIAN_POINT('Ctrl Pts',(0.156961863502205,-0.169813264738413,
0.888260114992969));
#27632=CARTESIAN_POINT('Ctrl Pts',(0.227793763782214,0.0397941284253905,
0.899374827874745));
#27633=CARTESIAN_POINT('Ctrl Pts',(0.0900917081199666,0.212971959664249,
0.910489540756522));
#27634=CARTESIAN_POINT('Ctrl Pts',(-0.130084862998348,0.191184465618692,
0.921604253638297));
#27635=CARTESIAN_POINT('Ctrl Pts',(-0.23117515783393,-0.00562297747292118,
0.932718966520074));
#27636=CARTESIAN_POINT('Ctrl Pts',(-0.12063599724344,-0.197282862013618,
0.94383367940185));
#27637=CARTESIAN_POINT('Ctrl Pts',(0.100339469049717,-0.208340016381933,
0.954948392283626));
#27638=CARTESIAN_POINT('Ctrl Pts',(0.229459100175727,-0.0286721610931074,
0.966063105165402));
#27639=CARTESIAN_POINT('Ctrl Pts',(0.148520242025696,0.177243643563972,
0.977177818047179));
#27640=CARTESIAN_POINT('Ctrl Pts',(-0.0683815726727458,0.220901634204017,
0.988292530928954));
#27641=CARTESIAN_POINT('Ctrl Pts',(-0.222683430172034,0.0623350736104523,
0.999407243810731));
#27642=CARTESIAN_POINT('Ctrl Pts',(-0.173129590107263,-0.153296172504387,
1.01052195669251));
#27643=CARTESIAN_POINT('Ctrl Pts',(0.0349158509402568,-0.228592333266716,
1.02163666957428));
#27644=CARTESIAN_POINT('Ctrl Pts',(0.210997552503568,-0.0946234871092144,
1.03275138245606));
#27645=CARTESIAN_POINT('Ctrl Pts',(0.193921401160202,0.125968494661433,
1.04386609533784));
#27646=CARTESIAN_POINT('Ctrl Pts',(-0.000680228731668428,0.231242532342292,
1.05498080821961));
#27647=CARTESIAN_POINT('Ctrl Pts',(-0.194659142768612,0.124825436557587,
1.06609552110139));
#27648=CARTESIAN_POINT('Ctrl Pts',(-0.210437212200008,-0.0958631899985209,
1.07721023398317));
#27649=CARTESIAN_POINT('Ctrl Pts',(-0.0335703926366225,-0.228793794088533,
1.08832494686494));
#27650=CARTESIAN_POINT('Ctrl Pts',(0.174028465692067,-0.152274963812402,
1.09943965974672));
#27651=CARTESIAN_POINT('Ctrl Pts',(0.222312846772713,0.0636440856247927,
1.1105543726285));
#27652=CARTESIAN_POINT('Ctrl Pts',(0.0670807811141855,0.221300113602127,
1.12166908551027));
#27653=CARTESIAN_POINT('Ctrl Pts',(-0.149560431226741,0.176366802109906,
1.13278379839205));
#27654=CARTESIAN_POINT('Ctrl Pts',(-0.229286445107886,-0.0300216182940176,
1.14389851127382));
#27655=CARTESIAN_POINT('Ctrl Pts',(-0.099112026912242,-0.208926727817555,
1.1550132241556));
#27656=CARTESIAN_POINT('Ctrl Pts',(0.121794563711203,-0.196569722301278,
1.16612793703738));
#27657=CARTESIAN_POINT('Ctrl Pts',(0.231204238171301,-0.00426283084717903,
1.17724264991915));
#27658=CARTESIAN_POINT('Ctrl Pts',(0.128957835590708,0.191946472004472,
1.18835736280093));
#27659=CARTESIAN_POINT('Ctrl Pts',(-0.0913431052659731,0.212438246546079,
1.1994720756827));
#27660=CARTESIAN_POINT('Ctrl Pts',(-0.228023938298392,0.0384532838401966,
1.21058678856448));
#27661=CARTESIAN_POINT('Ctrl Pts',(-0.155960101971211,-0.170733763703413,
1.22170150144625));
#27662=CARTESIAN_POINT('Ctrl Pts',(0.0588775157502169,-0.223622471174715,
1.23281621432803));
#27663=CARTESIAN_POINT('Ctrl Pts',(0.219815671644481,-0.0717958353575546,
1.24393092720981));
#27664=CARTESIAN_POINT('Ctrl Pts',(0.17952342146866,0.145756346755087,1.25504564009158));
#27665=CARTESIAN_POINT('Ctrl Pts',(-0.0251136669571722,0.229875782124103,
1.26616035297336));
#27666=CARTESIAN_POINT('Ctrl Pts',(-0.206760431891084,0.103555276444112,
1.27727506585514));
#27667=CARTESIAN_POINT('Ctrl Pts',(-0.199128218864034,-0.117564977468804,
1.28838977873691));
#27668=CARTESIAN_POINT('Ctrl Pts',(-0.00920394248114851,-0.231060292819875,
1.29950449161869));
#27669=CARTESIAN_POINT('Ctrl Pts',(0.189146089304304,-0.133031306000099,
1.31061920450046));
#27670=CARTESIAN_POINT('Ctrl Pts',(0.214342205026698,0.0867812803517921,
1.32173391738224));
#27671=CARTESIAN_POINT('Ctrl Pts',(0.0433186034159268,0.227149884598909,
1.33284863026401));
#27672=CARTESIAN_POINT('Ctrl Pts',(-0.167361043146336,0.159573972539927,
1.34396334314579));
#27673=CARTESIAN_POINT('Ctrl Pts',(-0.224829908963541,-0.0540840411826741,
1.35507805602757));
#27674=CARTESIAN_POINT('Ctrl Pts',(-0.0764780817475084,-0.218230782630281,
1.36619276890935));
#27675=CARTESIAN_POINT('Ctrl Pts',(0.141885657405372,-0.182598005733494,
1.37730748179112));
#27676=CARTESIAN_POINT('Ctrl Pts',(0.230360075011687,0.0201942396691022,
1.3884221946729));
#27677=CARTESIAN_POINT('Ctrl Pts',(0.107951205315767,0.204499654635592,
1.39953690755467));
#27678=CARTESIAN_POINT('Ctrl Pts',(-0.113281668687639,0.201595721716874,
1.41065162043645));
#27679=CARTESIAN_POINT('Ctrl Pts',(-0.230810762065343,0.0141408482779098,
1.42176633331823));
#27680=CARTESIAN_POINT('Ctrl Pts',(-0.137043986371098,-0.186259274332104,
1.4328810462));
#27681=CARTESIAN_POINT('Ctrl Pts',(0.0821797998293032,-0.21614821760824,
1.44399575908178));
#27682=CARTESIAN_POINT('Ctrl Pts',(0.226172032398009,-0.0481641281054451,
1.45511047196355));
#27683=CARTESIAN_POINT('Ctrl Pts',(0.163114924122819,0.163911845220565,
1.46622518484533));
#27684=CARTESIAN_POINT('Ctrl Pts',(-0.0492658523502109,0.225934608387937,
1.47733989772711));
#27685=CARTESIAN_POINT('Ctrl Pts',(-0.216546170791042,0.0811253806828713,
1.48845461060888));
#27686=CARTESIAN_POINT('Ctrl Pts',(-0.185589149941156,-0.13795013192934,
1.49956932349066));
#27687=CARTESIAN_POINT('Ctrl Pts',(0.0152655844132623,-0.230739102467971,
1.51068403637244));
#27688=CARTESIAN_POINT('Ctrl Pts',(0.202145429136763,-0.112297804761793,
1.52179874925421));
#27689=CARTESIAN_POINT('Ctrl Pts',(0.203971103308708,0.108946594670196,
1.53291346213599));
#27690=CARTESIAN_POINT('Ctrl Pts',(0.0190712922670278,0.230455759933375,
1.54402817501776));
#27691=CARTESIAN_POINT('Ctrl Pts',(-0.183287346247982,0.140994043067697,
1.55514288789954));
#27692=CARTESIAN_POINT('Ctrl Pts',(-0.217855459014481,-0.077540766392869,
1.56625760078132));
#27693=CARTESIAN_POINT('Ctrl Pts',(-0.052987643695869,-0.225090828535423,
1.57737231366309));
#27694=CARTESIAN_POINT('Ctrl Pts',(0.160387746072949,-0.166581338645248,
1.58848702654487));
#27695=CARTESIAN_POINT('Ctrl Pts',(0.226936064644018,0.0444251509743055,
1.59960173942665));
#27696=CARTESIAN_POINT('Ctrl Pts',(0.085735608532081,0.214762605927655,
1.61071645230842));
#27697=CARTESIAN_POINT('Ctrl Pts',(-0.133951568706273,0.188495487257208,
1.6218311651902));
#27698=CARTESIAN_POINT('Ctrl Pts',(-0.231012691292417,-0.0103299533899106,
1.63294587807197));
#27699=CARTESIAN_POINT('Ctrl Pts',(-0.116593088558386,-0.199698831182409,
1.64406059095375));
#27700=CARTESIAN_POINT('Ctrl Pts',(0.104561736373614,-0.206253278184223,
1.65517530383553));
#27701=CARTESIAN_POINT('Ctrl Pts',(0.229995448645884,-0.0239930214308629,
1.6662900167173));
#27702=CARTESIAN_POINT('Ctrl Pts',(0.144879671070419,0.180231663105379,
1.67740472959908));
#27703=CARTESIAN_POINT('Ctrl Pts',(-0.0728662998970503,0.219463149103709,
1.68851944248086));
#27704=CARTESIAN_POINT('Ctrl Pts',(-0.223906767078497,0.0577869460316003,
1.69963415536263));
#27705=CARTESIAN_POINT('Ctrl Pts',(-0.169971632093058,-0.156790356077234,
1.71074886824441));
#27706=CARTESIAN_POINT('Ctrl Pts',(0.0395641490637797,-0.227833820105933,
1.72186358112618));
#27707=CARTESIAN_POINT('Ctrl Pts',(0.212880903058631,-0.0903066586035895,
1.73297829400796));
#27708=CARTESIAN_POINT('Ctrl Pts',(0.191315689600593,0.129891794921208,
1.74409300688973));
#27709=CARTESIAN_POINT('Ctrl Pts',(-0.00538960198695829,0.231180716465768,
1.75520771977151));
#27710=CARTESIAN_POINT('Ctrl Pts',(-0.197160978770901,0.12083509393096,
1.76632243265329));
#27711=CARTESIAN_POINT('Ctrl Pts',(-0.208441203479882,-0.100129097504481,
1.77743714553507));
#27712=CARTESIAN_POINT('Ctrl Pts',(-0.0289037867341024,-0.229430038546902,
1.78855185841684));
#27713=CARTESIAN_POINT('Ctrl Pts',(0.17709362123047,-0.148699094801151,
1.79966657129862));
#27714=CARTESIAN_POINT('Ctrl Pts',(0.220970553225224,0.0681585363879073,
1.81078128418039));
#27715=CARTESIAN_POINT('Ctrl Pts',(0.0625598420215454,0.222620389096423,
1.82189599706217));
#27716=CARTESIAN_POINT('Ctrl Pts',(-0.153121319098175,0.173284255236413,
1.83301070994394));
#27717=CARTESIAN_POINT('Ctrl Pts',(-0.228627464534992,-0.0346850679039896,
1.84412542282572));
#27718=CARTESIAN_POINT('Ctrl Pts',(-0.0948364421085485,-0.210901922047656,
1.8552401357075));
#27719=CARTESIAN_POINT('Ctrl Pts',(0.12577266572998,-0.194048468250533,
1.86635484858927));
#27720=CARTESIAN_POINT('Ctrl Pts',(0.231243101207172,0.000446787749336298,
1.87746956147105));
#27721=CARTESIAN_POINT('Ctrl Pts',(0.12502188245106,0.194533031600284,1.88858427435282));
#27722=CARTESIAN_POINT('Ctrl Pts',(-0.0956507036032086,0.210533879400477,
1.8996989872346));
#27723=CARTESIAN_POINT('Ctrl Pts',(-0.22875978800645,0.0338013441514916,
1.91081370011638));
#27724=CARTESIAN_POINT('Ctrl Pts',(-0.152450568934512,-0.173874654584121,
1.92192841299815));
#27725=CARTESIAN_POINT('Ctrl Pts',(0.0634196271269303,-0.22237698255504,
1.93304312587993));
#27726=CARTESIAN_POINT('Ctrl Pts',(0.221232282412995,-0.0673041506412468,
1.9441578387617));
#27727=CARTESIAN_POINT('Ctrl Pts',(0.176517694337723,0.149382311740377,
1.95527255164348));
#27728=CARTESIAN_POINT('Ctrl Pts',(-0.0297901370418169,0.229316635267117,
1.96638726452526));
#27729=CARTESIAN_POINT('Ctrl Pts',(-0.208826567210671,0.099322889115285,
1.97750197740704));
#27730=CARTESIAN_POINT('Ctrl Pts',(-0.196692574435429,-0.121596063411524,
1.98861669028881));
#27731=CARTESIAN_POINT('Ctrl Pts',(-0.00449623065254251,-0.231199817009248,
1.99973140317059));
#27732=CARTESIAN_POINT('Ctrl Pts',(0.191816190538262,-0.129151540922183,
2.01084611605236));
#27733=CARTESIAN_POINT('Ctrl Pts',(0.212530349676141,0.0911286011185604,
2.02196082893414));
#27734=CARTESIAN_POINT('Ctrl Pts',(0.0386834556929351,0.227985003302295,
2.03307554181592));
#27735=CARTESIAN_POINT('Ctrl Pts',(-0.170576234106037,0.15613237919574,
2.04419025469769));
#27736=CARTESIAN_POINT('Ctrl Pts',(-0.22368179441174,-0.0586517376086509,
2.05530496757947));
#27737=CARTESIAN_POINT('Ctrl Pts',(-0.0720177039274894,-0.219743081336705,
2.06641968046125));
#27738=CARTESIAN_POINT('Ctrl Pts',(0.145575042578183,-0.179670471845826,
2.07753439334302));
#27739=CARTESIAN_POINT('Ctrl Pts',(0.229901017386071,0.0248815932714643,
2.0886491062248));
#27740=CARTESIAN_POINT('Ctrl Pts',(0.103763949480942,0.206655786893781,
2.09976381910657));
#27741=CARTESIAN_POINT('Ctrl Pts',(-0.117363896480564,0.199246799920331,
2.11087853198835));
#27742=CARTESIAN_POINT('Ctrl Pts',(-0.231050883702757,0.00943719442296102,
2.12199324487013));
#27743=CARTESIAN_POINT('Ctrl Pts',(-0.133222182155807,-0.189011697012588,
2.1331079577519));
#27744=CARTESIAN_POINT('Ctrl Pts',(0.0865648562855566,-0.214429702115095,
2.14422267063368));
#27745=CARTESIAN_POINT('Ctrl Pts',(0.227106038835561,-0.0435478902060165,
2.15533738351545));
#27746=CARTESIAN_POINT('Ctrl Pts',(0.159742842467667,0.167199866623727,
2.16645209639723));
#27747=CARTESIAN_POINT('Ctrl Pts',(-0.0538570452843743,0.224884393346986,
2.17756680927901));
#27748=CARTESIAN_POINT('Ctrl Pts',(-0.218153468818653,0.0766983464531386,
2.18868152216078));
#27749=CARTESIAN_POINT('Ctrl Pts',(-0.182741142414774,-0.141701248491403,
2.19979623504256));
#27750=CARTESIAN_POINT('Ctrl Pts',(0.0199616707544952,-0.230380349352727,
2.21091094792433));
#27751=CARTESIAN_POINT('Ctrl Pts',(0.204390589890243,-0.10815758335346,
2.22202566080611));
#27752=CARTESIAN_POINT('Ctrl Pts',(0.20170994550457,0.113078078965284,2.23314037368789));
#27753=CARTESIAN_POINT('Ctrl Pts',(0.0143739066504459,0.230796407208724,
2.24425508656966));
#27754=CARTESIAN_POINT('Ctrl Pts',(-0.186120948441361,0.137231874000472,
2.25536979945144));
#27755=CARTESIAN_POINT('Ctrl Pts',(-0.216230848357744,-0.081961417532537,
2.26648451233322));
#27756=CARTESIAN_POINT('Ctrl Pts',(-0.048392844163279,-0.226123556916373,
2.27759922521499));
#27757=CARTESIAN_POINT('Ctrl Pts',(0.163747892690182,-0.16327981306027,
2.28871393809677));
#27758=CARTESIAN_POINT('Ctrl Pts',(0.225982712376694,0.0490367978780694,
2.29982865097855));
#27759=CARTESIAN_POINT('Ctrl Pts',(0.0813468259969867,0.216465965620237,
2.31094336386032));
#27760=CARTESIAN_POINT('Ctrl Pts',(-0.137768190986319,0.185724889406933,
2.3220580767421));
#27761=CARTESIAN_POINT('Ctrl Pts',(-0.230743965476533,-0.0150261240684335,
2.33317278962387));
#27762=CARTESIAN_POINT('Ctrl Pts',(-0.112521659700458,-0.202044365771375,
2.34428750250565));
#27763=CARTESIAN_POINT('Ctrl Pts',(0.108778414904377,-0.204057369921787,
2.35540221538743));
#27764=CARTESIAN_POINT('Ctrl Pts',(0.23036421697438,-0.0193489636911256,
2.3665169282692));
#27765=CARTESIAN_POINT('Ctrl Pts',(0.141318813665082,0.183231604869622,
2.37763164115098));
#27766=CARTESIAN_POINT('Ctrl Pts',(-0.0776082748673582,0.217759953254891,
2.38874635403276));
#27767=CARTESIAN_POINT('Ctrl Pts',(-0.175417824731111,0.108336165866313,
2.3961561626206));
#27768=CARTESIAN_POINT('Ctrl Pts',(-0.190389869545322,0.0450217421539731,
2.39986106691453));
#27769=CARTESIAN_POINT('Ctrl Pts',(0.10578567459061,-0.148326269272423,
-0.0153811560512364));
#27770=CARTESIAN_POINT('Ctrl Pts',(0.155128758505242,-0.113136858768523,
-0.0116750641192532));
#27771=CARTESIAN_POINT('Ctrl Pts',(0.215067008659125,0.00972595016050153,
-0.00426406789334474));
#27772=CARTESIAN_POINT('Ctrl Pts',(0.108223828032029,0.1863337320444,0.00685183262648915));
#27773=CARTESIAN_POINT('Ctrl Pts',(-0.0977711467537901,0.19179243276145,
0.0179665455082654));
#27774=CARTESIAN_POINT('Ctrl Pts',(-0.214214328808668,0.0219512348848415,
0.0290812583900415));
#27775=CARTESIAN_POINT('Ctrl Pts',(-0.134579639120505,-0.168129131106836,
0.0401959712718177));
#27776=CARTESIAN_POINT('Ctrl Pts',(0.0682691003923698,-0.204220103398932,
0.051310684153594));
#27777=CARTESIAN_POINT('Ctrl Pts',(0.208613997076146,-0.0533972936631411,
0.06242539703537));
#27778=CARTESIAN_POINT('Ctrl Pts',(0.157986668383419,0.146328945874253,
0.0735401099171463));
#27779=CARTESIAN_POINT('Ctrl Pts',(-0.0372715557951986,0.212087297028674,
0.0846548227989223));
#27780=CARTESIAN_POINT('Ctrl Pts',(-0.198408514036763,0.0836959468849107,
0.0957695356806986));
#27781=CARTESIAN_POINT('Ctrl Pts',(-0.177912786162498,-0.121317942107057,
0.106884248562475));
#27782=CARTESIAN_POINT('Ctrl Pts',(0.00545359768767935,-0.215269647088839,
0.117998961444251));
#27783=CARTESIAN_POINT('Ctrl Pts',(0.183827337311238,-0.112153443844903,
0.129113674326027));
#27784=CARTESIAN_POINT('Ctrl Pts',(0.193916291968782,0.0936341455939032,
0.140228387207803));
#27785=CARTESIAN_POINT('Ctrl Pts',(0.0264844053555898,0.21370406160572,
0.15134310008958));
#27786=CARTESIAN_POINT('Ctrl Pts',(-0.165192627155433,0.138138570637568,
0.162457812971356));
#27787=CARTESIAN_POINT('Ctrl Pts',(-0.205643967850216,-0.0638860326305435,
0.173572525853132));
#27788=CARTESIAN_POINT('Ctrl Pts',(-0.0578383925482501,-0.207426090306074,
0.184687238734908));
#27789=CARTESIAN_POINT('Ctrl Pts',(0.142915375489557,-0.161077810225246,
0.195801951616684));
#27790=CARTESIAN_POINT('Ctrl Pts',(0.21283716746355,0.0327292700306685,
0.20691666449846));
#27791=CARTESIAN_POINT('Ctrl Pts',(0.0879170289222095,0.196574312904571,
0.218031377380237));
#27792=CARTESIAN_POINT('Ctrl Pts',(-0.117486813081955,0.180465269934133,
0.229146090262013));
#27793=CARTESIAN_POINT('Ctrl Pts',(-0.215337272398233,-0.000850828452481674,
0.240260803143789));
#27794=CARTESIAN_POINT('Ctrl Pts',(-0.116057079157066,-0.181388034645117,
0.251375516025565));
#27795=CARTESIAN_POINT('Ctrl Pts',(0.0894676460468228,-0.19587344156003,
0.262490228907341));
#27796=CARTESIAN_POINT('Ctrl Pts',(0.213089153877661,-0.0310463730193083,
0.273604941789118));
#27797=CARTESIAN_POINT('Ctrl Pts',(0.141638050883947,0.162202118708908,
0.284719654670894));
#27798=CARTESIAN_POINT('Ctrl Pts',(-0.059475702088586,0.206962570630221,
0.29583436755267));
#27799=CARTESIAN_POINT('Ctrl Pts',(-0.206142383148674,0.0622589965159431,
0.306949080434446));
#27800=CARTESIAN_POINT('Ctrl Pts',(-0.1640958793867,-0.139439618276758,
0.318063793316222));
#27801=CARTESIAN_POINT('Ctrl Pts',(0.0281723087350732,-0.213488139714225,
0.329178506197999));
#27802=CARTESIAN_POINT('Ctrl Pts',(0.194650137670344,-0.0920987984854177,
0.340293219079775));
#27803=CARTESIAN_POINT('Ctrl Pts',(0.182935365723024,0.113602450437052,
0.351407931961551));
#27804=CARTESIAN_POINT('Ctrl Pts',(0.00375228883829077,0.215306258864348,
0.362522644843327));
#27805=CARTESIAN_POINT('Ctrl Pts',(-0.178865823414919,0.119907806216696,
0.373637357725103));
#27806=CARTESIAN_POINT('Ctrl Pts',(-0.197741096003495,-0.0852603291627437,
0.384752070606879));
#27807=CARTESIAN_POINT('Ctrl Pts',(-0.035594147802109,-0.212376838237756,
0.395866783488655));
#27808=CARTESIAN_POINT('Ctrl Pts',(0.159137487206888,-0.1450728263428,0.406981496370432));
#27809=CARTESIAN_POINT('Ctrl Pts',(0.208186601347174,0.0550382030695517,
0.418096209252208));
#27810=CARTESIAN_POINT('Ctrl Pts',(0.0666511497282075,0.204764472058811,
0.429210922133984));
#27811=CARTESIAN_POINT('Ctrl Pts',(-0.13590014222874,0.167038965872701,
0.44032563501576));
#27812=CARTESIAN_POINT('Ctrl Pts',(-0.214041556577407,-0.0236024751993154,
0.451440347897537));
#27813=CARTESIAN_POINT('Ctrl Pts',(-0.0962384824202376,-0.192637014301674,
0.462555060779312));
#27814=CARTESIAN_POINT('Ctrl Pts',(0.109666175905667,-0.185321867678483,
0.473669773661089));
#27815=CARTESIAN_POINT('Ctrl Pts',(0.215176858931472,-0.0083536912798596,
0.484784486542865));
#27816=CARTESIAN_POINT('Ctrl Pts',(0.123703740139465,0.176261877480984,
0.495899199424641));
#27817=CARTESIAN_POINT('Ctrl Pts',(-0.0810140516752797,0.199518390653015,
0.507013912306417));
#27818=CARTESIAN_POINT('Ctrl Pts',(-0.211567474798578,0.0401256574396861,
0.518128625188193));
#27819=CARTESIAN_POINT('Ctrl Pts',(-0.148441309262714,-0.156000136160149,
0.52924333806997));
#27820=CARTESIAN_POINT('Ctrl Pts',(0.0505755537700164,-0.209315499040252,
0.540358050951745));
#27821=CARTESIAN_POINT('Ctrl Pts',(0.203292991715257,-0.0710128460003809,
0.551472763833522));
#27822=CARTESIAN_POINT('Ctrl Pts',(0.16990572216618,0.132298565195555,0.562587476715298));
#27823=CARTESIAN_POINT('Ctrl Pts',(-0.0190218562669204,0.214497164927125,
0.573702189597074));
#27824=CARTESIAN_POINT('Ctrl Pts',(-0.190535863446603,0.10033418917932,
0.584816902478851));
#27825=CARTESIAN_POINT('Ctrl Pts',(-0.187623684879683,-0.105679788274689,
0.595931615360627));
#27826=CARTESIAN_POINT('Ctrl Pts',(-0.012951276415378,-0.214949131695911,
0.607046328242403));
#27827=CARTESIAN_POINT('Ctrl Pts',(0.173577386849575,-0.127443146351959,
0.61816104112418));
#27828=CARTESIAN_POINT('Ctrl Pts',(0.201204513299551,0.0767307539745598,
0.629275754005954));
#27829=CARTESIAN_POINT('Ctrl Pts',(0.0446388312409215,0.210661433402173,
0.640390466887733));
#27830=CARTESIAN_POINT('Ctrl Pts',(-0.152791499229278,0.151741960383025,
0.651505179769506));
#27831=CARTESIAN_POINT('Ctrl Pts',(-0.210348747839816,-0.0460897934453505,
0.662619892651285));
#27832=CARTESIAN_POINT('Ctrl Pts',(-0.0753420922142629,-0.201728614525534,
0.673734605533059));
#27833=CARTESIAN_POINT('Ctrl Pts',(0.128636532957515,-0.172694838273424,
0.684849318414837));
#27834=CARTESIAN_POINT('Ctrl Pts',(0.214854756567229,0.0144325450995374,
0.695964031296612));
#27835=CARTESIAN_POINT('Ctrl Pts',(0.104384047187493,0.188347645247752,
0.707078744178388));
#27836=CARTESIAN_POINT('Ctrl Pts',(-0.10164510916572,0.189839765487378,
0.718193457060165));
#27837=CARTESIAN_POINT('Ctrl Pts',(-0.214623181219824,0.0175429433304858,
0.729308169941941));
#27838=CARTESIAN_POINT('Ctrl Pts',(-0.131124316093717,-0.170813578226583,
0.740422882823717));
#27839=CARTESIAN_POINT('Ctrl Pts',(0.0724123933580511,-0.202798693451838,
0.751537595705493));
#27840=CARTESIAN_POINT('Ctrl Pts',(0.209659128073555,-0.0491316068641172,
0.76265230858727));
#27841=CARTESIAN_POINT('Ctrl Pts',(0.154973271436896,0.149513042634279,
0.773767021469046));
#27842=CARTESIAN_POINT('Ctrl Pts',(-0.0415829719103787,0.211285875592086,
0.784881734350822));
#27843=CARTESIAN_POINT('Ctrl Pts',(-0.200072055348054,0.0796369100757868,
0.795996447232598));
#27844=CARTESIAN_POINT('Ctrl Pts',(-0.175405039678833,-0.12491571891832,
0.807111160114375));
#27845=CARTESIAN_POINT('Ctrl Pts',(0.00983663883061682,-0.215114168092504,
0.81822587299615));
#27846=CARTESIAN_POINT('Ctrl Pts',(0.186073359634179,-0.108386205820036,
0.829340585877927));
#27847=CARTESIAN_POINT('Ctrl Pts',(0.191969096840493,0.0975639822673277,
0.840455298759702));
#27848=CARTESIAN_POINT('Ctrl Pts',(0.0221265938152439,0.214199156449667,
0.85157001164148));
#27849=CARTESIAN_POINT('Ctrl Pts',(-0.167971714563094,0.13474556721595,
0.862684724523254));
#27850=CARTESIAN_POINT('Ctrl Pts',(-0.204300202632679,-0.0680609431455381,
0.873799437405031));
#27851=CARTESIAN_POINT('Ctrl Pts',(-0.0536019312887383,-0.208561016826566,
0.884914150286807));
#27852=CARTESIAN_POINT('Ctrl Pts',(0.146166264499983,-0.158133765843145,
0.896028863168584));
#27853=CARTESIAN_POINT('Ctrl Pts',(0.212126454066791,0.0370571486040605,
0.907143576050359));
#27854=CARTESIAN_POINT('Ctrl Pts',(0.0838953370232766,0.198324071164759,
0.918258288932136));
#27855=CARTESIAN_POINT('Ctrl Pts',(-0.121137823342632,0.178035087927698,
0.929373001813913));
#27856=CARTESIAN_POINT('Ctrl Pts',(-0.215275280962153,-0.00523623760731131,
0.940487714695687));
#27857=CARTESIAN_POINT('Ctrl Pts',(-0.112338836248953,-0.183714045864339,
0.951602427577466));
#27858=CARTESIAN_POINT('Ctrl Pts',(0.093438272492876,-0.194010705918928,
0.962717140459239));
#27859=CARTESIAN_POINT('Ctrl Pts',(0.21367725114797,-0.0267001333229138,
0.973831853341018));
#27860=CARTESIAN_POINT('Ctrl Pts',(0.138305244950313,0.165053094478255,
0.984946566222792));
#27861=CARTESIAN_POINT('Ctrl Pts',(-0.0636783917774306,0.205708354711845,
0.996061279104569));
#27862=CARTESIAN_POINT('Ctrl Pts',(-0.207367601454554,0.0580477617535676,
1.00717599198635));
#27863=CARTESIAN_POINT('Ctrl Pts',(-0.161221999380996,-0.14275269417145,
1.01829070486812));
#27864=CARTESIAN_POINT('Ctrl Pts',(0.0325143916484108,-0.212870099152858,
1.0294054177499));
#27865=CARTESIAN_POINT('Ctrl Pts',(0.196485460735197,-0.0881154271242621,
1.04052013063168));
#27866=CARTESIAN_POINT('Ctrl Pts',(0.180583781192123,0.117304572579115,
1.05163484351345));
#27867=CARTESIAN_POINT('Ctrl Pts',(-0.000633443630793526,0.215338021553975,
1.06274955639523));
#27868=CARTESIAN_POINT('Ctrl Pts',(-0.181270782051193,0.116240132278671,
1.07386426927701));
#27869=CARTESIAN_POINT('Ctrl Pts',(-0.195963659788188,-0.0892698651283455,
1.08497898215878));
#27870=CARTESIAN_POINT('Ctrl Pts',(-0.0312614719270617,-0.213057703804784,
1.09609369504056));
#27871=CARTESIAN_POINT('Ctrl Pts',(0.162059051665856,-0.141801722665054,
1.10720840792233));
#27872=CARTESIAN_POINT('Ctrl Pts',(0.2070225062196,0.059266741906144,1.11832312080411));
#27873=CARTESIAN_POINT('Ctrl Pts',(0.0624670666901483,0.206079427301083,
1.12943783368589));
#27874=CARTESIAN_POINT('Ctrl Pts',(-0.139273891515134,0.164236560850027,
1.14055254656766));
#27875=CARTESIAN_POINT('Ctrl Pts',(-0.213516471033934,-0.0279567769034468,
1.15166725944944));
#27876=CARTESIAN_POINT('Ctrl Pts',(-0.0922952519647008,-0.194557064231516,
1.16278197233121));
#27877=CARTESIAN_POINT('Ctrl Pts',(0.113417718271556,-0.183049954820229,
1.17389668521299));
#27878=CARTESIAN_POINT('Ctrl Pts',(0.215302361198007,-0.00396963980438003,
1.18501139809477));
#27879=CARTESIAN_POINT('Ctrl Pts',(0.120088311171413,0.178744684669536,
1.19612611097654));
#27880=CARTESIAN_POINT('Ctrl Pts',(-0.0850606649708146,0.1978270660257,
1.20724082385832));
#27881=CARTESIAN_POINT('Ctrl Pts',(-0.212340797528712,0.0358085252765923,
1.2183555367401));
#27882=CARTESIAN_POINT('Ctrl Pts',(-0.145233402608328,-0.158990954284894,
1.22947024962187));
#27883=CARTESIAN_POINT('Ctrl Pts',(0.0548280094809581,-0.208242056640751,
1.24058496250365));
#27884=CARTESIAN_POINT('Ctrl Pts',(0.204697083010726,-0.0668578266511397,
1.25169967538542));
#27885=CARTESIAN_POINT('Ctrl Pts',(0.167176072715028,0.135731446206079,
1.2628143882672));
#27886=CARTESIAN_POINT('Ctrl Pts',(-0.0233863870186178,0.214065274343667,
1.27392910114898));
#27887=CARTESIAN_POINT('Ctrl Pts',(-0.192539762854552,0.0964329015301672,
1.28504381403075));
#27888=CARTESIAN_POINT('Ctrl Pts',(-0.185432481868328,-0.109479036558445,
1.29615852691253));
#27889=CARTESIAN_POINT('Ctrl Pts',(-0.00857090927137133,-0.215168316189618,
1.3072732397943));
#27890=CARTESIAN_POINT('Ctrl Pts',(0.176136908045833,-0.123881614461822,
1.31838795267608));
#27891=CARTESIAN_POINT('Ctrl Pts',(0.199600073128609,0.0808125954580599,
1.32950266555786));
#27892=CARTESIAN_POINT('Ctrl Pts',(0.0403392155482017,0.211526859917528,
1.34061737843963));
#27893=CARTESIAN_POINT('Ctrl Pts',(-0.15585020433436,0.148598716638307,
1.35173209132141));
#27894=CARTESIAN_POINT('Ctrl Pts',(-0.209366448689055,-0.0503642228267966,
1.36284680420318));
#27895=CARTESIAN_POINT('Ctrl Pts',(-0.0712180352331336,-0.203221200260076,
1.37396151708496));
#27896=CARTESIAN_POINT('Ctrl Pts',(0.132126977001494,-0.170039191735495,
1.38507622996674));
#27897=CARTESIAN_POINT('Ctrl Pts',(0.214516258300679,0.0188053104810904,
1.39619094284852));
#27898=CARTESIAN_POINT('Ctrl Pts',(0.100526485078686,0.190434478431135,
1.40730565573029));
#27899=CARTESIAN_POINT('Ctrl Pts',(-0.105490327261336,0.187730273615925,
1.41842036861207));
#27900=CARTESIAN_POINT('Ctrl Pts',(-0.21493594778207,0.013168262172261,
1.42953508149384));
#27901=CARTESIAN_POINT('Ctrl Pts',(-0.127618308760518,-0.173448643830728,
1.44064979437562));
#27902=CARTESIAN_POINT('Ctrl Pts',(0.0765275977896153,-0.201281870902883,
1.45176450725739));
#27903=CARTESIAN_POINT('Ctrl Pts',(0.210616262908487,-0.044851472395862,
1.46287922013917));
#27904=CARTESIAN_POINT('Ctrl Pts',(0.151896126939755,0.152638237012603,
1.47399393302095));
#27905=CARTESIAN_POINT('Ctrl Pts',(-0.0458774217173872,0.210395168561873,
1.48510864590272));
#27906=CARTESIAN_POINT('Ctrl Pts',(-0.201652453469104,0.0755456999934797,
1.4962233587845));
#27907=CARTESIAN_POINT('Ctrl Pts',(-0.172824609579421,-0.128462131001064,
1.50733807166628));
#27908=CARTESIAN_POINT('Ctrl Pts',(0.0142156406614265,-0.214869216823162,
1.51845278454805));
#27909=CARTESIAN_POINT('Ctrl Pts',(0.18824217299288,-0.104574132004682,
1.52956749742983));
#27910=CARTESIAN_POINT('Ctrl Pts',(0.189942280063182,0.101453413062418,
1.5406822103116));
#27911=CARTESIAN_POINT('Ctrl Pts',(0.0177595976988407,0.214605362158519,
1.55179692319338));
#27912=CARTESIAN_POINT('Ctrl Pts',(-0.170681120454501,0.131296686546196,
1.56291163607516));
#27913=CARTESIAN_POINT('Ctrl Pts',(-0.202871690833546,-0.0722076300397131,
1.57402634895693));
#27914=CARTESIAN_POINT('Ctrl Pts',(-0.0493432338968959,-0.20960942260836,
1.58514106183871));
#27915=CARTESIAN_POINT('Ctrl Pts',(0.149356520061482,-0.155124126726753,
1.59625577472049));
#27916=CARTESIAN_POINT('Ctrl Pts',(0.211327746174964,0.0413696564431422,
1.60737048760226));
#27917=CARTESIAN_POINT('Ctrl Pts',(0.0798388433607749,0.199991559492963,
1.61848520048404));
#27918=CARTESIAN_POINT('Ctrl Pts',(-0.124738582894269,0.175531053421164,
1.62959991336581));
#27919=CARTESIAN_POINT('Ctrl Pts',(-0.215123988623049,-0.00961947485696401,
1.64071462624759));
#27920=CARTESIAN_POINT('Ctrl Pts',(-0.108573992693813,-0.185963848336544,
1.65182933912937));
#27921=CARTESIAN_POINT('Ctrl Pts',(0.0973701386716032,-0.192067490410758,
1.66294405201114));
#27922=CARTESIAN_POINT('Ctrl Pts',(0.214176710383506,-0.0223428177926071,
1.67405876489292));
#27923=CARTESIAN_POINT('Ctrl Pts',(0.134915066945881,0.167835602565731,
1.68517347777469));
#27924=CARTESIAN_POINT('Ctrl Pts',(-0.0678546662625307,0.204368806435851,
1.69628819065647));
#27925=CARTESIAN_POINT('Ctrl Pts',(-0.208506799103289,0.0538124474941849,
1.70740290353825));
#27926=CARTESIAN_POINT('Ctrl Pts',(-0.158281240931237,-0.146006553095679,
1.71851761642002));
#27927=CARTESIAN_POINT('Ctrl Pts',(0.0368429868742704,-0.212163755377294,
1.7296323293018));
#27928=CARTESIAN_POINT('Ctrl Pts',(0.198239277294426,-0.0840955035385219,
1.74074704218357));
#27929=CARTESIAN_POINT('Ctrl Pts',(0.178157286523072,0.120958034195128,
1.75186175506535));
#27930=CARTESIAN_POINT('Ctrl Pts',(-0.00501891333345269,0.215280457279719,
1.76297646794713));
#27931=CARTESIAN_POINT('Ctrl Pts',(-0.183600545566271,0.112524239368154,
1.7740911808289));
#27932=CARTESIAN_POINT('Ctrl Pts',(-0.194104933521689,-0.0932423699835773,
1.78520589371068));
#27933=CARTESIAN_POINT('Ctrl Pts',(-0.0269158281034883,-0.213650188333915,
1.79632060659246));
#27934=CARTESIAN_POINT('Ctrl Pts',(0.164913390453403,-0.138471796503031,
1.80743531947423));
#27935=CARTESIAN_POINT('Ctrl Pts',(0.205772533587259,0.0634706955901187,
1.81855003235601));
#27936=CARTESIAN_POINT('Ctrl Pts',(0.0582570709341164,0.207308896248547,
1.82966474523779));
#27937=CARTESIAN_POINT('Ctrl Pts',(-0.142589866917423,0.161366026877052,
1.84077945811956));
#27938=CARTESIAN_POINT('Ctrl Pts',(-0.212902814145765,-0.0322994815194884,
1.85189417100134));
#27939=CARTESIAN_POINT('Ctrl Pts',(-0.0883137354016025,-0.196396407597057,
1.86300888388311));
#27940=CARTESIAN_POINT('Ctrl Pts',(0.117122212464671,-0.180702108800628,
1.87412359676489));
#27941=CARTESIAN_POINT('Ctrl Pts',(0.215338551293191,0.000416058365307058,
1.88523830964666));
#27942=CARTESIAN_POINT('Ctrl Pts',(0.116423066921421,0.181153344617824,
1.89635302252844));
#27943=CARTESIAN_POINT('Ctrl Pts',(-0.089071993225153,0.196053678365167,
1.90746773541022));
#27944=CARTESIAN_POINT('Ctrl Pts',(-0.213026036609469,0.0314765389468832,
1.91858244829199));
#27945=CARTESIAN_POINT('Ctrl Pts',(-0.141965249933099,-0.161915819452723,
1.92969716117377));
#27946=CARTESIAN_POINT('Ctrl Pts',(0.059057721323464,-0.207082230840055,
1.94081187405555));
#27947=CARTESIAN_POINT('Ctrl Pts',(0.206016261438301,-0.0626750731997882,
1.95192658693732));
#27948=CARTESIAN_POINT('Ctrl Pts',(0.164377074939183,0.139108022816996,
1.9630412998191));
#27949=CARTESIAN_POINT('Ctrl Pts',(-0.0277412165808244,0.213544584759783,
1.97415601270088));
#27950=CARTESIAN_POINT('Ctrl Pts',(-0.19446379251932,0.0924916113851058,
1.98527072558265));
#27951=CARTESIAN_POINT('Ctrl Pts',(-0.183164357370848,-0.113232870521543,
1.99638543846443));
#27952=CARTESIAN_POINT('Ctrl Pts',(-0.00418698672498783,-0.215298244116777,
2.0075001513462));
#27953=CARTESIAN_POINT('Ctrl Pts',(0.178623363765053,-0.120268693743865,
2.01861486422798));
#27954=CARTESIAN_POINT('Ctrl Pts',(0.197912834442113,0.0848609140934513,
2.02972957710976));
#27955=CARTESIAN_POINT('Ctrl Pts',(0.0360228662582626,0.212304540422618,
2.04084428999153));
#27956=CARTESIAN_POINT('Ctrl Pts',(-0.158844259334395,0.145393830866544,
2.05195900287331));
#27957=CARTESIAN_POINT('Ctrl Pts',(-0.208297299715472,-0.0546177600176673,
2.06307371575508));
#27958=CARTESIAN_POINT('Ctrl Pts',(-0.0670644354372087,-0.204629485354265,
2.07418842863686));
#27959=CARTESIAN_POINT('Ctrl Pts',(0.135562611855587,-0.167313009190196,
2.08530314151863));
#27960=CARTESIAN_POINT('Ctrl Pts',(0.214088773962576,0.0231702750091667,
2.09641785440042));
#27961=CARTESIAN_POINT('Ctrl Pts',(0.0966272223518926,0.192442315181511,
2.10753256728219));
#27962=CARTESIAN_POINT('Ctrl Pts',(-0.109291785615718,0.185542907099355,
2.11864728016397));
#27963=CARTESIAN_POINT('Ctrl Pts',(-0.215159554217309,0.00878811849825859,
2.12976199304574));
#27964=CARTESIAN_POINT('Ctrl Pts',(-0.124059362444929,-0.176011759052189,
2.14087670592752));
#27965=CARTESIAN_POINT('Ctrl Pts',(0.0806110567109805,-0.19968155229992,
2.1519914188093));
#27966=CARTESIAN_POINT('Ctrl Pts',(0.211486029799309,-0.0405527323404903,
2.16310613169107));
#27967=CARTESIAN_POINT('Ctrl Pts',(0.148755971948441,0.155700113288616,
2.17422084457285));
#27968=CARTESIAN_POINT('Ctrl Pts',(-0.0501528393622344,0.20941718571921,
2.18533555745462));
#27969=CARTESIAN_POINT('Ctrl Pts',(-0.203149203975196,0.0714231504662535,
2.1964502703364));
#27970=CARTESIAN_POINT('Ctrl Pts',(-0.170172483692846,-0.131955251453046,
2.20756498321817));
#27971=CARTESIAN_POINT('Ctrl Pts',(0.0185887373038336,-0.21453513820328,
2.21867969609995));
#27972=CARTESIAN_POINT('Ctrl Pts',(0.190332914993618,-0.100718668747836,
2.22979440898173));
#27973=CARTESIAN_POINT('Ctrl Pts',(0.187836641264677,0.105300740131422,
2.2409091218635));
#27974=CARTESIAN_POINT('Ctrl Pts',(0.0133852911432732,0.214922580230725,
2.25202383474528));
#27975=CARTESIAN_POINT('Ctrl Pts',(-0.173319831785035,0.1277932737636,2.26313854762705));
#27976=CARTESIAN_POINT('Ctrl Pts',(-0.201358818434712,-0.0763242354961321,
2.27425326050883));
#27977=CARTESIAN_POINT('Ctrl Pts',(-0.0450644577099939,-0.210571121496985,
2.28536797339061));
#27978=CARTESIAN_POINT('Ctrl Pts',(0.152485560888693,-0.152049675066076,
2.29648268627238));
#27979=CARTESIAN_POINT('Ctrl Pts',(0.210439964031213,0.0456641212645707,
2.30759739915416));
#27980=CARTESIAN_POINT('Ctrl Pts',(0.075751914634623,0.201577764688349,
2.31871211203594));
#27981=CARTESIAN_POINT('Ctrl Pts',(-0.128292703680264,0.172951013090535,
2.32982682491771));
#27982=CARTESIAN_POINT('Ctrl Pts',(-0.214873745361368,-0.0139926500360693,
2.34094153779949));
#27983=CARTESIAN_POINT('Ctrl Pts',(-0.104782590540052,-0.188148060612542,
2.35205625068127));
#27984=CARTESIAN_POINT('Ctrl Pts',(0.101296800445916,-0.190022613389401,
2.36317096356304));
#27985=CARTESIAN_POINT('Ctrl Pts',(0.214520115385455,-0.0180181713033658,
2.37428567644482));
#27986=CARTESIAN_POINT('Ctrl Pts',(0.131599119914276,0.170629212883634,
2.3854003893266));
#27987=CARTESIAN_POINT('Ctrl Pts',(-0.0722704953836764,0.202782753815304,
2.39651510220837));
#27988=CARTESIAN_POINT('Ctrl Pts',(-0.163352852696599,0.100884968626203,
2.40392491079622));
#27989=CARTESIAN_POINT('Ctrl Pts',(-0.177295142967567,0.0419252149859687,
2.40762981509015));
#27990=CARTESIAN_POINT('Ctrl Pts',(0.0979725192981311,-0.137371135883486,
-0.00761240787562157));
#27991=CARTESIAN_POINT('Ctrl Pts',(0.143671204491229,-0.104780757148129,
-0.00390631594363848));
#27992=CARTESIAN_POINT('Ctrl Pts',(0.199182514435829,0.00900760753740661,
0.00350468028227001));
#27993=CARTESIAN_POINT('Ctrl Pts',(0.100230594751318,0.172571430198485,
0.0146205808021039));
#27994=CARTESIAN_POINT('Ctrl Pts',(-0.0905499312568196,0.177626960291894,
0.0257352936838801));
#27995=CARTESIAN_POINT('Ctrl Pts',(-0.198392812111508,0.0203299529137219,
0.0368500065656563));
#27996=CARTESIAN_POINT('Ctrl Pts',(-0.124639809141419,-0.155711391033705,
0.0479647194474324));
#27997=CARTESIAN_POINT('Ctrl Pts',(0.0632268573371749,-0.1891367436919,
0.0590794323292087));
#27998=CARTESIAN_POINT('Ctrl Pts',(0.193206111635628,-0.0494534577023437,
0.0701941452109847));
#27999=CARTESIAN_POINT('Ctrl Pts',(0.146318033863695,0.135521331494285,
0.0813088580927611));
#28000=CARTESIAN_POINT('Ctrl Pts',(-0.034518740212678,0.196422879387445,
0.092423570974537));
#28001=CARTESIAN_POINT('Ctrl Pts',(-0.183754388726148,0.0775143024146838,
0.103538283856313));
#28002=CARTESIAN_POINT('Ctrl Pts',(-0.164772441477984,-0.112357599176744,
0.114652996738089));
#28003=CARTESIAN_POINT('Ctrl Pts',(0.00505080396535491,-0.199370186325643,
0.125767709619866));
#28004=CARTESIAN_POINT('Ctrl Pts',(0.170250153642716,-0.10386997562733,
0.136882422501642));
#28005=CARTESIAN_POINT('Ctrl Pts',(0.179593954764274,0.0867184821731703,
0.147997135383418));
#28006=CARTESIAN_POINT('Ctrl Pts',(0.0245283108969357,0.197920232401811,
0.159111848265194));
#28007=CARTESIAN_POINT('Ctrl Pts',(-0.152991772416522,0.127935883851777,
0.170226561146971));
#28008=CARTESIAN_POINT('Ctrl Pts',(-0.190455443865352,-0.0591675157245945,
0.181341274028746));
#28009=CARTESIAN_POINT('Ctrl Pts',(-0.0535665443552399,-0.192105941698575,
0.192455986910523));
#28010=CARTESIAN_POINT('Ctrl Pts',(0.132359881783023,-0.149180869071993,
0.203570699792299));
#28011=CARTESIAN_POINT('Ctrl Pts',(0.1971173656299,0.0303119401762338,0.214685412674075));
#28012=CARTESIAN_POINT('Ctrl Pts',(0.0814236223009415,0.18205565866165,
0.225800125555851));
#28013=CARTESIAN_POINT('Ctrl Pts',(-0.108809431016943,0.16713640301193,
0.236914838437627));
#28014=CARTESIAN_POINT('Ctrl Pts',(-0.199432816941323,-0.000787987667539729,
0.248029551319403));
#28015=CARTESIAN_POINT('Ctrl Pts',(-0.107485294879524,-0.167991013844673,
0.25914426420118));
#28016=CARTESIAN_POINT('Ctrl Pts',(0.0828597134045088,-0.181406552517609,
0.270258977082955));
#28017=CARTESIAN_POINT('Ctrl Pts',(0.197350740743448,-0.0287533391599853,
0.281373689964733));
#28018=CARTESIAN_POINT('Ctrl Pts',(0.131176898264159,0.150222137987075,
0.292488402846508));
#28019=CARTESIAN_POINT('Ctrl Pts',(-0.0550829249158173,0.191676656820797,
0.303603115728285));
#28020=CARTESIAN_POINT('Ctrl Pts',(-0.190917047032656,0.0576606498114871,
0.31471782861006));
#28021=CARTESIAN_POINT('Ctrl Pts',(-0.151976028627464,-0.129140838260122,
0.325832541491837));
#28022=CARTESIAN_POINT('Ctrl Pts',(0.0260915485192222,-0.197720258144776,
0.336947254373613));
#28023=CARTESIAN_POINT('Ctrl Pts',(0.180273599833761,-0.0852965332675473,
0.348061967255389));
#28024=CARTESIAN_POINT('Ctrl Pts',(0.169424061603529,0.10521196098462,0.359176680137165));
#28025=CARTESIAN_POINT('Ctrl Pts',(0.0034751509790407,0.199404094015852,
0.370291393018941));
#28026=CARTESIAN_POINT('Ctrl Pts',(-0.165655088972228,0.111051613595375,
0.381406105900718));
#28027=CARTESIAN_POINT('Ctrl Pts',(-0.183136265087034,-0.078963141999978,
0.392520818782493));
#28028=CARTESIAN_POINT('Ctrl Pts',(-0.0329652228048722,-0.196691035560804,
0.40363553166427));
#28029=CARTESIAN_POINT('Ctrl Pts',(0.147383855108649,-0.134357986877806,
0.414750244546046));
#28030=CARTESIAN_POINT('Ctrl Pts',(0.192810282649647,0.0509731722488304,
0.425864957427822));
#28031=CARTESIAN_POINT('Ctrl Pts',(0.0617284058381346,0.18964090618121,
0.436979670309599));
#28032=CARTESIAN_POINT('Ctrl Pts',(-0.125862782069983,0.154701743604105,
0.448094383191375));
#28033=CARTESIAN_POINT('Ctrl Pts',(-0.198232800552033,-0.0218592353444565,
0.459209096073151));
#28034=CARTESIAN_POINT('Ctrl Pts',(-0.089130466980802,-0.178409162433804,
0.470323808954927));
#28035=CARTESIAN_POINT('Ctrl Pts',(0.101566413192055,-0.171634300464235,
0.481438521836703));
#28036=CARTESIAN_POINT('Ctrl Pts',(0.199284251348403,-0.00773670143234845,
0.49255323471848));
#28037=CARTESIAN_POINT('Ctrl Pts',(0.114567186105001,0.163243466186335,
0.503667947600255));
#28038=CARTESIAN_POINT('Ctrl Pts',(-0.075030487557911,0.184782291687729,
0.514782660482032));
#28039=CARTESIAN_POINT('Ctrl Pts',(-0.195941450369131,0.0371620426213107,
0.525897373363808));
#28040=CARTESIAN_POINT('Ctrl Pts',(-0.137477679210005,-0.14447822363103,
0.537012086245585));
#28041=CARTESIAN_POINT('Ctrl Pts',(0.0468401268595415,-0.193855801822718,
0.54812679912736));
#28042=CARTESIAN_POINT('Ctrl Pts',(0.188278106946687,-0.0657679544240076,
0.559241512009136));
#28043=CARTESIAN_POINT('Ctrl Pts',(0.157356766010237,0.122527211570924,
0.570356224890914));
#28044=CARTESIAN_POINT('Ctrl Pts',(-0.0176169333646449,0.198654758421167,
0.581470937772688));
#28045=CARTESIAN_POINT('Ctrl Pts',(-0.176463199112271,0.0929236715999202,
0.592585650654466));
#28046=CARTESIAN_POINT('Ctrl Pts',(-0.173766109246834,-0.0978744535707046,
0.60370036353624));
#28047=CARTESIAN_POINT('Ctrl Pts',(-0.0119947165195289,-0.199073343670525,
0.614815076418018));
#28048=CARTESIAN_POINT('Ctrl Pts',(0.160757247601359,-0.118030405947714,
0.625929789299793));
#28049=CARTESIAN_POINT('Ctrl Pts',(0.186343880099073,0.0710635471544257,
0.63704450218157));
#28050=CARTESIAN_POINT('Ctrl Pts',(0.0413418808560108,0.195102327694556,
0.648159215063346));
#28051=CARTESIAN_POINT('Ctrl Pts',(-0.141506571327,0.14053454968734,0.659273927945122));
#28052=CARTESIAN_POINT('Ctrl Pts',(-0.19481273657165,-0.0426856773872861,
0.670388640826899));
#28053=CARTESIAN_POINT('Ctrl Pts',(-0.0697774496593251,-0.186829272073696,
0.681503353708673));
#28054=CARTESIAN_POINT('Ctrl Pts',(0.119135650988641,-0.15993988260612,
0.692618066590452));
#28055=CARTESIAN_POINT('Ctrl Pts',(0.198985938933051,0.0133665811439721,
0.703732779472226));
#28056=CARTESIAN_POINT('Ctrl Pts',(0.0966744137811841,0.174436599097239,
0.714847492354004));
#28057=CARTESIAN_POINT('Ctrl Pts',(-0.0941377692002065,0.175818513799189,
0.725962205235778));
#28058=CARTESIAN_POINT('Ctrl Pts',(-0.198771467358517,0.0162472504962885,
0.737076918117557));
#28059=CARTESIAN_POINT('Ctrl Pts',(-0.121439690569283,-0.158197569320718,
0.748191630999331));
#28060=CARTESIAN_POINT('Ctrl Pts',(0.0670641335242294,-0.18782031673701,
0.759306343881108));
#28061=CARTESIAN_POINT('Ctrl Pts',(0.194174050982888,-0.0455028274884275,
0.770421056762883));
#28062=CARTESIAN_POINT('Ctrl Pts',(0.143527201441076,0.138470256123977,
0.781535769644661));
#28063=CARTESIAN_POINT('Ctrl Pts',(-0.0385117222509501,0.195680649615163,
0.792650482526435));
#28064=CARTESIAN_POINT('Ctrl Pts',(-0.185295063622389,0.073755059363555,
0.803765195408213));
#28065=CARTESIAN_POINT('Ctrl Pts',(-0.162449913009773,-0.115689650131998,
0.814879908289988));
#28066=CARTESIAN_POINT('Ctrl Pts',(0.00911012092507392,-0.19922619075131,
0.825994621171765));
#28067=CARTESIAN_POINT('Ctrl Pts',(0.172330288464656,-0.100380979583959,
0.837109334053541));
#28068=CARTESIAN_POINT('Ctrl Pts',(0.177790576253697,0.090358067597337,
0.848224046935317));
#28069=CARTESIAN_POINT('Ctrl Pts',(0.0204923601230103,0.198378760357896,
0.859338759817094));
#28070=CARTESIAN_POINT('Ctrl Pts',(-0.155565601016018,0.124793482061652,
0.870453472698869));
#28071=CARTESIAN_POINT('Ctrl Pts',(-0.189210926928472,-0.0630340742409649,
0.881568185580646));
#28072=CARTESIAN_POINT('Ctrl Pts',(-0.0496429811307334,-0.19315704441982,
0.892682898462421));
#28073=CARTESIAN_POINT('Ctrl Pts',(0.13537066549776,-0.146454266947876,
0.903797611344198));
#28074=CARTESIAN_POINT('Ctrl Pts',(0.196459144351367,0.0343201687827305,
0.914912324225975));
#28075=CARTESIAN_POINT('Ctrl Pts',(0.077698965926587,0.183676182665271,
0.92602703710775));
#28076=CARTESIAN_POINT('Ctrl Pts',(-0.112190783686916,0.164885710236704,
0.937141749989527));
#28077=CARTESIAN_POINT('Ctrl Pts',(-0.199375404090374,-0.0048494977417013,
0.948256462871302));
#28078=CARTESIAN_POINT('Ctrl Pts',(-0.104041675254465,-0.170145229715061,
0.959371175753079));
#28079=CARTESIAN_POINT('Ctrl Pts',(0.0865370759360344,-0.179681395455923,
0.970485888634854));
#28080=CARTESIAN_POINT('Ctrl Pts',(0.197895402120212,-0.0247281055527204,
0.981600601516632));
#28081=CARTESIAN_POINT('Ctrl Pts',(0.128090247874932,0.152862545392537,
0.992715314398406));
#28082=CARTESIAN_POINT('Ctrl Pts',(-0.0589752108821156,0.190515075219671,
1.00383002728019));
#28083=CARTESIAN_POINT('Ctrl Pts',(-0.192051772737075,0.0537604498966828,
1.01494474016196));
#28084=CARTESIAN_POINT('Ctrl Pts',(-0.149314408654731,-0.132209215838514,
1.02605945304374));
#28085=CARTESIAN_POINT('Ctrl Pts',(0.0301129323565648,-0.197147865039,1.03717416592551));
#28086=CARTESIAN_POINT('Ctrl Pts',(0.181973368966827,-0.0816073671393096,
1.04828887880729));
#28087=CARTESIAN_POINT('Ctrl Pts',(0.167246161224046,0.108640650496798,
1.05940359168907));
#28088=CARTESIAN_POINT('Ctrl Pts',(-0.000586658529918816,0.199433510765659,
1.07051830457085));
#28089=CARTESIAN_POINT('Ctrl Pts',(-0.167882421333772,0.107654827999754,
1.08163301745262));
#28090=CARTESIAN_POINT('Ctrl Pts',(-0.181490107376369,-0.0826765402581706,
1.0927477303344));
#28091=CARTESIAN_POINT('Ctrl Pts',(-0.028952551217501,-0.197321613521035,
1.10386244321617));
#28092=CARTESIAN_POINT('Ctrl Pts',(0.150089637639646,-0.131328481517706,
1.11497715609795));
#28093=CARTESIAN_POINT('Ctrl Pts',(0.191732165666487,0.0548893981874959,
1.12609186897972));
#28094=CARTESIAN_POINT('Ctrl Pts',(0.0578533522661112,0.19085874100004,
1.1372065818615));
#28095=CARTESIAN_POINT('Ctrl Pts',(-0.128987351803526,0.152106319590148,
1.14832129474328));
#28096=CARTESIAN_POINT('Ctrl Pts',(-0.197746496959982,-0.0258919355128762,
1.15943600762505));
#28097=CARTESIAN_POINT('Ctrl Pts',(-0.0854784770171591,-0.180187400645477,
1.17055072050683));
#28098=CARTESIAN_POINT('Ctrl Pts',(0.105040872831909,-0.16953018733918,
1.18166543338861));
#28099=CARTESIAN_POINT('Ctrl Pts',(0.199400484224714,-0.00367644876158102,
1.19278014627038));
#28100=CARTESIAN_POINT('Ctrl Pts',(0.111218786752117,0.1655428973346,1.20389485915216));
#28101=CARTESIAN_POINT('Ctrl Pts',(-0.0787782246756555,0.18321588550532,
1.21500957203393));
#28102=CARTESIAN_POINT('Ctrl Pts',(-0.196657656759033,0.033163766712988,
1.22612428491571));
#28103=CARTESIAN_POINT('Ctrl Pts',(-0.134506703245444,-0.147248144866374,
1.23723899779749));
#28104=CARTESIAN_POINT('Ctrl Pts',(0.0507785032116992,-0.192861642106786,
1.24835371067926));
#28105=CARTESIAN_POINT('Ctrl Pts',(0.18957849437697,-0.0619198179447247,
1.25946842356104));
#28106=CARTESIAN_POINT('Ctrl Pts',(0.154828723961395,0.125706545657069,
1.27058313644281));
#28107=CARTESIAN_POINT('Ctrl Pts',(-0.0216591070800636,0.198254766563231,
1.28169784932459));
#28108=CARTESIAN_POINT('Ctrl Pts',(-0.17831909381802,0.0893105266162228,
1.29281256220637));
#28109=CARTESIAN_POINT('Ctrl Pts',(-0.171736744872623,-0.101393095648087,
1.30392727508814));
#28110=CARTESIAN_POINT('Ctrl Pts',(-0.00793787606159387,-0.199276339559359,
1.31504198796992));
#28111=CARTESIAN_POINT('Ctrl Pts',(0.163127726787361,-0.114731922923546,
1.3261567008517));
#28112=CARTESIAN_POINT('Ctrl Pts',(0.184857941230518,0.0748439105643279,
1.33727141373347));
#28113=CARTESIAN_POINT('Ctrl Pts',(0.0373598276804767,0.195903835236148,
1.34838612661525));
#28114=CARTESIAN_POINT('Ctrl Pts',(-0.144339365522383,0.137623460736688,
1.35950083949703));
#28115=CARTESIAN_POINT('Ctrl Pts',(-0.193902988414568,-0.0466444044709194,
1.3706155523788));
#28116=CARTESIAN_POINT('Ctrl Pts',(-0.0659579887187589,-0.188211617889871,
1.38173026526058));
#28117=CARTESIAN_POINT('Ctrl Pts',(0.122368296597616,-0.157480377737496,
1.39284497814235));
#28118=CARTESIAN_POINT('Ctrl Pts',(0.19867244158967,0.017416381293079,1.40395969102413));
#28119=CARTESIAN_POINT('Ctrl Pts',(0.0931017648416045,0.176369302226678,
1.41507440390591));
#28120=CARTESIAN_POINT('Ctrl Pts',(-0.0976989858350325,0.173864825514976,
1.42618911678768));
#28121=CARTESIAN_POINT('Ctrl Pts',(-0.199061133498795,0.0121956760666124,
1.43730382966946));
#28122=CARTESIAN_POINT('Ctrl Pts',(-0.118192631149939,-0.160638013329352,
1.44841854255123));
#28123=CARTESIAN_POINT('Ctrl Pts',(0.0708753957499276,-0.186415524197525,
1.45953325543301));
#28124=CARTESIAN_POINT('Ctrl Pts',(0.195060493418966,-0.041538816686279,
1.47064796831478));
#28125=CARTESIAN_POINT('Ctrl Pts',(0.140677329756692,0.141364628804641,
1.48176268119656));
#28126=CARTESIAN_POINT('Ctrl Pts',(-0.0424889910845633,0.194855728735808,
1.49287739407834));
#28127=CARTESIAN_POINT('Ctrl Pts',(-0.186758736147166,0.0699660193040883,
1.50399210696011));
#28128=CARTESIAN_POINT('Ctrl Pts',(-0.160060069217685,-0.118974130072788,
1.51510681984189));
#28129=CARTESIAN_POINT('Ctrl Pts',(0.0131656969095905,-0.198999331178352,
1.52622153272367));
#28130=CARTESIAN_POINT('Ctrl Pts',(0.174338916848997,-0.0968504592475705,
1.53733624560544));
#28131=CARTESIAN_POINT('Ctrl Pts',(0.175913456817656,0.0939602314546404,
1.54845095848722));
#28132=CARTESIAN_POINT('Ctrl Pts',(0.0164479031306532,0.198754964383664,
1.559565671369));
#28133=CARTESIAN_POINT('Ctrl Pts',(-0.158074894661018,0.121599330024695,
1.57068038425077));
#28134=CARTESIAN_POINT('Ctrl Pts',(-0.18788792265261,-0.0668744936865572,
1.58179509713255));
#28135=CARTESIAN_POINT('Ctrl Pts',(-0.0456988240979224,-0.194128016681297,
1.59290981001432));
#28136=CARTESIAN_POINT('Ctrl Pts',(0.138325294050016,-0.143666914808259,
1.6040245228961));
#28137=CARTESIAN_POINT('Ctrl Pts',(0.195719427705911,0.0383141619119788,
1.61513923577788));
#28138=CARTESIAN_POINT('Ctrl Pts',(0.0739420781894689,0.185220513058271,
1.62625394865965));
#28139=CARTESIAN_POINT('Ctrl Pts',(-0.115525597082264,0.162566619585121,
1.63736866154143));
#28140=CARTESIAN_POINT('Ctrl Pts',(-0.199235285953682,-0.00890899632401715,
1.6484833744232));
#28141=CARTESIAN_POINT('Ctrl Pts',(-0.100554896829241,-0.172228865490681,
1.65959808730498));
#28142=CARTESIAN_POINT('Ctrl Pts',(0.0901785409695924,-0.177881702637294,
1.67071280018676));
#28143=CARTESIAN_POINT('Ctrl Pts',(0.198357972121127,-0.0206926141543518,
1.68182751306853));
#28144=CARTESIAN_POINT('Ctrl Pts',(0.124950462821344,0.155439542026084,
1.69294222595031));
#28145=CARTESIAN_POINT('Ctrl Pts',(-0.062843032628011,0.189274463767994,
1.70405693883209));
#28146=CARTESIAN_POINT('Ctrl Pts',(-0.193106831128081,0.0498379489567696,
1.71517165171386));
#28147=CARTESIAN_POINT('Ctrl Pts',(-0.146590849769418,-0.135222750114125,
1.72628636459564));
#28148=CARTESIAN_POINT('Ctrl Pts',(0.0341218246847609,-0.196493690648655,
1.73740107747742));
#28149=CARTESIAN_POINT('Ctrl Pts',(0.183597651530221,-0.0778843484734545,
1.74851579035919));
#28150=CARTESIAN_POINT('Ctrl Pts',(0.164998883445552,0.112024273469048,
1.75963050324097));
#28151=CARTESIAN_POINT('Ctrl Pts',(-0.00464822467994746,0.199380198093671,
1.77074521612274));
#28152=CARTESIAN_POINT('Ctrl Pts',(-0.170040112361639,0.104213384805349,
1.78185992900452));
#28153=CARTESIAN_POINT('Ctrl Pts',(-0.179768663563496,-0.0863556424626734,
1.7929746418863));
#28154=CARTESIAN_POINT('Ctrl Pts',(-0.0249278694728741,-0.197870338120928,
1.80408935476807));
#28155=CARTESIAN_POINT('Ctrl Pts',(0.152733159676335,-0.128244498204911,
1.81520406764985));
#28156=CARTESIAN_POINT('Ctrl Pts',(0.190574513949296,0.0587828547923301,
1.82631878053162));
#28157=CARTESIAN_POINT('Ctrl Pts',(0.0539542998466873,0.191997403400672,
1.8374334934134));
#28158=CARTESIAN_POINT('Ctrl Pts',(-0.132058414736671,0.149447798517691,
1.84854820629517));
#28159=CARTESIAN_POINT('Ctrl Pts',(-0.197178163756537,-0.0299138951349875,
1.85966291917695));
#28160=CARTESIAN_POINT('Ctrl Pts',(-0.0817910286946564,-0.181890893146459,
1.87077763205873));
#28161=CARTESIAN_POINT('Ctrl Pts',(0.108471759199364,-0.167355749350723,
1.8818923449405));
#28162=CARTESIAN_POINT('Ctrl Pts',(0.19943400137921,0.000385328981277993,
1.89300705782228));
#28163=CARTESIAN_POINT('Ctrl Pts',(0.107824251391782,0.167773657635365,
1.90412177070405));
#28164=CARTESIAN_POINT('Ctrl Pts',(-0.0824932828470974,0.181573477329856,
1.91523648358584));
#28165=CARTESIAN_POINT('Ctrl Pts',(-0.197292285212489,0.0291517337422745,
1.92635119646761));
#28166=CARTESIAN_POINT('Ctrl Pts',(-0.131479930931687,-0.149956984321324,
1.93746590934939));
#28167=CARTESIAN_POINT('Ctrl Pts',(0.0546958155199975,-0.19178747912507,
1.94858062223116));
#28168=CARTESIAN_POINT('Ctrl Pts',(0.190800240463607,-0.0580459957583295,
1.95969533511294));
#28169=CARTESIAN_POINT('Ctrl Pts',(0.152236455540641,0.128833733893613,
1.97081004799471));
#28170=CARTESIAN_POINT('Ctrl Pts',(-0.0256922961198321,0.19777253425245,
1.98192476087649));
#28171=CARTESIAN_POINT('Ctrl Pts',(-0.18010101782797,0.0856603336549266,
1.99303947375827));
#28172=CARTESIAN_POINT('Ctrl Pts',(-0.169636140306269,-0.104869677631563,
2.00415418664004));
#28173=CARTESIAN_POINT('Ctrl Pts',(-0.00387774279743271,-0.199396671224306,
2.01526889952182));
#28174=CARTESIAN_POINT('Ctrl Pts',(0.165430536991843,-0.111385846565546,
2.02638361240359));
#28175=CARTESIAN_POINT('Ctrl Pts',(0.183295319208086,0.0785932270683423,
2.03749832528537));
#28176=CARTESIAN_POINT('Ctrl Pts',(0.03336227682359,0.19662407754294,2.04861303816715));
#28177=CARTESIAN_POINT('Ctrl Pts',(-0.147112284562752,0.134655282537346,
2.05972775104892));
#28178=CARTESIAN_POINT('Ctrl Pts',(-0.192912805019205,-0.0505837824266837,
2.0708424639307));
#28179=CARTESIAN_POINT('Ctrl Pts',(-0.0621111669469283,-0.189515889371824,
2.08195717681248));
#28180=CARTESIAN_POINT('Ctrl Pts',(0.12555018113299,-0.154955546534564,
2.09307188969425));
#28181=CARTESIAN_POINT('Ctrl Pts',(0.198276530539081,0.021458956746869,
2.10418660257603));
#28182=CARTESIAN_POINT('Ctrl Pts',(0.0894904952228435,0.178228843469243,
2.11530131545781));
#28183=CARTESIAN_POINT('Ctrl Pts',(-0.101219674750872,0.171839014278377,
2.12641602833958));
#28184=CARTESIAN_POINT('Ctrl Pts',(-0.199268224731861,0.00813904257355614,
2.13753074122136));
#28185=CARTESIAN_POINT('Ctrl Pts',(-0.11489654273405,-0.16301182109179,
2.14864545410313));
#28186=CARTESIAN_POINT('Ctrl Pts',(0.0746572571364039,-0.184933402484744,
2.15976016698491));
#28187=CARTESIAN_POINT('Ctrl Pts',(0.195866020763059,-0.0375575744749643,
2.17087487986668));
#28188=CARTESIAN_POINT('Ctrl Pts',(0.137769101429214,0.144200359953505,
2.18198959274846));
#28189=CARTESIAN_POINT('Ctrl Pts',(-0.0464486334400941,0.193949978091433,
2.19310430563024));
#28190=CARTESIAN_POINT('Ctrl Pts',(-0.18814493913174,0.0661479544793682,
2.20421901851201));
#28191=CARTESIAN_POINT('Ctrl Pts',(-0.157603824970919,-0.122209254414689,
2.21533373139379));
#28192=CARTESIAN_POINT('Ctrl Pts',(0.0172158038531715,-0.198689927053832,
2.22644844427557));
#28193=CARTESIAN_POINT('Ctrl Pts',(0.176275240096993,-0.0932797541422112,
2.23756315715734));
#28194=CARTESIAN_POINT('Ctrl Pts',(0.173963337024785,0.0975234012975608,
2.24867787003912));
#28195=CARTESIAN_POINT('Ctrl Pts',(0.0123966756361006,0.199048753252725,
2.2597925829209));
#28196=CARTESIAN_POINT('Ctrl Pts',(-0.16051871512871,0.118354673526729,
2.27090729580267));
#28197=CARTESIAN_POINT('Ctrl Pts',(-0.186486788511679,-0.0706870534597272,
2.28202200868445));
#28198=CARTESIAN_POINT('Ctrl Pts',(-0.0417360712567089,-0.195018686077598,
2.29313672156622));
#28199=CARTESIAN_POINT('Ctrl Pts',(0.141223229087202,-0.140819537071881,
2.304251434448));
#28200=CARTESIAN_POINT('Ctrl Pts',(0.194897215685731,0.0422914446510719,
2.31536614732978));
#28201=CARTESIAN_POINT('Ctrl Pts',(0.0701570032722593,0.18668956375646,
2.32648086021155));
#28202=CARTESIAN_POINT('Ctrl Pts',(-0.118817216374208,0.160177136774138,
2.33759557309333));
#28203=CARTESIAN_POINT('Ctrl Pts',(-0.199003525246202,-0.0129591760037057,
2.3487102859751));
#28204=CARTESIAN_POINT('Ctrl Pts',(-0.097043521379645,-0.174251755453708,
2.35982499885688));
#28205=CARTESIAN_POINT('Ctrl Pts',(0.0938151859874535,-0.175987856857017,
2.37093971173865));
#28206=CARTESIAN_POINT('Ctrl Pts',(0.198676013796531,-0.0166873789156056,
2.38205442462043));
#28207=CARTESIAN_POINT('Ctrl Pts',(0.121879426163471,0.158026820897646,
2.39316913750221));
#28208=CARTESIAN_POINT('Ctrl Pts',(-0.0669327158999945,0.187805554375717,
2.40428385038399));
#28209=CARTESIAN_POINT('Ctrl Pts',(-0.151287880662087,0.0934337713860927,
2.41169365897184));
#28210=CARTESIAN_POINT('Ctrl Pts',(-0.164200416389812,0.0388286878179645,
2.41539856326576));
#28211=CARTESIAN_POINT('Ctrl Pts',(0.0901593640056525,-0.126416002494549,
0.00015634029999317));
#28212=CARTESIAN_POINT('Ctrl Pts',(0.132213650477217,-0.0964246555277346,
0.00386243223197628));
#28213=CARTESIAN_POINT('Ctrl Pts',(0.183298020212533,0.00828926491431173,
0.0112734284578848));
#28214=CARTESIAN_POINT('Ctrl Pts',(0.0922373614706075,0.158809128352571,
0.0223893289777186));
#28215=CARTESIAN_POINT('Ctrl Pts',(-0.0833287157598494,0.163461487822337,
0.0335040418594948));
#28216=CARTESIAN_POINT('Ctrl Pts',(-0.182571295414348,0.0187086709426025,
0.044618754741271));
#28217=CARTESIAN_POINT('Ctrl Pts',(-0.114699979162333,-0.143293650960574,
0.0557334676230472));
#28218=CARTESIAN_POINT('Ctrl Pts',(0.0581846142819802,-0.174053383984867,
0.0668481805048234));
#28219=CARTESIAN_POINT('Ctrl Pts',(0.177798226195109,-0.0455096217415463,
0.0779628933865995));
#28220=CARTESIAN_POINT('Ctrl Pts',(0.134649399343971,0.124713717114316,
0.0890776062683758));
#28221=CARTESIAN_POINT('Ctrl Pts',(-0.0317659246301578,0.180758461746217,
0.100192319150151));
#28222=CARTESIAN_POINT('Ctrl Pts',(-0.169100263415532,0.0713326579444572,
0.111307032031928));
#28223=CARTESIAN_POINT('Ctrl Pts',(-0.151632096793471,-0.10339725624643,
0.122421744913704));
#28224=CARTESIAN_POINT('Ctrl Pts',(0.0046480102430308,-0.183470725562448,
0.13353645779548));
#28225=CARTESIAN_POINT('Ctrl Pts',(0.156672969974193,-0.0955865074097566,
0.144651170677256));
#28226=CARTESIAN_POINT('Ctrl Pts',(0.165271617559767,0.0798028187524376,
0.155765883559033));
#28227=CARTESIAN_POINT('Ctrl Pts',(0.0225722164382812,0.182136403197904,
0.166880596440809));
#28228=CARTESIAN_POINT('Ctrl Pts',(-0.140790917677612,0.117733197065986,
0.177995309322585));
#28229=CARTESIAN_POINT('Ctrl Pts',(-0.175266919880487,-0.0544489988186458,
0.189110022204361));
#28230=CARTESIAN_POINT('Ctrl Pts',(-0.0492946961622294,-0.176785793091077,
0.200224735086137));
#28231=CARTESIAN_POINT('Ctrl Pts',(0.121804388076487,-0.137283927918741,
0.211339447967913));
#28232=CARTESIAN_POINT('Ctrl Pts',(0.181397563796251,0.0278946103217992,
0.22245416084969));
#28233=CARTESIAN_POINT('Ctrl Pts',(0.0749302156796734,0.167537004418727,
0.233568873731466));
#28234=CARTESIAN_POINT('Ctrl Pts',(-0.100132048951932,0.153807536089727,
0.244683586613242));
#28235=CARTESIAN_POINT('Ctrl Pts',(-0.183528361484412,-0.000725146882597591,
0.255798299495018));
#28236=CARTESIAN_POINT('Ctrl Pts',(-0.0989135106019816,-0.154593993044227,
0.266913012376794));
#28237=CARTESIAN_POINT('Ctrl Pts',(0.0762517807621952,-0.166939663475187,
0.27802772525857));
#28238=CARTESIAN_POINT('Ctrl Pts',(0.181612327609234,-0.0264603053006625,
0.289142438140347));
#28239=CARTESIAN_POINT('Ctrl Pts',(0.120715745644371,0.138242157265243,
0.300257151022123));
#28240=CARTESIAN_POINT('Ctrl Pts',(-0.0506901477430488,0.176390743011373,
0.311371863903899));
#28241=CARTESIAN_POINT('Ctrl Pts',(-0.175691710916637,0.053062303107031,
0.322486576785675));
#28242=CARTESIAN_POINT('Ctrl Pts',(-0.139856177868226,-0.118842058243485,
0.333601289667452));
#28243=CARTESIAN_POINT('Ctrl Pts',(0.0240107883033711,-0.181952376575327,
0.344716002549227));
#28244=CARTESIAN_POINT('Ctrl Pts',(0.165897061997177,-0.0784942680496771,
0.355830715431004));
#28245=CARTESIAN_POINT('Ctrl Pts',(0.155912757484034,0.0968214715321897,
0.366945428312779));
#28246=CARTESIAN_POINT('Ctrl Pts',(0.00319801311979034,0.183501929167357,
0.378060141194556));
#28247=CARTESIAN_POINT('Ctrl Pts',(-0.152444354529535,0.102195420974054,
0.389174854076332));
#28248=CARTESIAN_POINT('Ctrl Pts',(-0.168531434170574,-0.0726659548372124,
0.400289566958108));
#28249=CARTESIAN_POINT('Ctrl Pts',(-0.0303362978076353,-0.18100523288385,
0.411404279839885));
#28250=CARTESIAN_POINT('Ctrl Pts',(0.13563022301041,-0.123643147412814,
0.422518992721661));
#28251=CARTESIAN_POINT('Ctrl Pts',(0.17743396395212,0.0469081414281092,
0.433633705603437));
#28252=CARTESIAN_POINT('Ctrl Pts',(0.0568056619480616,0.17451734030361,
0.444748418485213));
#28253=CARTESIAN_POINT('Ctrl Pts',(-0.115825421911227,0.142364521335509,
0.455863131366989));
#28254=CARTESIAN_POINT('Ctrl Pts',(-0.18242404452666,-0.020115995489598,
0.466977844248765));
#28255=CARTESIAN_POINT('Ctrl Pts',(-0.0820224515413663,-0.164181310565931,
0.478092557130542));
#28256=CARTESIAN_POINT('Ctrl Pts',(0.0934666504784431,-0.157946733249989,
0.489207270012318));
#28257=CARTESIAN_POINT('Ctrl Pts',(0.183391643765334,-0.00711971158483698,
0.500321982894094));
#28258=CARTESIAN_POINT('Ctrl Pts',(0.105430632070536,0.150225054891685,
0.51143669577587));
#28259=CARTESIAN_POINT('Ctrl Pts',(-0.0690469234405426,0.170046192722443,
0.522551408657646));
#28260=CARTESIAN_POINT('Ctrl Pts',(-0.180315425939685,0.0341984278029353,
0.533666121539423));
#28261=CARTESIAN_POINT('Ctrl Pts',(-0.126514049157296,-0.132956311101909,
0.544780834421199));
#28262=CARTESIAN_POINT('Ctrl Pts',(0.0431046999490668,-0.178396104605183,
0.555895547302975));
#28263=CARTESIAN_POINT('Ctrl Pts',(0.173263222178117,-0.060523062847634,
0.567010260184751));
#28264=CARTESIAN_POINT('Ctrl Pts',(0.144807809854295,0.112755857946294,
0.578124973066527));
#28265=CARTESIAN_POINT('Ctrl Pts',(-0.0162120104623694,0.182812351915209,
0.589239685948304));
#28266=CARTESIAN_POINT('Ctrl Pts',(-0.16239053477794,0.0855131540205209,
0.600354398830079));
#28267=CARTESIAN_POINT('Ctrl Pts',(-0.159908533613985,-0.0900691188667203,
0.611469111711856));
#28268=CARTESIAN_POINT('Ctrl Pts',(-0.0110381566236799,-0.183197555645139,
0.622583824593632));
#28269=CARTESIAN_POINT('Ctrl Pts',(0.147937108353142,-0.108617665543471,
0.633698537475408));
#28270=CARTESIAN_POINT('Ctrl Pts',(0.171483246898593,0.0653963403342919,
0.644813250357184));
#28271=CARTESIAN_POINT('Ctrl Pts',(0.0380449304711,0.179543221986939,0.65592796323896));
#28272=CARTESIAN_POINT('Ctrl Pts',(-0.130221643424722,0.129327138991656,
0.667042676120737));
#28273=CARTESIAN_POINT('Ctrl Pts',(-0.179276725303484,-0.039281561329222,
0.678157389002513));
#28274=CARTESIAN_POINT('Ctrl Pts',(-0.0642128071043873,-0.171929929621858,
0.689272101884288));
#28275=CARTESIAN_POINT('Ctrl Pts',(0.109634769019767,-0.147184926938816,
0.700386814766066));
#28276=CARTESIAN_POINT('Ctrl Pts',(0.183117121298874,0.0123006171884068,
0.711501527647841));
#28277=CARTESIAN_POINT('Ctrl Pts',(0.0889647803748755,0.160525552946727,
0.722616240529618));
#28278=CARTESIAN_POINT('Ctrl Pts',(-0.0866304292346941,0.161797262110999,
0.733730953411393));
#28279=CARTESIAN_POINT('Ctrl Pts',(-0.182919753497209,0.014951557662091,
0.74484566629317));
#28280=CARTESIAN_POINT('Ctrl Pts',(-0.11175506504485,-0.145581560414854,
0.755960379174946));
#28281=CARTESIAN_POINT('Ctrl Pts',(0.0617158736904078,-0.172841940022184,
0.767075092056721));
#28282=CARTESIAN_POINT('Ctrl Pts',(0.178688973892221,-0.0418740481127377,
0.778189804938499));
#28283=CARTESIAN_POINT('Ctrl Pts',(0.132081131445255,0.127427469613673,
0.789304517820274));
#28284=CARTESIAN_POINT('Ctrl Pts',(-0.0354404725915213,0.180075423638242,
0.800419230702051));
#28285=CARTESIAN_POINT('Ctrl Pts',(-0.170518071896724,0.0678732086513234,
0.811533943583826));
#28286=CARTESIAN_POINT('Ctrl Pts',(-0.149494786340711,-0.106463581345676,
0.822648656465604));
#28287=CARTESIAN_POINT('Ctrl Pts',(0.00838360301953096,-0.183338213410116,
0.833763369347378));
#28288=CARTESIAN_POINT('Ctrl Pts',(0.158587217295133,-0.0923757533478818,
0.844878082229157));
#28289=CARTESIAN_POINT('Ctrl Pts',(0.163612055666903,0.0831521529273459,
0.85599279511093));
#28290=CARTESIAN_POINT('Ctrl Pts',(0.0188581264307767,0.182558364266125,
0.867107507992709));
#28291=CARTESIAN_POINT('Ctrl Pts',(-0.143159487468943,0.114841396907353,
0.878222220874483));
#28292=CARTESIAN_POINT('Ctrl Pts',(-0.174121651224263,-0.0580072053363914,
0.88933693375626));
#28293=CARTESIAN_POINT('Ctrl Pts',(-0.0456840309727285,-0.177753072013075,
0.900451646638036));
#28294=CARTESIAN_POINT('Ctrl Pts',(0.124575066495539,-0.134774768052608,
0.911566359519812));
#28295=CARTESIAN_POINT('Ctrl Pts',(0.180791834635944,0.0315831889614004,
0.922681072401588));
#28296=CARTESIAN_POINT('Ctrl Pts',(0.071502594829897,0.169028294165782,
0.933795785283364));
#28297=CARTESIAN_POINT('Ctrl Pts',(-0.103243744031201,0.15173633254571,
0.944910498165141));
#28298=CARTESIAN_POINT('Ctrl Pts',(-0.183475527218596,-0.00446275787609136,
0.956025211046916));
#28299=CARTESIAN_POINT('Ctrl Pts',(-0.0957445142599781,-0.156576413565783,
0.967139923928694));
#28300=CARTESIAN_POINT('Ctrl Pts',(0.0796358793791929,-0.165352084992918,
0.978254636810468));
#28301=CARTESIAN_POINT('Ctrl Pts',(0.182113553092454,-0.0227560777825268,
0.989369349692247));
#28302=CARTESIAN_POINT('Ctrl Pts',(0.117875250799549,0.140671996306819,
1.00048406257403));
#28303=CARTESIAN_POINT('Ctrl Pts',(-0.0542720299868005,0.175321795727498,
1.0115987754558));
#28304=CARTESIAN_POINT('Ctrl Pts',(-0.176735944019595,0.0494731380397978,
1.02271348833758));
#28305=CARTESIAN_POINT('Ctrl Pts',(-0.137406817928465,-0.121665737505578,
1.03382820121935));
#28306=CARTESIAN_POINT('Ctrl Pts',(0.027711473064719,-0.181425630925142,
1.04494291410113));
#28307=CARTESIAN_POINT('Ctrl Pts',(0.167461277198455,-0.0750993071543572,
1.05605762698291));
#28308=CARTESIAN_POINT('Ctrl Pts',(0.153908541255967,0.0999767284144798,
1.06717233986468));
#28309=CARTESIAN_POINT('Ctrl Pts',(-0.000539873429044207,0.183528999977341,
1.07828705274646));
#28310=CARTESIAN_POINT('Ctrl Pts',(-0.154494060616352,0.0990695237208374,
1.08940176562824));
#28311=CARTESIAN_POINT('Ctrl Pts',(-0.167016554964549,-0.0760832153879955,
1.10051647851001));
#28312=CARTESIAN_POINT('Ctrl Pts',(-0.0266436305079402,-0.181585523237285,
1.11163119139179));
#28313=CARTESIAN_POINT('Ctrl Pts',(0.138120223613435,-0.120855240370358,
1.12274590427356));
#28314=CARTESIAN_POINT('Ctrl Pts',(0.176441825113375,0.0505120544688475,
1.13386061715534));
#28315=CARTESIAN_POINT('Ctrl Pts',(0.053239637842074,0.175638054698995,
1.14497533003712));
#28316=CARTESIAN_POINT('Ctrl Pts',(-0.118700812091919,0.139976078330269,
1.15609004291889));
#28317=CARTESIAN_POINT('Ctrl Pts',(-0.181976522886029,-0.0238270941223055,
1.16720475580067));
#28318=CARTESIAN_POINT('Ctrl Pts',(-0.078661702069618,-0.165817737059439,
1.17831946868244));
#28319=CARTESIAN_POINT('Ctrl Pts',(0.0966640273922626,-0.156010419858132,
1.18943418156422));
#28320=CARTESIAN_POINT('Ctrl Pts',(0.18349860725142,-0.00338325771878211,
1.200548894446));
#28321=CARTESIAN_POINT('Ctrl Pts',(0.102349262332821,0.152341109999664,
1.21166360732777));
#28322=CARTESIAN_POINT('Ctrl Pts',(-0.0724957843804967,0.168604704984941,
1.22277832020955));
#28323=CARTESIAN_POINT('Ctrl Pts',(-0.180974515989352,0.0305190081493839,
1.23389303309133));
#28324=CARTESIAN_POINT('Ctrl Pts',(-0.123780003882562,-0.135505335447854,
1.2450077459731));
#28325=CARTESIAN_POINT('Ctrl Pts',(0.0467289969424402,-0.177481227572822,
1.25612245885488));
#28326=CARTESIAN_POINT('Ctrl Pts',(0.174459905743215,-0.05698180923831,
1.26723717173665));
#28327=CARTESIAN_POINT('Ctrl Pts',(0.142481375207763,0.115681645108059,
1.27835188461843));
#28328=CARTESIAN_POINT('Ctrl Pts',(-0.019931827141509,0.182444258782795,
1.28946659750021));
#28329=CARTESIAN_POINT('Ctrl Pts',(-0.164098424781489,0.082188151702278,
1.30058131038198));
#28330=CARTESIAN_POINT('Ctrl Pts',(-0.158041007876917,-0.0933071547377274,
1.31169602326376));
#28331=CARTESIAN_POINT('Ctrl Pts',(-0.00730484285181677,-0.183384362929101,
1.32281073614554));
#28332=CARTESIAN_POINT('Ctrl Pts',(0.150118545528891,-0.10558223138527,
1.33392544902731));
#28333=CARTESIAN_POINT('Ctrl Pts',(0.170115809332428,0.068875225670596,
1.34504016190909));
#28334=CARTESIAN_POINT('Ctrl Pts',(0.0343804398127517,0.180280810554767,
1.35615487479086));
#28335=CARTESIAN_POINT('Ctrl Pts',(-0.132828526710406,0.126648204835068,
1.36726958767264));
#28336=CARTESIAN_POINT('Ctrl Pts',(-0.178439528140082,-0.0429245861150422,
1.37838430055441));
#28337=CARTESIAN_POINT('Ctrl Pts',(-0.060697942204384,-0.173202035519666,
1.38949901343619));
#28338=CARTESIAN_POINT('Ctrl Pts',(0.112609616193738,-0.144921563739498,
1.40061372631797));
#28339=CARTESIAN_POINT('Ctrl Pts',(0.182828624878661,0.0160274521050675,
1.41172843919975));
#28340=CARTESIAN_POINT('Ctrl Pts',(0.0856770446045232,0.162304126022221,
1.42284315208152));
#28341=CARTESIAN_POINT('Ctrl Pts',(-0.0899076444087289,0.159999377414026,
1.4339578649633));
#28342=CARTESIAN_POINT('Ctrl Pts',(-0.18318631921552,0.0112230899609635,
1.44507257784508));
#28343=CARTESIAN_POINT('Ctrl Pts',(-0.10876695353936,-0.147827382827977,
1.45618729072685));
#28344=CARTESIAN_POINT('Ctrl Pts',(0.0652231937102401,-0.171549177492167,
1.46730200360863));
#28345=CARTESIAN_POINT('Ctrl Pts',(0.179504723929444,-0.038226160976696,
1.4784167164904));
#28346=CARTESIAN_POINT('Ctrl Pts',(0.129458532573627,0.130091020596679,
1.48953142937218));
#28347=CARTESIAN_POINT('Ctrl Pts',(-0.0391005604517399,0.179316288909742,
1.50064614225395));
#28348=CARTESIAN_POINT('Ctrl Pts',(-0.171865018825228,0.0643863386146969,
1.51176085513573));
#28349=CARTESIAN_POINT('Ctrl Pts',(-0.147295528855949,-0.109486129144512,
1.52287556801751));
#28350=CARTESIAN_POINT('Ctrl Pts',(0.0121157531577547,-0.183129445533543,
1.53399028089928));
#28351=CARTESIAN_POINT('Ctrl Pts',(0.160435660705114,-0.0891267864904594,
1.54510499378106));
#28352=CARTESIAN_POINT('Ctrl Pts',(0.16188463357213,0.0864670498468623,
1.55621970666283));
#28353=CARTESIAN_POINT('Ctrl Pts',(0.0151362085624658,0.182904566608809,
1.56733441954461));
#28354=CARTESIAN_POINT('Ctrl Pts',(-0.145468668867536,0.111901973503194,
1.57844913242639));
#28355=CARTESIAN_POINT('Ctrl Pts',(-0.172904154471676,-0.0615413573334011,
1.58956384530816));
#28356=CARTESIAN_POINT('Ctrl Pts',(-0.0420544142989491,-0.178646610754234,
1.60067855818994));
#28357=CARTESIAN_POINT('Ctrl Pts',(0.12729406803855,-0.132209702889763,
1.61179327107171));
#28358=CARTESIAN_POINT('Ctrl Pts',(0.180111109236858,0.0352586673808153,
1.62290798395349));
#28359=CARTESIAN_POINT('Ctrl Pts',(0.0680453130181629,0.17044946662358,
1.63402269683527));
#28360=CARTESIAN_POINT('Ctrl Pts',(-0.106312611270259,0.149602185749077,
1.64513740971704));
#28361=CARTESIAN_POINT('Ctrl Pts',(-0.183346583284314,-0.00819851779107011,
1.65625212259882));
#28362=CARTESIAN_POINT('Ctrl Pts',(-0.0925358009646688,-0.158493882644819,
1.6673668354806));
#28363=CARTESIAN_POINT('Ctrl Pts',(0.0829869432675812,-0.163695914863828,
1.67848154836237));
#28364=CARTESIAN_POINT('Ctrl Pts',(0.182539233858749,-0.0190424105160965,
1.68959626124415));
#28365=CARTESIAN_POINT('Ctrl Pts',(0.114985858696805,0.143043481486438,
1.70071097412593));
#28366=CARTESIAN_POINT('Ctrl Pts',(-0.057831398993491,0.174180121100136,
1.7118256870077));
#28367=CARTESIAN_POINT('Ctrl Pts',(-0.177706863152873,0.0458634504193542,
1.72294039988948));
#28368=CARTESIAN_POINT('Ctrl Pts',(-0.134900458607596,-0.12443894713257,
1.73405511277125));
#28369=CARTESIAN_POINT('Ctrl Pts',(0.0314006624952514,-0.180823625920016,
1.74516982565303));
#28370=CARTESIAN_POINT('Ctrl Pts',(0.168956025766015,-0.0716731934083868,
1.75628453853481));
#28371=CARTESIAN_POINT('Ctrl Pts',(0.151840480368031,0.103090512742967,
1.76739925141658));
#28372=CARTESIAN_POINT('Ctrl Pts',(-0.00427753602644203,0.183479938907623,
1.77851396429836));
#28373=CARTESIAN_POINT('Ctrl Pts',(-0.156479679157009,0.0959025302425444,
1.78962867718014));
#28374=CARTESIAN_POINT('Ctrl Pts',(-0.165432393605304,-0.0794689149417693,
1.80074339006191));
#28375=CARTESIAN_POINT('Ctrl Pts',(-0.0229399108422602,-0.18209048790794,
1.81185810294369));
#28376=CARTESIAN_POINT('Ctrl Pts',(0.140552928899268,-0.118017199906791,
1.82297281582546));
#28377=CARTESIAN_POINT('Ctrl Pts',(0.175376494311331,0.0540950139945414,
1.83408752870724));
#28378=CARTESIAN_POINT('Ctrl Pts',(0.0496515287592585,0.176685910552798,
1.84520224158902));
#28379=CARTESIAN_POINT('Ctrl Pts',(-0.121526962555918,0.137529570158329,
1.85631695447079));
#28380=CARTESIAN_POINT('Ctrl Pts',(-0.181453513367309,-0.0275283087504863,
1.86743166735257));
#28381=CARTESIAN_POINT('Ctrl Pts',(-0.0752683219877107,-0.167385378695861,
1.87854638023434));
#28382=CARTESIAN_POINT('Ctrl Pts',(0.0998213059340555,-0.154009389900818,
1.88966109311612));
#28383=CARTESIAN_POINT('Ctrl Pts',(0.183529451465229,0.000354599597248665,
1.9007758059979));
#28384=CARTESIAN_POINT('Ctrl Pts',(0.0992254358621439,0.154393970652905,
1.91189051887967));
#28385=CARTESIAN_POINT('Ctrl Pts',(-0.075914572469042,0.167093276294544,
1.92300523176145));
#28386=CARTESIAN_POINT('Ctrl Pts',(-0.181558533815509,0.0268269285376663,
1.93411994464322));
#28387=CARTESIAN_POINT('Ctrl Pts',(-0.120994611930274,-0.137998149189926,
1.945234657525));
#28388=CARTESIAN_POINT('Ctrl Pts',(0.0503339097165312,-0.176492727410085,
1.95634937040678));
#28389=CARTESIAN_POINT('Ctrl Pts',(0.175584219488913,-0.0534169183168714,
1.96746408328856));
#28390=CARTESIAN_POINT('Ctrl Pts',(0.140095836142101,0.118559444970232,
1.97857879617033));
#28391=CARTESIAN_POINT('Ctrl Pts',(-0.0236433756588397,0.182000483745117,
1.98969350905211));
#28392=CARTESIAN_POINT('Ctrl Pts',(-0.165738243136619,0.0788290559247478,
2.00080822193388));
#28393=CARTESIAN_POINT('Ctrl Pts',(-0.156107923241689,-0.0965064847415824,
2.01192293481566));
#28394=CARTESIAN_POINT('Ctrl Pts',(-0.00356849886987757,-0.183495098331836,
2.02303764769743));
#28395=CARTESIAN_POINT('Ctrl Pts',(0.152237710218634,-0.102502999387228,
2.03415236057921));
#28396=CARTESIAN_POINT('Ctrl Pts',(0.168677803974058,0.0723255400432333,
2.04526707346099));
#28397=CARTESIAN_POINT('Ctrl Pts',(0.0307016873889171,0.180943614663262,
2.05638178634276));
#28398=CARTESIAN_POINT('Ctrl Pts',(-0.13538030979111,0.123916734208149,
2.06749649922454));
#28399=CARTESIAN_POINT('Ctrl Pts',(-0.177528310322938,-0.0465498048357001,
2.07861121210631));
#28400=CARTESIAN_POINT('Ctrl Pts',(-0.0571578984566474,-0.174402293389383,
2.08972592498809));
#28401=CARTESIAN_POINT('Ctrl Pts',(0.115537750410393,-0.142598083878933,
2.10084063786986));
#28402=CARTESIAN_POINT('Ctrl Pts',(0.182464287115587,0.0197476384845713,
2.11195535075165));
#28403=CARTESIAN_POINT('Ctrl Pts',(0.0823537680937941,0.164015371756973,
2.12307006363342));
#28404=CARTESIAN_POINT('Ctrl Pts',(-0.0931475638860256,0.1581351214574,
2.1341847765152));
#28405=CARTESIAN_POINT('Ctrl Pts',(-0.183376895246413,0.00748996664885357,
2.14529948939697));
#28406=CARTESIAN_POINT('Ctrl Pts',(-0.105733723023171,-0.150011883131391,
2.15641420227875));
#28407=CARTESIAN_POINT('Ctrl Pts',(0.0687034575618276,-0.170185252669568,
2.16752891516052));
#28408=CARTESIAN_POINT('Ctrl Pts',(0.180246011726807,-0.0345624166094378,
2.1786436280423));
#28409=CARTESIAN_POINT('Ctrl Pts',(0.126782230909987,0.132700606618394,
2.18975834092408));
#28410=CARTESIAN_POINT('Ctrl Pts',(-0.0427444275179538,0.178482770463656,
2.20087305380585));
#28411=CARTESIAN_POINT('Ctrl Pts',(-0.173140674288284,0.0608727584924831,
2.21198776668763));
#28412=CARTESIAN_POINT('Ctrl Pts',(-0.14503516624899,-0.112463257376332,
2.2231024795694));
#28413=CARTESIAN_POINT('Ctrl Pts',(0.0158428704025093,-0.182844715904384,
2.23421719245118));
#28414=CARTESIAN_POINT('Ctrl Pts',(0.162217565200369,-0.085840839536587,
2.24533190533296));
#28415=CARTESIAN_POINT('Ctrl Pts',(0.160090032784892,0.0897460624636993,
2.25644661821473));
#28416=CARTESIAN_POINT('Ctrl Pts',(0.0114080601289279,0.183174926274725,
2.26756133109651));
#28417=CARTESIAN_POINT('Ctrl Pts',(-0.147717598472383,0.108916073289857,
2.27867604397829));
#28418=CARTESIAN_POINT('Ctrl Pts',(-0.171614758588647,-0.0650498714233224,
2.28979075686006));
#28419=CARTESIAN_POINT('Ctrl Pts',(-0.0384076848034237,-0.179466250658209,
2.30090546974184));
#28420=CARTESIAN_POINT('Ctrl Pts',(0.129960897285711,-0.129589399077687,
2.31202018262361));
#28421=CARTESIAN_POINT('Ctrl Pts',(0.17935446734025,0.0389187680375732,
2.32313489550539));
#28422=CARTESIAN_POINT('Ctrl Pts',(0.0645620919098956,0.171801362824571,
2.33424960838716));
#28423=CARTESIAN_POINT('Ctrl Pts',(-0.109341729068153,0.14740326045774,
2.34536432126895));
#28424=CARTESIAN_POINT('Ctrl Pts',(-0.183133305131037,-0.0119257019713418,
2.35647903415071));
#28425=CARTESIAN_POINT('Ctrl Pts',(-0.0893044522192385,-0.160355450294875,
2.3675937470325));
#28426=CARTESIAN_POINT('Ctrl Pts',(0.0863335715289918,-0.161953100324632,
2.37870845991427));
#28427=CARTESIAN_POINT('Ctrl Pts',(0.182831912207608,-0.0153565865278459,
2.38982317279605));
#28428=CARTESIAN_POINT('Ctrl Pts',(0.112159732412666,0.145424428911658,
2.40093788567783));
#28429=CARTESIAN_POINT('Ctrl Pts',(-0.0615949364163127,0.172828354936131,
2.4120525985596));
#28430=CARTESIAN_POINT('Ctrl Pts',(-0.139222908627576,0.085982574145982,
2.41946240714745));
#28431=CARTESIAN_POINT('Ctrl Pts',(-0.151105689812057,0.0357321606499603,
2.42316731144138));
#28432=CARTESIAN_POINT('',(0.103380467594096,0.116394573955406,2.40007508722328));
#28433=CARTESIAN_POINT('Ctrl Pts',(0.103461767481305,0.116497970106859,
2.4));
#28434=CARTESIAN_POINT('Ctrl Pts',(0.101062838412543,0.119258880418803,
2.4));
#28435=CARTESIAN_POINT('Ctrl Pts',(0.0985654514169241,0.121922998634949,
2.4));
#28436=CARTESIAN_POINT('Ctrl Pts',(0.095972990647464,0.124483778490481,
2.4));
#28437=CARTESIAN_POINT('Ctrl Pts',(0.0883971619082253,0.131967027553669,
2.4));
#28438=CARTESIAN_POINT('Ctrl Pts',(0.0800129758471178,0.138570016932135,
2.4));
#28439=CARTESIAN_POINT('Ctrl Pts',(0.0710089580556215,0.144290176540958,
2.4));
#28440=CARTESIAN_POINT('Ctrl Pts',(0.0663636114037173,0.147241317343045,
2.4));
#28441=CARTESIAN_POINT('Ctrl Pts',(0.0615524547995155,0.149957058484752,
2.4));
#28442=CARTESIAN_POINT('Ctrl Pts',(0.0565975106583602,0.152433694248754,
2.4));
#28443=CARTESIAN_POINT('Ctrl Pts',(0.0527699197084543,0.154346843694329,
2.4));
#28444=CARTESIAN_POINT('Ctrl Pts',(0.0488630480765027,0.156113602347608,
2.4));
#28445=CARTESIAN_POINT('Ctrl Pts',(0.0449001875407907,0.157728503257228,
2.4));
#28446=CARTESIAN_POINT('Ctrl Pts',(0.035918044860841,0.161388806276592,
2.4));
#28447=CARTESIAN_POINT('Ctrl Pts',(0.0266316597928958,0.164279400994296,
2.4));
#28448=CARTESIAN_POINT('Ctrl Pts',(0.0171631885948985,0.16639083815603,
2.4));
#28449=CARTESIAN_POINT('Ctrl Pts',(0.00998520832101847,0.167991503562255,
2.4));
#28450=CARTESIAN_POINT('Ctrl Pts',(0.00270180372882996,0.169144080993686,
2.4));
#28451=CARTESIAN_POINT('Ctrl Pts',(-0.00463850986789263,0.169835856818611,
2.4));
#28452=CARTESIAN_POINT('Ctrl Pts',(-0.00897136590947692,0.170244199735156,
2.4));
#28453=CARTESIAN_POINT('Ctrl Pts',(-0.0133190494795881,0.170490952148472,
2.4));
#28454=CARTESIAN_POINT('Ctrl Pts',(-0.0176555019082484,0.170574199016548,
2.4));
#28455=CARTESIAN_POINT('Ctrl Pts',(-0.0285870584998179,0.170784052085254,
2.4));
#28456=CARTESIAN_POINT('Ctrl Pts',(-0.039474963002183,0.169960336922977,
2.4));
#28457=CARTESIAN_POINT('Ctrl Pts',(-0.0501623159300887,0.168075457674568,
2.4));
#28458=CARTESIAN_POINT('Ctrl Pts',(-0.0531380387349237,0.167550643138949,
2.4));
#28459=CARTESIAN_POINT('Ctrl Pts',(-0.0560982762643852,0.166943351080139,
2.4));
#28460=CARTESIAN_POINT('Ctrl Pts',(-0.059039724474309,0.1662524758191,2.4));
#28461=CARTESIAN_POINT('Ctrl Pts',(-0.0633625816644486,0.165237140896798,
2.4));
#28462=CARTESIAN_POINT('Ctrl Pts',(-0.0676448709143601,0.164041331557733,
2.4));
#28463=CARTESIAN_POINT('Ctrl Pts',(-0.0718806214018753,0.162672203759917,
2.4));
#28464=CARTESIAN_POINT('Ctrl Pts',(-0.0757157250276606,0.161432577630607,
2.4));
#28465=CARTESIAN_POINT('Ctrl Pts',(-0.0795060665151785,0.160052743939154,
2.4));
#28466=CARTESIAN_POINT('Ctrl Pts',(-0.083238263168423,0.158543149031955,
2.4));
#28467=CARTESIAN_POINT('Ctrl Pts',(-0.0942712060057412,0.154080556123256,
2.4));
#28468=CARTESIAN_POINT('Ctrl Pts',(-0.104821070565539,0.148480110078236,
2.4));
#28469=CARTESIAN_POINT('Ctrl Pts',(-0.114778874551992,0.141898905553672,
2.4));
#28470=CARTESIAN_POINT('Ctrl Pts',(-0.120197102208962,0.13831794890704,
2.4));
#28471=CARTESIAN_POINT('Ctrl Pts',(-0.125439738625044,0.134445884472761,
2.4));
#28472=CARTESIAN_POINT('Ctrl Pts',(-0.130488353457401,0.130301426506045,
2.4));
#28473=CARTESIAN_POINT('Ctrl Pts',(-0.134449742315667,0.127049483119975,
2.4));
#28474=CARTESIAN_POINT('Ctrl Pts',(-0.138288930969708,0.123631215695906,
2.4));
#28475=CARTESIAN_POINT('Ctrl Pts',(-0.141981521250133,0.120071365074424,
2.4));
#28476=CARTESIAN_POINT('Ctrl Pts',(-0.148243719704175,0.11403427745692,
2.4));
#28477=CARTESIAN_POINT('Ctrl Pts',(-0.154096955106979,0.107580854604382,
2.4));
#28478=CARTESIAN_POINT('Ctrl Pts',(-0.159498257185175,0.100759941050575,
2.4));
#28479=CARTESIAN_POINT('Ctrl Pts',(-0.162517575610272,0.0969470622908144,
2.4));
#28480=CARTESIAN_POINT('Ctrl Pts',(-0.165397051519882,0.0930169578682919,
2.4));
#28481=CARTESIAN_POINT('Ctrl Pts',(-0.16812342541814,0.0889841305063993,
2.4));
#28482=CARTESIAN_POINT('Ctrl Pts',(-0.174697816516933,0.0792593512573283,
2.4));
#28483=CARTESIAN_POINT('Ctrl Pts',(-0.180364044921554,0.0689697058721336,
2.4));
#28484=CARTESIAN_POINT('Ctrl Pts',(-0.185015139554039,0.0582282398394182,
2.4));
#28485=CARTESIAN_POINT('Ctrl Pts',(-0.186897941765302,0.0538800040806022,
2.4));
#28486=CARTESIAN_POINT('Ctrl Pts',(-0.188614220377741,0.0494572905282926,
2.4));
#28487=CARTESIAN_POINT('Ctrl Pts',(-0.190155688860645,0.0449663651403318,
2.4));
#28488=CARTESIAN_POINT('Ctrl Pts',(0.104759235283674,0.114983934194216,
2.4));
#28489=CARTESIAN_POINT('Ctrl Pts',(0.10427439309968,0.115425662830347,2.40002502907443));
#28490=CARTESIAN_POINT('Ctrl Pts',(0.103786756983843,0.115864324841204,
2.40005005814885));
#28491=CARTESIAN_POINT('Ctrl Pts',(0.10329636595052,0.11629988513071,2.40007508722328));
#28492=CARTESIAN_POINT('Ctrl Pts',(0.0863566694936598,0.175642871684081,
3.00324001778485E-17));
#28493=CARTESIAN_POINT('Ctrl Pts',(0.0902251377602555,0.173267020623209,
1.02990543755693E-16));
#28494=CARTESIAN_POINT('Ctrl Pts',(0.0939991325874576,0.170750246590702,
-9.76497076806834E-17));
#28495=CARTESIAN_POINT('Ctrl Pts',(0.0976698484646395,0.16809208422283,
-8.68445940160889E-17));
#28496=CARTESIAN_POINT('Ctrl Pts',(0.104400047624094,0.163218385812893,
-6.02536217891983E-17));
#28497=CARTESIAN_POINT('Ctrl Pts',(0.110783523872764,0.157869648682406,
-3.87972721901173E-17));
#28498=CARTESIAN_POINT('Ctrl Pts',(0.11679477944429,0.152098287545979,-3.64291929955129E-17));
#28499=CARTESIAN_POINT('Ctrl Pts',(0.122324543199851,0.146789203070577,
-3.42507931013796E-17));
#28500=CARTESIAN_POINT('Ctrl Pts',(0.127544162554551,0.141115067318068,
-1.26605818491442E-17));
#28501=CARTESIAN_POINT('Ctrl Pts',(0.132400641086032,0.135150809061649,
-8.89045781438114E-17));
#28502=CARTESIAN_POINT('Ctrl Pts',(0.137099361104822,0.129380294585985,
-1.62671854037244E-16));
#28503=CARTESIAN_POINT('Ctrl Pts',(0.141463395349392,0.123334515287111,
-5.10858319320469E-17));
#28504=CARTESIAN_POINT('Ctrl Pts',(0.145472480412238,0.117050620606459,
-9.0205620750794E-17));
#28505=CARTESIAN_POINT('Ctrl Pts',(0.148028749789222,0.113043889073319,
-1.15149146922942E-16));
#28506=CARTESIAN_POINT('Ctrl Pts',(0.150440599606425,0.108940295545949,
-4.4214120273351E-17));
#28507=CARTESIAN_POINT('Ctrl Pts',(0.152701484434877,0.104749210972548,
-9.36750677027476E-17));
#28508=CARTESIAN_POINT('Ctrl Pts',(0.154529352382147,0.101360825567148,
-1.33662987171292E-16));
#28509=CARTESIAN_POINT('Ctrl Pts',(0.156257288991465,0.0979170901241365,
-9.60317181142712E-17));
#28510=CARTESIAN_POINT('Ctrl Pts',(0.157877700765807,0.0944331993150869,
-1.64798730217797E-17));
#28511=CARTESIAN_POINT('Ctrl Pts',(0.163035894966784,0.0833430642934671,
2.36754442187825E-16));
#28512=CARTESIAN_POINT('Ctrl Pts',(0.16712377054151,0.0718185232873831,
4.96472933007523E-18));
#28513=CARTESIAN_POINT('Ctrl Pts',(0.170039561512778,0.0600249603217789,
-7.11236625150491E-17));
#28514=CARTESIAN_POINT('Ctrl Pts',(0.171494712723099,0.0541392786688407,
-1.09096245795481E-16));
#28515=CARTESIAN_POINT('Ctrl Pts',(0.17265715824647,0.0481865085500087,
-8.55724220067749E-17));
#28516=CARTESIAN_POINT('Ctrl Pts',(0.173509220055223,0.0421877481517497,
-2.25514051876985E-17));
#28517=CARTESIAN_POINT('Ctrl Pts',(0.174254193713336,0.036942919159156,
3.25490546091879E-17));
#28518=CARTESIAN_POINT('Ctrl Pts',(0.174761331352098,0.0316591437943461,
-1.13288127970075E-16));
#28519=CARTESIAN_POINT('Ctrl Pts',(0.175017019263399,0.0263849939813338,
-1.31838984174237E-16));
#28520=CARTESIAN_POINT('Ctrl Pts',(0.175312644314683,0.0202870490256223,
-1.53287388945601E-16));
#28521=CARTESIAN_POINT('Ctrl Pts',(0.175274136046595,0.0141923338965255,
-1.87526340687399E-16));
#28522=CARTESIAN_POINT('Ctrl Pts',(0.174886275518905,0.00812263339345144,
-1.05818132034585E-16));
#28523=CARTESIAN_POINT('Ctrl Pts',(0.174375504119754,0.000129478130005221,
-7.9097615780314E-18));
#28524=CARTESIAN_POINT('Ctrl Pts',(0.173259119449215,-0.00782060291629472,
-1.15450484634852E-16));
#28525=CARTESIAN_POINT('Ctrl Pts',(0.171567084712523,-0.0156736935166775,
-7.28583859910259E-17));
#28526=CARTESIAN_POINT('Ctrl Pts',(0.170483272838823,-0.0207038933425822,
-4.55765452374446E-17));
#28527=CARTESIAN_POINT('Ctrl Pts',(0.169162566961701,-0.0256957555113034,
2.18154106348517E-16));
#28528=CARTESIAN_POINT('Ctrl Pts',(0.16761260374838,-0.0306286181104371,
2.77555756156289E-17));
#28529=CARTESIAN_POINT('Ctrl Pts',(0.166323465714418,-0.0347313869621074,
-1.30603013458363E-16));
#28530=CARTESIAN_POINT('Ctrl Pts',(0.164878296492824,-0.0387849189721862,
-7.45107699010496E-17));
#28531=CARTESIAN_POINT('Ctrl Pts',(0.163285258777898,-0.0427743425247604,
-2.77555756156289E-17));
#28532=CARTESIAN_POINT('Ctrl Pts',(0.159781230740532,-0.0515494341940759,
7.50866296464515E-17));
#28533=CARTESIAN_POINT('Ctrl Pts',(0.15555905845194,-0.0600274982283718,
-1.67125813435077E-16));
#28534=CARTESIAN_POINT('Ctrl Pts',(0.150667339924487,-0.068116122664101,
-1.45716771982052E-16));
#28535=CARTESIAN_POINT('Ctrl Pts',(0.146817200022984,-0.0744824611019111,
-1.28866292076344E-16));
#28536=CARTESIAN_POINT('Ctrl Pts',(0.142551803362311,-0.0806074016922841,
-2.96987614464865E-16));
#28537=CARTESIAN_POINT('Ctrl Pts',(0.137888788869483,-0.0864371653375756,
-4.85722573273506E-17));
#28538=CARTESIAN_POINT('Ctrl Pts',(0.135609742264458,-0.0892864601584125,
7.28406563985689E-17));
#28539=CARTESIAN_POINT('Ctrl Pts',(0.133240253652339,-0.0920591324808986,
7.04833804390097E-17));
#28540=CARTESIAN_POINT('Ctrl Pts',(0.130787574864596,-0.0947448381828875,
3.12250225675825E-17));
#28541=CARTESIAN_POINT('Ctrl Pts',(0.125477874028838,-0.100559009154527,
-5.37637401852564E-17));
#28542=CARTESIAN_POINT('Ctrl Pts',(0.119772613931372,-0.105974110081735,
-1.21563507678846E-16));
#28543=CARTESIAN_POINT('Ctrl Pts',(0.113697442368773,-0.110930478022775,
-6.93889390390723E-17));
#28544=CARTESIAN_POINT('Ctrl Pts',(0.10643549160352,-0.116855067903314,
-7.02211618374062E-18));
#28545=CARTESIAN_POINT('Ctrl Pts',(0.0986448235562052,-0.12212533697402,
-1.11878079465019E-16));
#28546=CARTESIAN_POINT('Ctrl Pts',(0.0903606778650216,-0.126612599672285,
-1.73472347597681E-17));
#28547=CARTESIAN_POINT('Origin',(-0.0866025403784439,-0.15,-0.3));
#28548=CARTESIAN_POINT('',(-0.0866025403784439,-0.15,-0.3));
#28549=CARTESIAN_POINT('',(0.0866025403784439,-0.15,-0.3));
#28550=CARTESIAN_POINT('',(-0.043301270189222,-0.15,-0.3));
#28551=CARTESIAN_POINT('',(-0.0866025403784439,-0.15,-0.1));
#28552=CARTESIAN_POINT('',(-0.0866025403784439,-0.15,-0.3));
#28553=CARTESIAN_POINT('',(0.0866025403784439,-0.15,-0.1));
#28554=CARTESIAN_POINT('',(-0.0866025403784439,-0.15,-0.1));
#28555=CARTESIAN_POINT('',(0.0866025403784439,-0.15,-0.3));
#28556=CARTESIAN_POINT('Origin',(-0.173205080756888,2.12115047744981E-17,
-0.3));
#28557=CARTESIAN_POINT('',(-0.173205080756888,2.12115047744981E-17,-0.3));
#28558=CARTESIAN_POINT('',(-0.151554445662277,-0.0375,-0.3));
#28559=CARTESIAN_POINT('',(-0.173205080756888,2.77555756156289E-17,-0.1));
#28560=CARTESIAN_POINT('',(-0.173205080756888,2.12115047744981E-17,-0.3));
#28561=CARTESIAN_POINT('',(-0.173205080756888,2.12115047744981E-17,-0.1));
#28562=CARTESIAN_POINT('Origin',(-0.0866025403784438,0.15,-0.3));
#28563=CARTESIAN_POINT('',(-0.0866025403784438,0.15,-0.3));
#28564=CARTESIAN_POINT('',(-0.108253175473055,0.1125,-0.3));
#28565=CARTESIAN_POINT('',(-0.0866025403784438,0.15,-0.1));
#28566=CARTESIAN_POINT('',(-0.0866025403784438,0.15,-0.3));
#28567=CARTESIAN_POINT('',(-0.0866025403784438,0.15,-0.1));
#28568=CARTESIAN_POINT('Origin',(0.0866025403784439,0.15,-0.3));
#28569=CARTESIAN_POINT('',(0.0866025403784439,0.15,-0.3));
#28570=CARTESIAN_POINT('',(0.043301270189222,0.15,-0.3));
#28571=CARTESIAN_POINT('',(0.0866025403784439,0.15,-0.1));
#28572=CARTESIAN_POINT('',(0.0866025403784439,0.15,-0.3));
#28573=CARTESIAN_POINT('',(0.0866025403784439,0.15,-0.1));
#28574=CARTESIAN_POINT('Origin',(0.173205080756888,0.,-0.3));
#28575=CARTESIAN_POINT('',(0.173205080756888,0.,-0.3));
#28576=CARTESIAN_POINT('',(0.151554445662277,0.0375,-0.3));
#28577=CARTESIAN_POINT('',(0.173205080756888,0.,-0.1));
#28578=CARTESIAN_POINT('',(0.173205080756888,0.,-0.3));
#28579=CARTESIAN_POINT('',(0.173205080756888,0.,-0.1));
#28580=CARTESIAN_POINT('Origin',(0.0866025403784439,-0.15,-0.3));
#28581=CARTESIAN_POINT('',(0.108253175473055,-0.1125,-0.3));
#28582=CARTESIAN_POINT('',(0.0866025403784439,-0.15,-0.1));
#28583=CARTESIAN_POINT('Origin',(0.,2.77555756156289E-17,-0.1));
#28584=CARTESIAN_POINT('Origin',(0.,0.,0.));
#28585=CARTESIAN_POINT('',(-0.4,-4.89858719658941E-17,0.));
#28586=CARTESIAN_POINT('Origin',(0.,0.,0.));
#28587=CARTESIAN_POINT('Origin',(0.,0.,-0.3));
#28588=CARTESIAN_POINT('',(-0.4,-4.89858719658941E-17,-0.3));
#28589=CARTESIAN_POINT('',(-0.4,-4.89858719658941E-17,-0.3));
#28590=CARTESIAN_POINT('Origin',(0.,0.,-0.3));
#28591=CARTESIAN_POINT('Origin',(0.,0.,-0.3));
#28592=CARTESIAN_POINT('Origin',(0.,0.,2.4));
#28593=CARTESIAN_POINT('',(0.,0.,0.));
#28594=CARTESIAN_POINT('Origin',(0.,0.,0.554592528053768));
#28595=CARTESIAN_POINT('',(0.125207372047943,0.162920500888771,0.0106050744780265));
#28596=CARTESIAN_POINT('',(0.124934343482292,0.162564573588643,0.00478498949683932));
#28597=CARTESIAN_POINT('',(0.125207372047944,0.16292050088877,0.554592528053768));
#28598=CARTESIAN_POINT('',(0.181742788875946,0.0958620587959239,0.));
#28599=CARTESIAN_POINT('Ctrl Pts',(0.124934343482292,0.162564573588643,
0.00478498949683932));
#28600=CARTESIAN_POINT('Ctrl Pts',(0.148318591442515,0.144625169784585,
0.0031899929978929));
#28601=CARTESIAN_POINT('Ctrl Pts',(0.168018548550233,0.1218815470411,0.00159499649894647));
#28602=CARTESIAN_POINT('Ctrl Pts',(0.181742788875947,0.0958620587959227,
0.));
#28603=CARTESIAN_POINT('',(0.205337197401384,-0.00752402740192784,1.13225540054884E-10));
#28604=CARTESIAN_POINT('Origin',(0.,0.,0.));
#28605=CARTESIAN_POINT('Ctrl Pts',(0.125207372047943,0.162920500888771,
0.0106050744780265));
#28606=CARTESIAN_POINT('Ctrl Pts',(0.135191036397379,0.15524787301332,0.00991897992953218));
#28607=CARTESIAN_POINT('Ctrl Pts',(0.144499847540114,0.146628725624496,
0.00923288538103781));
#28608=CARTESIAN_POINT('Ctrl Pts',(0.152951970006133,0.137206670742508,
0.0085467908325435));
#28609=CARTESIAN_POINT('Ctrl Pts',(0.161726091348647,0.127425665656181,
0.00783455827260035));
#28610=CARTESIAN_POINT('Ctrl Pts',(0.169576008636495,0.11677979549158,0.00712232571265741));
#28611=CARTESIAN_POINT('Ctrl Pts',(0.176338684112991,0.105473428456171,
0.00641009315271424));
#28612=CARTESIAN_POINT('Ctrl Pts',(0.182841040154334,0.0946022837067508,
0.00572527695754354));
#28613=CARTESIAN_POINT('Ctrl Pts',(0.188338039031849,0.0831214749447625,
0.00504046076237263));
#28614=CARTESIAN_POINT('Ctrl Pts',(0.192729448030586,0.0712413888608711,
0.00435564456720194));
#28615=CARTESIAN_POINT('Ctrl Pts',(0.197121501740769,0.0593595586380301,
0.00367072783281035));
#28616=CARTESIAN_POINT('Ctrl Pts',(0.2004073773629,0.0470791616454508,0.00298581109841873));
#28617=CARTESIAN_POINT('Ctrl Pts',(0.202536285480387,0.034626993643793,
0.00230089436402714));
#28618=CARTESIAN_POINT('Ctrl Pts',(0.204669951533879,0.0221469960622687,
0.00161444689659701));
#28619=CARTESIAN_POINT('Ctrl Pts',(0.205641422441559,0.00949532753146084,
0.000927999429167045));
#28620=CARTESIAN_POINT('Ctrl Pts',(0.205451672523553,-0.00309610760064894,
0.000241551961736919));
#28621=CARTESIAN_POINT('Ctrl Pts',(0.205429415688848,-0.00457302781954408,
0.000161034678899832));
#28622=CARTESIAN_POINT('Ctrl Pts',(0.205391241254496,-0.00604912403675888,
8.05173960626305E-5));
#28623=CARTESIAN_POINT('Ctrl Pts',(0.205337197401384,-0.00752402740192794,
1.13225540054884E-10));
#28624=CARTESIAN_POINT('Origin',(0.,0.,0.554592528053768));
#28625=CARTESIAN_POINT('',(0.125161044493656,0.16285866358402,0.0806174252350157));
#28626=CARTESIAN_POINT('',(0.125207372047944,0.16292050088877,0.0747863044042028));
#28627=CARTESIAN_POINT('',(0.125207372047944,0.16292050088877,0.554592528053768));
#28628=CARTESIAN_POINT('',(-0.20546235540252,-0.000151937791236579,0.0295925301446521));
#28629=CARTESIAN_POINT('Ctrl Pts',(0.125207372047944,0.16292050088877,0.0747863044042028));
#28630=CARTESIAN_POINT('Ctrl Pts',(0.135260192360196,0.155194725396423,
0.0740996580920012));
#28631=CARTESIAN_POINT('Ctrl Pts',(0.144610938545834,0.146523023284227,
0.0734130117797997));
#28632=CARTESIAN_POINT('Ctrl Pts',(0.153083746180861,0.137059630381209,
0.0727263654675981));
#28633=CARTESIAN_POINT('Ctrl Pts',(0.161551511709001,0.127601869075248,
0.0720401277736786));
#28634=CARTESIAN_POINT('Ctrl Pts',(0.169141797394902,0.117353995805741,
0.071353890079759));
#28635=CARTESIAN_POINT('Ctrl Pts',(0.175717374888728,0.106505304033246,
0.0706676523858395));
#28636=CARTESIAN_POINT('Ctrl Pts',(0.182309139155736,0.0956299065739565,
0.0699797254146039));
#28637=CARTESIAN_POINT('Ctrl Pts',(0.187880772542185,0.0841514911841738,
0.0692917984433683));
#28638=CARTESIAN_POINT('Ctrl Pts',(0.192340188204511,0.0722857359819571,
0.0686038714721326));
#28639=CARTESIAN_POINT('Ctrl Pts',(0.196450264707989,0.0613495135381388,
0.0679698349313207));
#28640=CARTESIAN_POINT('Ctrl Pts',(0.199615952662604,0.0500850390171815,
0.0673357983905087));
#28641=CARTESIAN_POINT('Ctrl Pts',(0.201803192669525,0.0386710105038203,
0.0667017618496967));
#28642=CARTESIAN_POINT('Ctrl Pts',(0.204176317968265,0.0262869466882869,
0.0660138409308376));
#28643=CARTESIAN_POINT('Ctrl Pts',(0.205413490830913,0.0136405328699919,
0.0653259200119784));
#28644=CARTESIAN_POINT('Ctrl Pts',(0.205472755776309,0.000960343006070464,
0.0646379990931193));
#28645=CARTESIAN_POINT('Ctrl Pts',(0.205531897792633,-0.0116935452396088,
0.0639515050798178));
#28646=CARTESIAN_POINT('Ctrl Pts',(0.204417904171905,-0.0243802152524297,
0.0632650110665164));
#28647=CARTESIAN_POINT('Ctrl Pts',(0.202140596895965,-0.0368667154970847,
0.0625785170532149));
#28648=CARTESIAN_POINT('Ctrl Pts',(0.199863615838169,-0.0493514270841568,
0.0618921213783348));
#28649=CARTESIAN_POINT('Ctrl Pts',(0.196423760605867,-0.0616351685143203,
0.0612057257034547));
#28650=CARTESIAN_POINT('Ctrl Pts',(0.191882452794946,-0.0734921760080312,
0.0605193300285745));
#28651=CARTESIAN_POINT('Ctrl Pts',(0.187341539995639,-0.085348152156618,
0.0598329940576992));
#28652=CARTESIAN_POINT('Ctrl Pts',(0.181699696856621,-0.0967766695112979,
0.0591466580868238));
#28653=CARTESIAN_POINT('Ctrl Pts',(0.175066635828823,-0.107571597759717,
0.0584603221159485));
#28654=CARTESIAN_POINT('Ctrl Pts',(0.16841825206409,-0.118391462887969,
0.0577724006711138));
#28655=CARTESIAN_POINT('Ctrl Pts',(0.160774582289236,-0.128574111464531,
0.0570844792262791));
#28656=CARTESIAN_POINT('Ctrl Pts',(0.152288266677789,-0.137942957258697,
0.0563965577814444));
#28657=CARTESIAN_POINT('Ctrl Pts',(0.148950279128879,-0.141628077167082,
0.0561259723681009));
#28658=CARTESIAN_POINT('Ctrl Pts',(0.145482337108395,-0.145187682787088,
0.0558553869547575));
#28659=CARTESIAN_POINT('Ctrl Pts',(0.141895208834322,-0.14861266882357,
0.055584801541414));
#28660=CARTESIAN_POINT('Ctrl Pts',(0.13279099500499,-0.157305361935212,
0.0548980495565511));
#28661=CARTESIAN_POINT('Ctrl Pts',(0.122852615423652,-0.16518924674948,
0.0542112975716881));
#28662=CARTESIAN_POINT('Ctrl Pts',(0.112248597575376,-0.172105281637029,
0.0535245455868252));
#28663=CARTESIAN_POINT('Ctrl Pts',(0.101666698579554,-0.179006890412003,
0.0528392260934992));
#28664=CARTESIAN_POINT('Ctrl Pts',(0.0904225953185901,-0.184944124413337,
0.0521539066001731));
#28665=CARTESIAN_POINT('Ctrl Pts',(0.0787166429651472,-0.189799014078834,
0.0514685871068471));
#28666=CARTESIAN_POINT('Ctrl Pts',(0.0670122096419139,-0.194653273746546,
0.0507833565444327));
#28667=CARTESIAN_POINT('Ctrl Pts',(0.0548468279443643,-0.198425091847161,
0.0500981259820183));
#28668=CARTESIAN_POINT('Ctrl Pts',(0.0424428474164345,-0.201043727403233,
0.0494128954196039));
#28669=CARTESIAN_POINT('Ctrl Pts',(0.0300398755813251,-0.203662150011624,
0.0487277205802009));
#28670=CARTESIAN_POINT('Ctrl Pts',(0.0173991977050335,-0.20512742159407,
0.0480425457407979));
#28671=CARTESIAN_POINT('Ctrl Pts',(0.00475285713355531,-0.20542002330364,
0.0473573709013949));
#28672=CARTESIAN_POINT('Ctrl Pts',(-0.00792325603801462,-0.205713313869693,
0.0466705829916835));
#28673=CARTESIAN_POINT('Ctrl Pts',(-0.0206041896027675,-0.204828463813174,
0.0459837950819722));
#28674=CARTESIAN_POINT('Ctrl Pts',(-0.0330594692979208,-0.202798045145262,
0.0452970071722607));
#28675=CARTESIAN_POINT('Ctrl Pts',(-0.0380719307092315,-0.201980930197159,
0.0450206185258843));
#28676=CARTESIAN_POINT('Ctrl Pts',(-0.0430479551847099,-0.200978867605235,
0.0447442298795076));
#28677=CARTESIAN_POINT('Ctrl Pts',(-0.0479731481905962,-0.199796277937511,
0.0444678412331312));
#28678=CARTESIAN_POINT('Ctrl Pts',(-0.0602519252280685,-0.19684801685628,
0.0437787891370023));
#28679=CARTESIAN_POINT('Ctrl Pts',(-0.0723001442737591,-0.19275349126515,
0.0430897370408734));
#28680=CARTESIAN_POINT('Ctrl Pts',(-0.0838917469720236,-0.187569055057016,
0.0424006849447446));
#28681=CARTESIAN_POINT('Ctrl Pts',(-0.0954591205084849,-0.182395455533594,
0.0417130731287187));
#28682=CARTESIAN_POINT('Ctrl Pts',(-0.106570964122892,-0.176136749040885,
0.0410254613126929));
#28683=CARTESIAN_POINT('Ctrl Pts',(-0.117018611011345,-0.168898254289307,
0.040337849496667));
#28684=CARTESIAN_POINT('Ctrl Pts',(-0.127464214162663,-0.161661175510215,
0.0396503721891881));
#28685=CARTESIAN_POINT('Ctrl Pts',(-0.137245145186447,-0.153445140223816,
0.0389628948817094));
#28686=CARTESIAN_POINT('Ctrl Pts',(-0.14618056856958,-0.144399504838744,
0.0382754175742306));
#28687=CARTESIAN_POINT('Ctrl Pts',(-0.155114959869761,-0.135354914266622,
0.0375880196735777));
#28688=CARTESIAN_POINT('Ctrl Pts',(-0.163203448204579,-0.125481542661584,
0.0369006217729247));
#28689=CARTESIAN_POINT('Ctrl Pts',(-0.170302958735799,-0.1149646809713,
0.0362132238722718));
#28690=CARTESIAN_POINT('Ctrl Pts',(-0.177418338475885,-0.104424311424518,
0.0355242894627552));
#28691=CARTESIAN_POINT('Ctrl Pts',(-0.183539892256841,-0.0932383261556052,
0.0348353550532384));
#28692=CARTESIAN_POINT('Ctrl Pts',(-0.188569123495992,-0.0816190007838447,
0.0341464206437218));
#28693=CARTESIAN_POINT('Ctrl Pts',(-0.190504940680171,-0.0771465697792584,
0.0338812407374307));
#28694=CARTESIAN_POINT('Ctrl Pts',(-0.192279431480133,-0.0726101451294261,
0.0336160608311397));
#28695=CARTESIAN_POINT('Ctrl Pts',(-0.193888937113424,-0.0680224645982971,
0.0333508809248486));
#28696=CARTESIAN_POINT('Ctrl Pts',(-0.198705199436606,-0.0542943530366855,
0.0325573602529624));
#28697=CARTESIAN_POINT('Ctrl Pts',(-0.202067611815247,-0.0400300622513279,
0.031763839581076));
#28698=CARTESIAN_POINT('Ctrl Pts',(-0.203883660505739,-0.0255230994156351,
0.0309703189091898));
#28699=CARTESIAN_POINT('Ctrl Pts',(-0.204934727938483,-0.0171269609946517,
0.0305110560382134));
#28700=CARTESIAN_POINT('Ctrl Pts',(-0.205468659503104,-0.00864994056524452,
0.0300517931672369));
#28701=CARTESIAN_POINT('Ctrl Pts',(-0.205474943816094,-0.000151949903191644,
0.0295925302962604));
#28702=CARTESIAN_POINT('Ctrl Pts',(-0.205288744110104,-0.000151770750953056,
0.0295925280537678));
#28703=CARTESIAN_POINT('Ctrl Pts',(-0.204996003270372,0.0451941134373501,
0.0271396589080337));
#28704=CARTESIAN_POINT('Ctrl Pts',(-0.16789984592073,0.159522204476035,
0.0209811363262054));
#28705=CARTESIAN_POINT('Ctrl Pts',(-0.00906163169318692,0.22853860958862,
0.0127119568072292));
#28706=CARTESIAN_POINT('Ctrl Pts',(0.0939899964509164,0.186303764936298,
0.00689564643398706));
#28707=CARTESIAN_POINT('Ctrl Pts',(0.124934343482292,0.162564573588643,
0.00478498949683932));
#28708=CARTESIAN_POINT('',(-0.205474920450601,0.000180806026586553,0.0354074719462324));
#28709=CARTESIAN_POINT('Ctrl Pts',(-0.205474920450601,0.000180806026586553,
0.0354074719462324));
#28710=CARTESIAN_POINT('Ctrl Pts',(-0.205462672789408,0.0140995191186828,
0.0346517512397107));
#28711=CARTESIAN_POINT('Ctrl Pts',(-0.204034908267823,0.0279571981809514,
0.0338960305331892));
#28712=CARTESIAN_POINT('Ctrl Pts',(-0.201235673998871,0.0415232360880032,
0.0331403098266677));
#28713=CARTESIAN_POINT('Ctrl Pts',(-0.198691911824772,0.0538511696458031,
0.0324535599648376));
#28714=CARTESIAN_POINT('Ctrl Pts',(-0.195002027539007,0.0659883377117587,
0.0317668101030073));
#28715=CARTESIAN_POINT('Ctrl Pts',(-0.190214170361878,0.0777080756327314,
0.0310800602411772));
#28716=CARTESIAN_POINT('Ctrl Pts',(-0.185436300195792,0.0894033673040152,
0.0303947428737176));
#28717=CARTESIAN_POINT('Ctrl Pts',(-0.17956525817496,0.100682133855508,
0.0297094255062579));
#28718=CARTESIAN_POINT('Ctrl Pts',(-0.172698732637008,0.111333388390775,
0.0290241081387983));
#28719=CARTESIAN_POINT('Ctrl Pts',(-0.165833097875624,0.121983261166387,
0.0283388796757852));
#28720=CARTESIAN_POINT('Ctrl Pts',(-0.157972665043853,0.132005029581892,
0.0276536512127722));
#28721=CARTESIAN_POINT('Ctrl Pts',(-0.1492600756121,0.141214041275187,0.0269684227497591));
#28722=CARTESIAN_POINT('Ctrl Pts',(-0.140548194533839,0.150422304254723,
0.0262832499973907));
#28723=CARTESIAN_POINT('Ctrl Pts',(-0.130984909061376,0.15881732859402,
0.0255980772450224));
#28724=CARTESIAN_POINT('Ctrl Pts',(-0.120749968207374,0.166251077599269,
0.024912904492654));
#28725=CARTESIAN_POINT('Ctrl Pts',(-0.110490930863035,0.173702328147871,
0.0242261186133666));
#28726=CARTESIAN_POINT('Ctrl Pts',(-0.0995578191178444,0.180187324520427,
0.0235393327340791));
#28727=CARTESIAN_POINT('Ctrl Pts',(-0.0881587200673234,0.185601766427724,
0.0228525468547917));
#28728=CARTESIAN_POINT('Ctrl Pts',(-0.083571117217974,0.187780825405233,
0.0225761477426559));
#28729=CARTESIAN_POINT('Ctrl Pts',(-0.0789082812909707,0.189787029962141,
0.0222997486305201));
#28730=CARTESIAN_POINT('Ctrl Pts',(-0.0741845676270748,0.191615828028334,
0.0220233495183842));
#28731=CARTESIAN_POINT('Ctrl Pts',(-0.0624085198732363,0.196174955632579,
0.0213342965030613));
#28732=CARTESIAN_POINT('Ctrl Pts',(-0.0501701202187604,0.199660157841503,
0.0206452434877385));
#28733=CARTESIAN_POINT('Ctrl Pts',(-0.0376873519293716,0.201989205477797,
0.0199561904724155));
#28734=CARTESIAN_POINT('Ctrl Pts',(-0.0252306758224384,0.204313384808082,
0.0192685777543551));
#28735=CARTESIAN_POINT('Ctrl Pts',(-0.0125314697797735,0.205485978497169,
0.0185809650362948));
#28736=CARTESIAN_POINT('Ctrl Pts',(0.000178736612729978,0.205474922261144,
0.0178933523182345));
#28737=CARTESIAN_POINT('Ctrl Pts',(0.0128864559775172,0.205463868188512,
0.017205874146525));
#28738=CARTESIAN_POINT('Ctrl Pts',(0.0256043115927967,0.204269578020358,
0.0165183959748154));
#28739=CARTESIAN_POINT('Ctrl Pts',(0.0380986165458339,0.201912037883563,
0.0158309178031059));
#28740=CARTESIAN_POINT('Ctrl Pts',(0.0505914779703075,0.199554770124988,
0.0151435190591342));
#28741=CARTESIAN_POINT('Ctrl Pts',(0.0628599977250734,0.196034701279311,
0.0144561203151623));
#28742=CARTESIAN_POINT('Ctrl Pts',(0.0746811072610426,0.19142285089107,
0.0137687215711906));
#28743=CARTESIAN_POINT('Ctrl Pts',(0.0865286391536204,0.186800692167962,
0.0130797863644452));
#28744=CARTESIAN_POINT('Ctrl Pts',(0.0979259823920605,0.18108224616592,
0.0123908511576998));
#28745=CARTESIAN_POINT('Ctrl Pts',(0.108671384715014,0.17438608249835,0.0117019159509544));
#28746=CARTESIAN_POINT('Ctrl Pts',(0.112807358996017,0.17180868614984,0.0114367403706702));
#28747=CARTESIAN_POINT('Ctrl Pts',(0.116847046830691,0.169086900231906,
0.0111715647903859));
#28748=CARTESIAN_POINT('Ctrl Pts',(0.120780194335444,0.166229119835522,
0.0109063892101017));
#28749=CARTESIAN_POINT('Ctrl Pts',(0.122269918345648,0.165146703255102,
0.0108059509660766));
#28750=CARTESIAN_POINT('Ctrl Pts',(0.123745850864902,0.164043706535222,
0.0107055127220516));
#28751=CARTESIAN_POINT('Ctrl Pts',(0.125207372047943,0.162920500888771,
0.0106050744780265));
#28752=CARTESIAN_POINT('Ctrl Pts',(0.125161044493633,0.162858663584037,
0.0806174252350173));
#28753=CARTESIAN_POINT('Ctrl Pts',(0.139948319312594,0.151719697155996,
0.0796143338432777));
#28754=CARTESIAN_POINT('Ctrl Pts',(0.202192621330403,0.0903875593842567,
0.074905589015444));
#28755=CARTESIAN_POINT('Ctrl Pts',(0.228035008840565,-0.083631262664263,
0.0664911907515159));
#28756=CARTESIAN_POINT('Ctrl Pts',(0.0533337265757384,-0.236956827852518,
0.0553742304432329));
#28757=CARTESIAN_POINT('Ctrl Pts',(-0.154992695350211,-0.17760232906673,
0.0450130024403464));
#28758=CARTESIAN_POINT('Ctrl Pts',(-0.20504063162631,-0.0541692048004282,
0.0383574278735543));
#28759=CARTESIAN_POINT('Ctrl Pts',(-0.205542551645511,0.00018022444937596,
0.0354075067428563));
#28760=CARTESIAN_POINT('Origin',(0.,0.,0.554592528053768));
#28761=CARTESIAN_POINT('',(0.125015612364501,0.162672938451339,0.150603574429178));
#28762=CARTESIAN_POINT('',(0.125207372047945,0.162920500888769,0.144794087791587));
#28763=CARTESIAN_POINT('',(0.125207372047944,0.16292050088877,0.554592528053768));
#28764=CARTESIAN_POINT('',(-0.205474993442675,-5.19108148716082E-5,0.0995925280506006));
#28765=CARTESIAN_POINT('Ctrl Pts',(0.125207372047945,0.16292050088877,0.144794087791587));
#28766=CARTESIAN_POINT('Ctrl Pts',(0.126533996279166,0.161900966006541,
0.144702886530283));
#28767=CARTESIAN_POINT('Ctrl Pts',(0.127847586394256,0.160865672653201,
0.144611685268979));
#28768=CARTESIAN_POINT('Ctrl Pts',(0.12914775512683,0.159814996075776,0.144520484007676));
#28769=CARTESIAN_POINT('Ctrl Pts',(0.138952052153233,0.151892066546959,
0.143832754613328));
#28770=CARTESIAN_POINT('Ctrl Pts',(0.148058839276438,0.143035853394179,
0.14314502521898));
#28771=CARTESIAN_POINT('Ctrl Pts',(0.156288532458628,0.133393666442333,
0.142457295824632));
#28772=CARTESIAN_POINT('Ctrl Pts',(0.164501105837628,0.123771537631085,
0.141770997078015));
#28773=CARTESIAN_POINT('Ctrl Pts',(0.171839594963137,0.113367283593476,
0.141084698331399));
#28774=CARTESIAN_POINT('Ctrl Pts',(0.17816111201773,0.102365002757808,0.140398399584782));
#28775=CARTESIAN_POINT('Ctrl Pts',(0.184481700913311,0.0913643373359736,
0.139712201604225));
#28776=CARTESIAN_POINT('Ctrl Pts',(0.189785143090681,0.079766544590134,
0.139026003623668));
#28777=CARTESIAN_POINT('Ctrl Pts',(0.193972586509944,0.0677835622230219,
0.138339805643111));
#28778=CARTESIAN_POINT('Ctrl Pts',(0.198159655731775,0.0558016506766435,
0.137653668982433));
#28779=CARTESIAN_POINT('Ctrl Pts',(0.201230661855283,0.0434354425276815,
0.136967532321755));
#28780=CARTESIAN_POINT('Ctrl Pts',(0.203136303503206,0.0309130688229653,
0.136281395661077));
#28781=CARTESIAN_POINT('Ctrl Pts',(0.205046352401837,0.0183617341431124,
0.135593672145762));
#28782=CARTESIAN_POINT('Ctrl Pts',(0.205785584821844,0.00565437702989593,
0.134905948630448));
#28783=CARTESIAN_POINT('Ctrl Pts',(0.205356555857814,-0.00697571438753253,
0.134218225115133));
#28784=CARTESIAN_POINT('Ctrl Pts',(0.205187141601162,-0.0119630642597618,
0.133946657976553));
#28785=CARTESIAN_POINT('Ctrl Pts',(0.204836135880033,-0.01693839824953,
0.133675090837974));
#28786=CARTESIAN_POINT('Ctrl Pts',(0.204305913300231,-0.0218876544097049,
0.133403523699394));
#28787=CARTESIAN_POINT('Ctrl Pts',(0.202963143048502,-0.034421473589077,
0.13271578936117));
#28788=CARTESIAN_POINT('Ctrl Pts',(0.200457982603897,-0.0468750981425169,
0.132028055022946));
#28789=CARTESIAN_POINT('Ctrl Pts',(0.196816867803737,-0.0590177615038569,
0.131340320684722));
#28790=CARTESIAN_POINT('Ctrl Pts',(0.193183326817346,-0.0711351671416734,
0.130654016889637));
#28791=CARTESIAN_POINT('Ctrl Pts',(0.188418696734644,-0.0829420542843885,
0.129967713094553));
#28792=CARTESIAN_POINT('Ctrl Pts',(0.182600220325673,-0.0942185499889263,
0.129281409299469));
#28793=CARTESIAN_POINT('Ctrl Pts',(0.176782597581181,-0.105493391249386,
0.128595206196238));
#28794=CARTESIAN_POINT('Ctrl Pts',(0.169911789447793,-0.116237206609658,
0.127909003093007));
#28795=CARTESIAN_POINT('Ctrl Pts',(0.162112304146814,-0.126252035505219,
0.127222799989776));
#28796=CARTESIAN_POINT('Ctrl Pts',(0.154313515265857,-0.136265970171596,
0.126536658157971));
#28797=CARTESIAN_POINT('Ctrl Pts',(0.145586764616251,-0.145550380111688,
0.125850516326165));
#28798=CARTESIAN_POINT('Ctrl Pts',(0.136097029331549,-0.15394016445401,
0.12516437449436));
#28799=CARTESIAN_POINT('Ctrl Pts',(0.126585347297815,-0.162349351707568,
0.124476645834035));
#28800=CARTESIAN_POINT('Ctrl Pts',(0.1163078453797,-0.169859254438693,0.123788917173711));
#28801=CARTESIAN_POINT('Ctrl Pts',(0.1054619457945,-0.176345551727958,0.123101188513387));
#28802=CARTESIAN_POINT('Ctrl Pts',(0.101179567784339,-0.178906591193676,
0.122829646805962));
#28803=CARTESIAN_POINT('Ctrl Pts',(0.0968088623768857,-0.181308553120973,
0.122558105098536));
#28804=CARTESIAN_POINT('Ctrl Pts',(0.0923629294268599,-0.183545811427798,
0.122286563391111));
#28805=CARTESIAN_POINT('Ctrl Pts',(0.0811031496119801,-0.189211896860714,
0.121598856250555));
#28806=CARTESIAN_POINT('Ctrl Pts',(0.0692806436434433,-0.193857829957916,
0.120911149109999));
#28807=CARTESIAN_POINT('Ctrl Pts',(0.0571036400178444,-0.197380723277914,
0.120223441969443));
#28808=CARTESIAN_POINT('Ctrl Pts',(0.0449519676547056,-0.200896288084425,
0.119537165434527));
#28809=CARTESIAN_POINT('Ctrl Pts',(0.0324480632690806,-0.203293141389066,
0.118850888899612));
#28810=CARTESIAN_POINT('Ctrl Pts',(0.0198185460416459,-0.204516994056228,
0.118164612364696));
#28811=CARTESIAN_POINT('Ctrl Pts',(0.00719087598648223,-0.205740667724726,
0.11747843620345));
#28812=CARTESIAN_POINT('Ctrl Pts',(-0.00556151550682495,-0.205791551073304,
0.116792260042204));
#28813=CARTESIAN_POINT('Ctrl Pts',(-0.0182047982369213,-0.204666951279763,
0.116106083880958));
#28814=CARTESIAN_POINT('Ctrl Pts',(-0.03084695479573,-0.203542451657359,
0.115419968839272));
#28815=CARTESIAN_POINT('Ctrl Pts',(-0.0433791623346208,-0.201242777741841,
0.114733853797587));
#28816=CARTESIAN_POINT('Ctrl Pts',(-0.0555732645159496,-0.197817056635772,
0.114047738755902));
#28817=CARTESIAN_POINT('Ctrl Pts',(-0.0677955817975969,-0.194383408987574,
0.113360036159476));
#28818=CARTESIAN_POINT('Ctrl Pts',(-0.079677415121298,-0.189818803845433,
0.11267233356305));
#28819=CARTESIAN_POINT('Ctrl Pts',(-0.0910072878395048,-0.184221739176183,
0.111984630966624));
#28820=CARTESIAN_POINT('Ctrl Pts',(-0.0954831384146339,-0.18201062650599,
0.111712955005358));
#28821=CARTESIAN_POINT('Ctrl Pts',(-0.0998731142906491,-0.179638895026068,
0.111441279044093));
#28822=CARTESIAN_POINT('Ctrl Pts',(-0.10416536863244,-0.177114515505274,
0.111169603082828));
#28823=CARTESIAN_POINT('Ctrl Pts',(-0.115031174605359,-0.170724069858124,
0.110481857658734));
#28824=CARTESIAN_POINT('Ctrl Pts',(-0.125344713458378,-0.163307637310166,
0.10979411223464));
#28825=CARTESIAN_POINT('Ctrl Pts',(-0.134906633517487,-0.154984437470278,
0.109106366810546));
#28826=CARTESIAN_POINT('Ctrl Pts',(-0.144448659959639,-0.146678554084455,
0.108420052243847));
#28827=CARTESIAN_POINT('Ctrl Pts',(-0.153241477344281,-0.137470154345247,
0.107733737677149));
#28828=CARTESIAN_POINT('Ctrl Pts',(-0.161116603529287,-0.127520256007376,
0.10704742311045));
#28829=CARTESIAN_POINT('Ctrl Pts',(-0.168990567313194,-0.117571826315528,
0.106361209846612));
#28830=CARTESIAN_POINT('Ctrl Pts',(-0.17594653596607,-0.106882763030196,
0.105674996582773));
#28831=CARTESIAN_POINT('Ctrl Pts',(-0.181855475767578,-0.0956481131980548,
0.104988783318935));
#28832=CARTESIAN_POINT('Ctrl Pts',(-0.187763885043637,-0.084414472052386,
0.104302631665743));
#28833=CARTESIAN_POINT('Ctrl Pts',(-0.192625071016067,-0.0726361185384288,
0.103616480012551));
#28834=CARTESIAN_POINT('Ctrl Pts',(-0.196356620124702,-0.0605314245512496,
0.102930328359358));
#28835=CARTESIAN_POINT('Ctrl Pts',(-0.200096795289964,-0.0483987486796708,
0.102242590559812));
#28836=CARTESIAN_POINT('Ctrl Pts',(-0.20270192231038,-0.0359390704211971,
0.101554852760265));
#28837=CARTESIAN_POINT('Ctrl Pts',(-0.204140116154794,-0.0233835113126177,
0.100867114960718));
#28838=CARTESIAN_POINT('Ctrl Pts',(-0.204707856207942,-0.0184270905746907,
0.100595624231994));
#28839=CARTESIAN_POINT('Ctrl Pts',(-0.205094320000884,-0.0134557812286958,
0.10032413350327));
#28840=CARTESIAN_POINT('Ctrl Pts',(-0.205299781453641,-0.00848382932921304,
0.100052642774545));
#28841=CARTESIAN_POINT('Ctrl Pts',(-0.205415851517875,-0.0056750553786874,
0.0998992712009528));
#28842=CARTESIAN_POINT('Ctrl Pts',(-0.205474283030533,-0.00286388298952928,
0.0997458996273603));
#28843=CARTESIAN_POINT('Ctrl Pts',(-0.20547499344266,-5.19108729419778E-5,
0.0995925280537679));
#28844=CARTESIAN_POINT('Ctrl Pts',(-0.205474993442675,-5.19108148716082E-5,
0.0995925280506004));
#28845=CARTESIAN_POINT('Ctrl Pts',(-0.205478158112058,0.0124745814452694,
0.0989093036977783));
#28846=CARTESIAN_POINT('Ctrl Pts',(-0.204331518578654,0.0250472595540262,
0.0982260793449564));
#28847=CARTESIAN_POINT('Ctrl Pts',(-0.202035879687132,0.0374363318722169,
0.0975428549921343));
#28848=CARTESIAN_POINT('Ctrl Pts',(-0.199625866061445,0.0504426601787855,
0.0968255906149783));
#28849=CARTESIAN_POINT('Ctrl Pts',(-0.195949068210376,0.0632455487890031,
0.0961083262378224));
#28850=CARTESIAN_POINT('Ctrl Pts',(-0.191068136702914,0.0755840112846409,
0.0953910618606664));
#28851=CARTESIAN_POINT('Ctrl Pts',(-0.18642882519258,0.0873116847806354,
0.0947093041109819));
#28852=CARTESIAN_POINT('Ctrl Pts',(-0.180702384870152,0.0986190302533711,
0.0940275463612974));
#28853=CARTESIAN_POINT('Ctrl Pts',(-0.173993039971578,0.109299577613315,
0.093345788611613));
#28854=CARTESIAN_POINT('Ctrl Pts',(-0.167283223855812,0.119980875099776,
0.0926639829800598));
#28855=CARTESIAN_POINT('Ctrl Pts',(-0.159590862137391,0.130034563297859,
0.0919821773485063));
#28856=CARTESIAN_POINT('Ctrl Pts',(-0.151063415701073,0.13928323682958,
0.0913003717169531));
#28857=CARTESIAN_POINT('Ctrl Pts',(-0.142516961859761,0.148552525358391,
0.0906170463624837));
#28858=CARTESIAN_POINT('Ctrl Pts',(-0.133132359550586,0.157012629513546,
0.0899337210080143));
#28859=CARTESIAN_POINT('Ctrl Pts',(-0.123092726545284,0.164524029541729,
0.0892503956535449));
#28860=CARTESIAN_POINT('Ctrl Pts',(-0.121551437864583,0.165677182832646,
0.0891454912577842));
#28861=CARTESIAN_POINT('Ctrl Pts',(-0.119994765657942,0.166808060439192,
0.0890405868620236));
#28862=CARTESIAN_POINT('Ctrl Pts',(-0.118423428086134,0.167916250867295,
0.088935682466263));
#28863=CARTESIAN_POINT('Ctrl Pts',(-0.108124263520439,0.175179766864068,
0.088248097790005));
#28864=CARTESIAN_POINT('Ctrl Pts',(-0.0971182332163936,0.181517662625345,
0.087560513113747));
#28865=CARTESIAN_POINT('Ctrl Pts',(-0.0855960337030366,0.186797469574158,
0.086872928437489));
#28866=CARTESIAN_POINT('Ctrl Pts',(-0.0740978098127389,0.192066290195137,
0.0861867745011692));
#28867=CARTESIAN_POINT('Ctrl Pts',(-0.0620862963673555,0.196280968083181,
0.0855006205648494));
#28868=CARTESIAN_POINT('Ctrl Pts',(-0.0497775549847631,0.199354384563618,
0.0848144666285295));
#28869=CARTESIAN_POINT('Ctrl Pts',(-0.0374705848010918,0.202427358786656,
0.0841284114281465));
#28870=CARTESIAN_POINT('Ctrl Pts',(-0.024867298253071,0.204359142474981,
0.0834423562277635));
#28871=CARTESIAN_POINT('Ctrl Pts',(-0.0121985044514171,0.205112583997542,
0.0827563010273805));
#28872=CARTESIAN_POINT('Ctrl Pts',(0.000469175482691606,0.205865959275907,
0.0820703061464434));
#28873=CARTESIAN_POINT('Ctrl Pts',(0.0132014858459238,0.205441171173303,
0.0813843112655062));
#28874=CARTESIAN_POINT('Ctrl Pts',(0.0257655867619812,0.20385315833661,
0.080698316384569));
#28875=CARTESIAN_POINT('Ctrl Pts',(0.0383588268137166,0.202261462520783,
0.0800107305184875));
#28876=CARTESIAN_POINT('Ctrl Pts',(0.0507822274498415,0.199501323851069,
0.0793231446524059));
#28877=CARTESIAN_POINT('Ctrl Pts',(0.0628121673557659,0.195638971723609,
0.0786355587863244));
#28878=CARTESIAN_POINT('Ctrl Pts',(0.0675759338595545,0.194109509080029,
0.0783632799102093));
#28879=CARTESIAN_POINT('Ctrl Pts',(0.0722781904676448,0.192407754399022,
0.0780910010340942));
#28880=CARTESIAN_POINT('Ctrl Pts',(0.0769059571795283,0.190539889197251,
0.0778187221579791));
#28881=CARTESIAN_POINT('Ctrl Pts',(0.0885973767354331,0.185820983274074,
0.0771308468230583));
#28882=CARTESIAN_POINT('Ctrl Pts',(0.0998936717960377,0.180005521932965,
0.0764429714881376));
#28883=CARTESIAN_POINT('Ctrl Pts',(0.110580041473782,0.173182071972409,
0.0757550961532168));
#28884=CARTESIAN_POINT('Ctrl Pts',(0.115596874343119,0.169978728921711,
0.0754321655702121));
#28885=CARTESIAN_POINT('Ctrl Pts',(0.120479518615123,0.166553942355756,
0.0751092349872075));
#28886=CARTESIAN_POINT('Ctrl Pts',(0.125207372047944,0.16292050088877,0.0747863044042028));
#28887=CARTESIAN_POINT('',(-0.205137705209698,-7.29564938455052E-7,0.105407471946233));
#28888=CARTESIAN_POINT('Ctrl Pts',(-0.205137705209698,-7.29564938455052E-7,
0.105407471946233));
#28889=CARTESIAN_POINT('Ctrl Pts',(-0.205136713680842,0.0343461846931921,
0.103552338522943));
#28890=CARTESIAN_POINT('Ctrl Pts',(-0.180678665067047,0.137302931168816,
0.0979915516635594));
#28891=CARTESIAN_POINT('Ctrl Pts',(-0.0354393139172565,0.230872355804693,
0.0897282027598211));
#28892=CARTESIAN_POINT('Ctrl Pts',(0.0853206790052409,0.192869635794213,
0.0833199872793719));
#28893=CARTESIAN_POINT('Ctrl Pts',(0.125161044493633,0.162858663584037,
0.0806174252350173));
#28894=CARTESIAN_POINT('Ctrl Pts',(0.125015612364502,0.162672938451338,
0.150603574429178));
#28895=CARTESIAN_POINT('Ctrl Pts',(0.155720339957463,0.138903214455256,
0.14850568725595));
#28896=CARTESIAN_POINT('Ctrl Pts',(0.223157023264117,0.0501045043133742,
0.142702146646629));
#28897=CARTESIAN_POINT('Ctrl Pts',(0.193712423773769,-0.146520715699965,
0.133192952601213));
#28898=CARTESIAN_POINT('Ctrl Pts',(-0.0181106010581924,-0.24220824221319,
0.12207599229293));
#28899=CARTESIAN_POINT('Ctrl Pts',(-0.18076764144762,-0.137130727182572,
0.112814165407936));
#28900=CARTESIAN_POINT('Ctrl Pts',(-0.205138694272785,-0.0342622287190314,
0.107257991959037));
#28901=CARTESIAN_POINT('Ctrl Pts',(-0.205137705209698,-7.29564938455052E-7,
0.105407471946233));
#28902=CARTESIAN_POINT('Origin',(0.,0.,0.554592528053768));
#28903=CARTESIAN_POINT('',(0.125207372047944,0.16292050088877,0.220601534780829));
#28904=CARTESIAN_POINT('',(0.125103714720563,0.162782948353132,0.214801399208945));
#28905=CARTESIAN_POINT('',(0.125207372047944,0.16292050088877,0.554592528053768));
#28906=CARTESIAN_POINT('',(-0.205474914417448,0.000187537043271921,0.16959252654344));
#28907=CARTESIAN_POINT('Ctrl Pts',(0.125103714720543,0.162782948353147,
0.214801399208946));
#28908=CARTESIAN_POINT('Ctrl Pts',(0.142694629810408,0.149496203490235,
0.213608348091755));
#28909=CARTESIAN_POINT('Ctrl Pts',(0.206176667207859,0.0838646344828523,
0.20870964353847));
#28910=CARTESIAN_POINT('Ctrl Pts',(0.223448082612567,-0.0952038262864637,
0.20010528554909));
#28911=CARTESIAN_POINT('Ctrl Pts',(0.0411315804786337,-0.23937629702844,
0.188988325240808));
#28912=CARTESIAN_POINT('Ctrl Pts',(-0.160132400758511,-0.170716737438922,
0.1788174060757));
#28913=CARTESIAN_POINT('Ctrl Pts',(-0.204971567375627,-0.0507230854143627,
0.172352140346687));
#28914=CARTESIAN_POINT('Ctrl Pts',(-0.205429022845128,0.000187467295045865,
0.169592528053768));
#28915=CARTESIAN_POINT('Ctrl Pts',(-0.205474914417448,0.000187537043271921,
0.16959252654344));
#28916=CARTESIAN_POINT('Ctrl Pts',(-0.20546003488534,0.0164902926646276,
0.168709023204908));
#28917=CARTESIAN_POINT('Ctrl Pts',(-0.203501056447997,0.0327051355942583,
0.167825519866375));
#28918=CARTESIAN_POINT('Ctrl Pts',(-0.199682357505078,0.048445141409787,
0.166942016527842));
#28919=CARTESIAN_POINT('Ctrl Pts',(-0.199412057308611,0.0495592713079335,
0.166879479226642));
#28920=CARTESIAN_POINT('Ctrl Pts',(-0.199132458627398,0.0506710315391687,
0.166816941925442));
#28921=CARTESIAN_POINT('Ctrl Pts',(-0.19884360010305,0.0517802889433662,
0.166754404624242));
#28922=CARTESIAN_POINT('Ctrl Pts',(-0.195666995000812,0.0639788997955671,
0.166066675880494));
#28923=CARTESIAN_POINT('Ctrl Pts',(-0.191352556686954,0.0759267682013015,
0.165378947136745));
#28924=CARTESIAN_POINT('Ctrl Pts',(-0.185960463086372,0.0873995525944041,
0.164691218392996));
#28925=CARTESIAN_POINT('Ctrl Pts',(-0.180579586019762,0.0988484715123463,
0.164004920249936));
#28926=CARTESIAN_POINT('Ctrl Pts',(-0.174125800579575,0.109823461849753,
0.163318622106875));
#28927=CARTESIAN_POINT('Ctrl Pts',(-0.166707929573821,0.120118449216638,
0.162632323963815));
#28928=CARTESIAN_POINT('Ctrl Pts',(-0.159291146875126,0.130411926162617,
0.161946126510442));
#28929=CARTESIAN_POINT('Ctrl Pts',(-0.150911025889177,0.140024870067992,
0.16125992905707));
#28930=CARTESIAN_POINT('Ctrl Pts',(-0.141719906483916,0.148779849882939,
0.160573731603697));
#28931=CARTESIAN_POINT('Ctrl Pts',(-0.132529607834903,0.157534047888397,
0.159887595426957));
#28932=CARTESIAN_POINT('Ctrl Pts',(-0.12252909774965,0.165429854936943,
0.159201459250217));
#28933=CARTESIAN_POINT('Ctrl Pts',(-0.111905896277347,0.172328308769522,
0.158515323073477));
#28934=CARTESIAN_POINT('Ctrl Pts',(-0.101258124978244,0.179242717662003,
0.157827599969569));
#28935=CARTESIAN_POINT('Ctrl Pts',(-0.0899855450072962,0.185154746955193,
0.157139876865662));
#28936=CARTESIAN_POINT('Ctrl Pts',(-0.0783017522917341,0.189970553541974,
0.156452153761754));
#28937=CARTESIAN_POINT('Ctrl Pts',(-0.0736880270710313,0.191872231263273,
0.156180583946489));
#28938=CARTESIAN_POINT('Ctrl Pts',(-0.0690103880702461,0.193603509023575,
0.155909014131224));
#28939=CARTESIAN_POINT('Ctrl Pts',(-0.0642826260963226,0.195160753245012,
0.155637444315959));
#28940=CARTESIAN_POINT('Ctrl Pts',(-0.0523099317195422,0.199104354728359,
0.154949714599857));
#28941=CARTESIAN_POINT('Ctrl Pts',(-0.0399311091990029,0.201955891739313,
0.154261984883755));
#28942=CARTESIAN_POINT('Ctrl Pts',(-0.0273673002084757,0.2036443137048,
0.153574255167652));
#28943=CARTESIAN_POINT('Ctrl Pts',(-0.0148297791737362,0.205329202891175,
0.152887964426656));
#28944=CARTESIAN_POINT('Ctrl Pts',(-0.00210887860604118,0.20585562065462,
0.152201673685659));
#28945=CARTESIAN_POINT('Ctrl Pts',(0.0105632472606296,0.205203297810515,
0.151515382944663));
#28946=CARTESIAN_POINT('Ctrl Pts',(0.023232324583079,0.204551131896278,
0.15082925730522));
#28947=CARTESIAN_POINT('Ctrl Pts',(0.0358517861306209,0.202720787990091,
0.150143131665778));
#28948=CARTESIAN_POINT('Ctrl Pts',(0.0481900208858049,0.199744080042503,
0.149457006026335));
#28949=CARTESIAN_POINT('Ctrl Pts',(0.060527095013038,0.196767652106643,
0.148770944929075));
#28950=CARTESIAN_POINT('Ctrl Pts',(0.072582160107258,0.192645300831173,
0.148084883831814));
#28951=CARTESIAN_POINT('Ctrl Pts',(0.084136856198351,0.187459235712882,
0.147398822734554));
#28952=CARTESIAN_POINT('Ctrl Pts',(0.0957157812287071,0.182262295980861,
0.146711323041893));
#28953=CARTESIAN_POINT('Ctrl Pts',(0.106791480451592,0.175997600872094,
0.146023823349231));
#28954=CARTESIAN_POINT('Ctrl Pts',(0.117169482386542,0.168793625538021,
0.14533632365657));
#28955=CARTESIAN_POINT('Ctrl Pts',(0.119897883536421,0.166899683456647,
0.145155578368242));
#28956=CARTESIAN_POINT('Ctrl Pts',(0.122578229909477,0.164941044504228,
0.144974833079914));
#28957=CARTESIAN_POINT('Ctrl Pts',(0.125207372047945,0.16292050088877,0.144794087791587));
#28958=CARTESIAN_POINT('',(-0.205474918801311,-0.000182670727437368,0.175407471946233));
#28959=CARTESIAN_POINT('Ctrl Pts',(-0.205537738049557,-0.000182131345404107,
0.175407439637765));
#28960=CARTESIAN_POINT('Ctrl Pts',(-0.205035768459691,0.0542506832901805,
0.172452904267196));
#28961=CARTESIAN_POINT('Ctrl Pts',(-0.154875619861323,0.177771679933206,
0.165792715460535));
#28962=CARTESIAN_POINT('Ctrl Pts',(0.0114351922188548,0.224924155783168,
0.157524760391006));
#28963=CARTESIAN_POINT('Ctrl Pts',(0.101484306313129,0.180889437797084,
0.152211340692044));
#28964=CARTESIAN_POINT('Ctrl Pts',(0.125015612364502,0.162672938451338,
0.150603574429178));
#28965=CARTESIAN_POINT('Ctrl Pts',(0.125207372047944,0.16292050088877,0.220601534780829));
#28966=CARTESIAN_POINT('Ctrl Pts',(0.135229999383183,0.155217929249134,
0.219914936476142));
#28967=CARTESIAN_POINT('Ctrl Pts',(0.144564381930118,0.146567701750036,
0.219228338171454));
#28968=CARTESIAN_POINT('Ctrl Pts',(0.153031143228616,0.137118360649268,
0.218541739866767));
#28969=CARTESIAN_POINT('Ctrl Pts',(0.161494455183014,0.127672869193935,
0.217855421281057));
#28970=CARTESIAN_POINT('Ctrl Pts',(0.169090227725395,0.117429513005291,
0.217169102695347));
#28971=CARTESIAN_POINT('Ctrl Pts',(0.17567590576567,0.106573691680506,0.216482784109637));
#28972=CARTESIAN_POINT('Ctrl Pts',(0.182259370136659,0.0957215193646887,
0.215796696218832));
#28973=CARTESIAN_POINT('Ctrl Pts',(0.187832975118639,0.0842580367541301,
0.215110608328027));
#28974=CARTESIAN_POINT('Ctrl Pts',(0.192298948011159,0.0723953742914676,
0.214424520437223));
#28975=CARTESIAN_POINT('Ctrl Pts',(0.196775565953506,0.0605044361011993,
0.213736797193952));
#28976=CARTESIAN_POINT('Ctrl Pts',(0.200139011911504,0.0482132446836958,
0.213049073950681));
#28977=CARTESIAN_POINT('Ctrl Pts',(0.202340970147259,0.0357506283142815,
0.21236135070741));
#28978=CARTESIAN_POINT('Ctrl Pts',(0.203781438193507,0.027597884832918,
0.211911458724671));
#28979=CARTESIAN_POINT('Ctrl Pts',(0.204725906820054,0.0193720658313528,
0.211461566741931));
#28980=CARTESIAN_POINT('Ctrl Pts',(0.205172899463256,0.0111380856003394,
0.211011674759192));
#28981=CARTESIAN_POINT('Ctrl Pts',(0.205856195198212,-0.00144879621779465,
0.210323946946057));
#28982=CARTESIAN_POINT('Ctrl Pts',(0.205379296652322,-0.0141428135166041,
0.209636219132922));
#28983=CARTESIAN_POINT('Ctrl Pts',(0.203731311683629,-0.0267119498477401,
0.208948491319788));
#28984=CARTESIAN_POINT('Ctrl Pts',(0.202086754839864,-0.0392549399637114,
0.208262194112456));
#28985=CARTESIAN_POINT('Ctrl Pts',(0.199275985054326,-0.0516727063359742,
0.207575896905125));
#28986=CARTESIAN_POINT('Ctrl Pts',(0.195340006274478,-0.0637358421430748,
0.206889599697793));
#28987=CARTESIAN_POINT('Ctrl Pts',(0.191404604920815,-0.075797208232684,
0.206203403173418));
#28988=CARTESIAN_POINT('Ctrl Pts',(0.186344545251388,-0.0875032115397956,
0.205517206649042));
#28989=CARTESIAN_POINT('Ctrl Pts',(0.180250997610476,-0.0986384990023071,
0.204831010124667));
#28990=CARTESIAN_POINT('Ctrl Pts',(0.17415799409207,-0.109772792140843,
0.204144874874117));
#28991=CARTESIAN_POINT('Ctrl Pts',(0.167032122503542,-0.120335723462707,
0.203458739623567));
#28992=CARTESIAN_POINT('Ctrl Pts',(0.15900976532022,-0.130137889017029,
0.202772604373016));
#28993=CARTESIAN_POINT('Ctrl Pts',(0.150968853384569,-0.139962725807498,
0.202084882173724));
#28994=CARTESIAN_POINT('Ctrl Pts',(0.142027910315271,-0.149022652279799,
0.201397159974432));
#28995=CARTESIAN_POINT('Ctrl Pts',(0.13236187985571,-0.157163317558718,
0.20070943777514));
#28996=CARTESIAN_POINT('Ctrl Pts',(0.128544863587495,-0.16037798276526,
0.20043786333373));
#28997=CARTESIAN_POINT('Ctrl Pts',(0.12461513953985,-0.163449748249725,
0.200166288892319));
#28998=CARTESIAN_POINT('Ctrl Pts',(0.120584741148151,-0.166370958485048,
0.199894714450909));
#28999=CARTESIAN_POINT('Ctrl Pts',(0.110378272528381,-0.173768549914217,
0.19920698690023));
#29000=CARTESIAN_POINT('Ctrl Pts',(0.0994528298630109,-0.180249297313827,
0.19851925934955));
#29001=CARTESIAN_POINT('Ctrl Pts',(0.0879974741651207,-0.185678270579944,
0.19783153179887));
#29002=CARTESIAN_POINT('Ctrl Pts',(0.076565947853254,-0.191095950517152,
0.197145234856346));
#29003=CARTESIAN_POINT('Ctrl Pts',(0.0646074384906068,-0.195465765742606,
0.196458937913822));
#29004=CARTESIAN_POINT('Ctrl Pts',(0.0523369473541958,-0.198697809667455,
0.195772640971298));
#29005=CARTESIAN_POINT('Ctrl Pts',(0.0400682563455929,-0.201929379439144,
0.19508644471115));
#29006=CARTESIAN_POINT('Ctrl Pts',(0.0274884973790633,-0.204023243709893,
0.194400248451003));
#29007=CARTESIAN_POINT('Ctrl Pts',(0.0148280576884289,-0.204939269858631,
0.193714052190855));
#29008=CARTESIAN_POINT('Ctrl Pts',(0.0021687485099159,-0.205855214210946,
0.193027917204503));
#29009=CARTESIAN_POINT('Ctrl Pts',(-0.0105703625229801,-0.20559349116586,
0.192341782218151));
#29010=CARTESIAN_POINT('Ctrl Pts',(-0.0231561837545491,-0.204166027484804,
0.191655647231799));
#29011=CARTESIAN_POINT('Ctrl Pts',(-0.0357711145876626,-0.202735262239375,
0.190967925291708));
#29012=CARTESIAN_POINT('Ctrl Pts',(-0.0482311949624943,-0.200133530206466,
0.190280203351617));
#29013=CARTESIAN_POINT('Ctrl Pts',(-0.0603118844336391,-0.196424164045729,
0.189592481411526));
#29014=CARTESIAN_POINT('Ctrl Pts',(-0.0650824496700984,-0.194959365757686,
0.189320905655226));
#29015=CARTESIAN_POINT('Ctrl Pts',(-0.0697940336714093,-0.193322389566768,
0.189049329898927));
#29016=CARTESIAN_POINT('Ctrl Pts',(-0.0744336798374629,-0.191519197290648,
0.188777754142627));
#29017=CARTESIAN_POINT('Ctrl Pts',(-0.0861829337940887,-0.186952865457034,
0.188090026584311));
#29018=CARTESIAN_POINT('Ctrl Pts',(-0.0975515135574834,-0.181285346209476,
0.187402299025996));
#29019=CARTESIAN_POINT('Ctrl Pts',(-0.108323544963334,-0.174602363190126,
0.18671457146768));
#29020=CARTESIAN_POINT('Ctrl Pts',(-0.119073168379992,-0.167933282117922,
0.186028274520835));
#29021=CARTESIAN_POINT('Ctrl Pts',(-0.129227940214968,-0.160253318696065,
0.185341977573991));
#29022=CARTESIAN_POINT('Ctrl Pts',(-0.13859575768312,-0.151694401931126,
0.184655680627146));
#29023=CARTESIAN_POINT('Ctrl Pts',(-0.147962200789884,-0.143136740852985,
0.183969484367577));
#29024=CARTESIAN_POINT('Ctrl Pts',(-0.156541249448778,-0.133700930003651,
0.183283288108009));
#29025=CARTESIAN_POINT('Ctrl Pts',(-0.16417428565667,-0.123558810103214,
0.18259709184844));
#29026=CARTESIAN_POINT('Ctrl Pts',(-0.171806640242344,-0.113417595883566,
0.181910956865486));
#29027=CARTESIAN_POINT('Ctrl Pts',(-0.178492649406469,-0.102570903692749,
0.181224821882532));
#29028=CARTESIAN_POINT('Ctrl Pts',(-0.184115975112121,-0.091221068473861,
0.180538686899578));
#29029=CARTESIAN_POINT('Ctrl Pts',(-0.189752306909373,-0.0798449824197511,
0.179850964967031));
#29030=CARTESIAN_POINT('Ctrl Pts',(-0.194320717629835,-0.0679642316562059,
0.179163243034484));
#29031=CARTESIAN_POINT('Ctrl Pts',(-0.197752701812011,-0.0558018328646087,
0.178475521101937));
#29032=CARTESIAN_POINT('Ctrl Pts',(-0.199107964243351,-0.0509990012423567,
0.178203945346073));
#29033=CARTESIAN_POINT('Ctrl Pts',(-0.200286569711164,-0.0461523936391531,
0.177932369590209));
#29034=CARTESIAN_POINT('Ctrl Pts',(-0.201286504152218,-0.0412761295566736,
0.177660793834344));
#29035=CARTESIAN_POINT('Ctrl Pts',(-0.20405206049521,-0.0277896623346762,
0.176909686538307));
#29036=CARTESIAN_POINT('Ctrl Pts',(-0.205462620446207,-0.0140163240550913,
0.17615857924227));
#29037=CARTESIAN_POINT('Ctrl Pts',(-0.205474918801311,-0.000182670727437368,
0.175407471946233));
#29038=CARTESIAN_POINT('Origin',(0.,0.,0.554592528053768));
#29039=CARTESIAN_POINT('',(0.12529644997826,0.163038483752229,0.290616425505885));
#29040=CARTESIAN_POINT('',(0.125045885691725,0.162713195961813,0.284785992558171));
#29041=CARTESIAN_POINT('',(0.125207372047944,0.16292050088877,0.554592528053768));
#29042=CARTESIAN_POINT('',(-0.205152667291151,-5.77023530759641E-5,0.239592528053768));
#29043=CARTESIAN_POINT('Ctrl Pts',(0.125045885691731,0.162713195961808,
0.284785992558171));
#29044=CARTESIAN_POINT('Ctrl Pts',(0.158439081624707,0.136730312047757,
0.282498664274471));
#29045=CARTESIAN_POINT('Ctrl Pts',(0.22621726887686,0.0424891423794237,
0.276505682554676));
#29046=CARTESIAN_POINT('Ctrl Pts',(0.185952226875698,-0.156251740320434,
0.266807047398788));
#29047=CARTESIAN_POINT('Ctrl Pts',(-0.030494276369136,-0.240962440043193,
0.255690087090504));
#29048=CARTESIAN_POINT('Ctrl Pts',(-0.18432786741861,-0.130018191841,0.246618580642165));
#29049=CARTESIAN_POINT('Ctrl Pts',(-0.205229924998058,-0.0307899101733451,
0.241252727629919));
#29050=CARTESIAN_POINT('Ctrl Pts',(-0.205152667291151,-5.77023530759641E-5,
0.239592528053768));
#29051=CARTESIAN_POINT('Ctrl Pts',(-0.205152667291151,-5.77023530759641E-5,
0.239592528053768));
#29052=CARTESIAN_POINT('Ctrl Pts',(-0.205057481701977,0.0378060063320381,
0.237547074193825));
#29053=CARTESIAN_POINT('Ctrl Pts',(-0.17685871883546,0.144397474870061,
0.231795966897788));
#29054=CARTESIAN_POINT('Ctrl Pts',(-0.0270112794014323,0.230407377050097,
0.223532257282847));
#29055=CARTESIAN_POINT('Ctrl Pts',(0.088056706918825,0.190765241376624,
0.21731400152785));
#29056=CARTESIAN_POINT('Ctrl Pts',(0.125103714720543,0.162782948353147,
0.214801399208946));
#29057=CARTESIAN_POINT('',(-0.205474970233635,0.00011060057405079,0.245407471946232));
#29058=CARTESIAN_POINT('Ctrl Pts',(-0.205474970233635,0.00011060057405079,
0.245407471946232));
#29059=CARTESIAN_POINT('Ctrl Pts',(-0.205471529321227,0.00650316571769436,
0.245059166525502));
#29060=CARTESIAN_POINT('Ctrl Pts',(-0.205169794342766,0.0128875158726893,
0.244710861104771));
#29061=CARTESIAN_POINT('Ctrl Pts',(-0.204571895687036,0.0192435734730444,
0.244362555684041));
#29062=CARTESIAN_POINT('Ctrl Pts',(-0.203391345348354,0.0317936032830672,
0.243674826955321));
#29063=CARTESIAN_POINT('Ctrl Pts',(-0.201047484118304,0.0442784848425534,
0.242987098226601));
#29064=CARTESIAN_POINT('Ctrl Pts',(-0.197563758380479,0.0564671320289918,
0.242299369497881));
#29065=CARTESIAN_POINT('Ctrl Pts',(-0.194087279374658,0.0686304247913778,
0.241613071359903));
#29066=CARTESIAN_POINT('Ctrl Pts',(-0.189475806558603,0.0804978629125803,
0.240926773221925));
#29067=CARTESIAN_POINT('Ctrl Pts',(-0.183803729986763,0.0918485953510078,
0.240240475083948));
#29068=CARTESIAN_POINT('Ctrl Pts',(-0.178132485468645,0.103197662716856,
0.239554277621077));
#29069=CARTESIAN_POINT('Ctrl Pts',(-0.171401289818514,0.114029381398208,
0.238868080158207));
#29070=CARTESIAN_POINT('Ctrl Pts',(-0.16373207813732,0.124144199275821,
0.238181882695337));
#29071=CARTESIAN_POINT('Ctrl Pts',(-0.156063551213915,0.134258114035796,
0.237495746500701));
#29072=CARTESIAN_POINT('Ctrl Pts',(-0.147457716636604,0.143654580501278,
0.236809610306065));
#29073=CARTESIAN_POINT('Ctrl Pts',(-0.138077400088184,0.152166380024918,
0.236123474111429));
#29074=CARTESIAN_POINT('Ctrl Pts',(-0.128675388147814,0.160697866179164,
0.235435750977419));
#29075=CARTESIAN_POINT('Ctrl Pts',(-0.118495998745998,0.168340063270647,
0.234748027843409));
#29076=CARTESIAN_POINT('Ctrl Pts',(-0.107735027333294,0.17496610960553,
0.234060304709399));
#29077=CARTESIAN_POINT('Ctrl Pts',(-0.103485708862233,0.177582618840717,
0.233788734931519));
#29078=CARTESIAN_POINT('Ctrl Pts',(-0.0991459938811956,0.180041173774481,
0.233517165153638));
#29079=CARTESIAN_POINT('Ctrl Pts',(-0.094728912604613,0.182335977639487,
0.233245595375758));
#29080=CARTESIAN_POINT('Ctrl Pts',(-0.0835430244141027,0.188147376127716,
0.232557867670271));
#29081=CARTESIAN_POINT('Ctrl Pts',(-0.0717812449575055,0.192945918580908,
0.231870139964785));
#29082=CARTESIAN_POINT('Ctrl Pts',(-0.0596504680101255,0.196626034113423,
0.231182412259298));
#29083=CARTESIAN_POINT('Ctrl Pts',(-0.047544925318993,0.200298494326022,
0.230496115154442));
#29084=CARTESIAN_POINT('Ctrl Pts',(-0.035072706489126,0.202856826392769,
0.229809818049586));
#29085=CARTESIAN_POINT('Ctrl Pts',(-0.0224597215775749,0.204243816385363,
0.22912352094473));
#29086=CARTESIAN_POINT('Ctrl Pts',(-0.00984858687894811,0.205630602918836,
0.228437324513567));
#29087=CARTESIAN_POINT('Ctrl Pts',(0.00290241978708712,0.205846247203182,
0.227751128082404));
#29088=CARTESIAN_POINT('Ctrl Pts',(0.0155595115836494,0.204885034163743,
0.227064931651241));
#29089=CARTESIAN_POINT('Ctrl Pts',(0.0282154732632697,0.203923906948376,
0.226378796488672));
#29090=CARTESIAN_POINT('Ctrl Pts',(0.0407766759930771,0.201786220869319,
0.225692661326102));
#29091=CARTESIAN_POINT('Ctrl Pts',(0.0530143360710842,0.198518149789741,
0.225006526163533));
#29092=CARTESIAN_POINT('Ctrl Pts',(0.0652803005675619,0.195242520006062,
0.22431880404262));
#29093=CARTESIAN_POINT('Ctrl Pts',(0.0772204080400473,0.190831566379232,
0.223631081921707));
#29094=CARTESIAN_POINT('Ctrl Pts',(0.0886219140799566,0.185381045335829,
0.222943359800793));
#29095=CARTESIAN_POINT('Ctrl Pts',(0.0931242601512917,0.183228686522827,
0.222671784889687));
#29096=CARTESIAN_POINT('Ctrl Pts',(0.0975428768938958,0.180914732552036,
0.222400209978581));
#29097=CARTESIAN_POINT('Ctrl Pts',(0.101865828789877,0.178446990868301,
0.222128635067475));
#29098=CARTESIAN_POINT('Ctrl Pts',(0.109968665011166,0.173821515688171,
0.221619601638593));
#29099=CARTESIAN_POINT('Ctrl Pts',(0.117776750206857,0.168631069100439,
0.221110568209711));
#29100=CARTESIAN_POINT('Ctrl Pts',(0.125207372047944,0.16292050088877,0.220601534780829));
#29101=CARTESIAN_POINT('Ctrl Pts',(0.125296449978256,0.163038483752231,
0.290616425505885));
#29102=CARTESIAN_POINT('Ctrl Pts',(0.134047410568505,0.156444912057247,
0.290021082642981));
#29103=CARTESIAN_POINT('Ctrl Pts',(0.193248710015229,0.103737668777768,
0.285720086343982));
#29104=CARTESIAN_POINT('Ctrl Pts',(0.235817802334529,-0.0581630255277868,
0.277713436608889));
#29105=CARTESIAN_POINT('Ctrl Pts',(0.078963123396891,-0.229690015875461,
0.266596476300606));
#29106=CARTESIAN_POINT('Ctrl Pts',(-0.143023970547039,-0.192086430267149,
0.255827853965015));
#29107=CARTESIAN_POINT('Ctrl Pts',(-0.205335749874147,-0.0615880815422457,
0.248764885065516));
#29108=CARTESIAN_POINT('Ctrl Pts',(-0.205737936806428,0.000108947515189247,
0.245407569602111));
#29109=CARTESIAN_POINT('Origin',(0.,0.,0.554592528053768));
#29110=CARTESIAN_POINT('',(0.125005569899291,0.162656434463559,0.360610754417505));
#29111=CARTESIAN_POINT('',(0.125373879670659,0.163134317426071,0.354786983357521));
#29112=CARTESIAN_POINT('',(0.125207372047944,0.16292050088877,0.554592528053768));
#29113=CARTESIAN_POINT('',(-0.205269929560708,-0.000254221530507089,0.385407471946233));
#29114=CARTESIAN_POINT('Ctrl Pts',(-0.205269929560708,-0.000254221530507089,
0.385407471946233));
#29115=CARTESIAN_POINT('Ctrl Pts',(-0.204911815068299,0.046813956992531,
0.382860341091967));
#29116=CARTESIAN_POINT('Ctrl Pts',(-0.165590599079174,0.163076528415273,
0.376607556801606));
#29117=CARTESIAN_POINT('Ctrl Pts',(-0.0053899581889141,0.227970089641994,
0.36834198429203));
#29118=CARTESIAN_POINT('Ctrl Pts',(0.0954129300657175,0.185281260987852,
0.36262354263672));
#29119=CARTESIAN_POINT('Ctrl Pts',(0.125005569899291,0.162656434463559,
0.360610754417505));
#29120=CARTESIAN_POINT('',(-0.053017021718863,-0.198517432567172,0.4));
#29121=CARTESIAN_POINT('Ctrl Pts',(-0.0530170217188623,-0.198517432567172,
0.4));
#29122=CARTESIAN_POINT('Ctrl Pts',(-0.11904762702766,-0.180882981070921,
0.396294346563906));
#29123=CARTESIAN_POINT('Ctrl Pts',(-0.192514897068364,-0.111293028538514,
0.391430170545983));
#29124=CARTESIAN_POINT('Ctrl Pts',(-0.205432812329624,-0.0216624454594562,
0.386565994528061));
#29125=CARTESIAN_POINT('Ctrl Pts',(-0.205269929560708,-0.000254221530507089,
0.385407471946233));
#29126=CARTESIAN_POINT('',(0.0530272806035336,-0.198514692496032,0.399999999884365));
#29127=CARTESIAN_POINT('Origin',(0.,0.,0.4));
#29128=CARTESIAN_POINT('',(-0.205474945991894,0.00014897861661356,0.379592528053768));
#29129=CARTESIAN_POINT('Ctrl Pts',(0.0530272806035336,-0.198514692496032,
0.399999999884365));
#29130=CARTESIAN_POINT('Ctrl Pts',(0.0408717438820405,-0.201761681666015,
0.39931360375684));
#29131=CARTESIAN_POINT('Ctrl Pts',(0.0283736580848827,-0.20389956149503,
0.398627207629315));
#29132=CARTESIAN_POINT('Ctrl Pts',(0.0157570658297097,-0.204869935572397,
0.39794081150179));
#29133=CARTESIAN_POINT('Ctrl Pts',(0.00316664435563644,-0.205838296788681,
0.397255839175751));
#29134=CARTESIAN_POINT('Ctrl Pts',(-0.00954094414690598,-0.205643818959396,
0.396570866849711));
#29135=CARTESIAN_POINT('Ctrl Pts',(-0.0221335092146457,-0.204279424795659,
0.395885894523672));
#29136=CARTESIAN_POINT('Ctrl Pts',(-0.0347240236104722,-0.202915252820552,
0.395201033743891));
#29137=CARTESIAN_POINT('Ctrl Pts',(-0.0471986847358641,-0.200381590770703,
0.394516172964109));
#29138=CARTESIAN_POINT('Ctrl Pts',(-0.0593287840410988,-0.196723336209014,
0.393831312184328));
#29139=CARTESIAN_POINT('Ctrl Pts',(-0.0714581310177007,-0.193065308538266,
0.393146493880734));
#29140=CARTESIAN_POINT('Ctrl Pts',(-0.083242134706469,-0.188283102977198,
0.392461675577141));
#29141=CARTESIAN_POINT('Ctrl Pts',(-0.0944682472819012,-0.18247116451781,
0.391776857273547));
#29142=CARTESIAN_POINT('Ctrl Pts',(-0.105719366886094,-0.176646279518715,
0.391090513484537));
#29143=CARTESIAN_POINT('Ctrl Pts',(-0.116409373895057,-0.169787539362461,
0.390404169695527));
#29144=CARTESIAN_POINT('Ctrl Pts',(-0.126352259228902,-0.162034200750188,
0.389717825906517));
#29145=CARTESIAN_POINT('Ctrl Pts',(-0.129366540326112,-0.159683701751704,
0.389509754200978));
#29146=CARTESIAN_POINT('Ctrl Pts',(-0.132312391393676,-0.15725126197307,
0.389301682495438));
#29147=CARTESIAN_POINT('Ctrl Pts',(-0.135185282742093,-0.154741445498419,
0.389093610789898));
#29148=CARTESIAN_POINT('Ctrl Pts',(-0.144554550829065,-0.146556261811243,
0.38841503323367));
#29149=CARTESIAN_POINT('Ctrl Pts',(-0.153213834910319,-0.137485213545017,
0.387736455677443));
#29150=CARTESIAN_POINT('Ctrl Pts',(-0.16099192577821,-0.127677623173457,
0.387057878121216));
#29151=CARTESIAN_POINT('Ctrl Pts',(-0.168758910581936,-0.117884036717488,
0.38638026948217));
#29152=CARTESIAN_POINT('Ctrl Pts',(-0.175646580121297,-0.107356630055652,
0.385702660843124));
#29153=CARTESIAN_POINT('Ctrl Pts',(-0.181521398102516,-0.0962806193161842,
0.385025052204078));
#29154=CARTESIAN_POINT('Ctrl Pts',(-0.187390823725915,-0.0852147749875414,
0.38434806552613));
#29155=CARTESIAN_POINT('Ctrl Pts',(-0.192248809751825,-0.0736021027695189,
0.383671078848182));
#29156=CARTESIAN_POINT('Ctrl Pts',(-0.196007247674439,-0.0616533412240657,
0.382994092170234));
#29157=CARTESIAN_POINT('Ctrl Pts',(-0.199772028850871,-0.0496844133145936,
0.382315962916988));
#29158=CARTESIAN_POINT('Ctrl Pts',(-0.202433306145674,-0.037379121243756,
0.381637833663743));
#29159=CARTESIAN_POINT('Ctrl Pts',(-0.203952980621335,-0.024963119209617,
0.380959704410497));
#29160=CARTESIAN_POINT('Ctrl Pts',(-0.204974252501832,-0.0166191521635482,
0.380503978958254));
#29161=CARTESIAN_POINT('Ctrl Pts',(-0.205481017838544,-0.00822546055280679,
0.380048253506011));
#29162=CARTESIAN_POINT('Ctrl Pts',(-0.205474945991894,0.00014897861661356,
0.379592528053768));
#29163=CARTESIAN_POINT('Ctrl Pts',(-0.205652323534904,0.000149107223343921,
0.379592528053768));
#29164=CARTESIAN_POINT('Ctrl Pts',(-0.20573550917628,0.010055539256624,
0.379053902196384));
#29165=CARTESIAN_POINT('Ctrl Pts',(-0.200581379579465,0.0880330322633288,
0.374809622902905));
#29166=CARTESIAN_POINT('Ctrl Pts',(-0.100785874709386,0.221009791285371,
0.366859690173332));
#29167=CARTESIAN_POINT('Ctrl Pts',(0.060421068680088,0.209514631200961,
0.359129801131968));
#29168=CARTESIAN_POINT('Ctrl Pts',(0.120756096920903,0.166732102669948,
0.355105565526697));
#29169=CARTESIAN_POINT('Ctrl Pts',(0.125373879670659,0.163134317426071,
0.354786983357521));
#29170=CARTESIAN_POINT('Origin',(0.,0.,0.2));
#29171=CARTESIAN_POINT('',(-0.156342830367367,0.0575541431412261,0.00322368732047967));
#29172=CARTESIAN_POINT('',(-0.156342830367367,0.0575541431412265,0.));
#29173=CARTESIAN_POINT('',(-0.156342830367367,0.0575541431412265,0.2));
#29174=CARTESIAN_POINT('',(-0.133525467299036,0.0997593943732614,4.94193308168658E-8));
#29175=CARTESIAN_POINT('Origin',(0.,0.,0.));
#29176=CARTESIAN_POINT('Ctrl Pts',(-0.133464457974224,0.0997135821122009,
4.94960437080749E-8));
#29177=CARTESIAN_POINT('Ctrl Pts',(-0.139892380533608,0.0911099477615352,
0.000722668837111375));
#29178=CARTESIAN_POINT('Ctrl Pts',(-0.145510047094401,0.0818485169225855,
0.00144528817817908));
#29179=CARTESIAN_POINT('Ctrl Pts',(-0.150187465421622,0.072106069302308,
0.00216790751924678));
#29180=CARTESIAN_POINT('Ctrl Pts',(-0.152465439227535,0.0673613492597746,
0.00251983411965774));
#29181=CARTESIAN_POINT('Ctrl Pts',(-0.154520997855119,0.0625030562146302,
0.00287176072006871));
#29182=CARTESIAN_POINT('Ctrl Pts',(-0.156342830367367,0.0575541431412261,
0.00322368732047967));
#29183=CARTESIAN_POINT('Origin',(0.,0.,0.2));
#29184=CARTESIAN_POINT('',(-0.156342830139253,0.0575541437608846,0.0733422317177101));
#29185=CARTESIAN_POINT('',(-0.156342830367367,0.0575541431412264,0.0539160112414913));
#29186=CARTESIAN_POINT('',(-0.156342830367367,0.0575541431412265,0.2));
#29187=CARTESIAN_POINT('',(-0.0769902040670466,-0.147743251885541,0.));
#29188=CARTESIAN_POINT('Ctrl Pts',(-0.156342830367367,0.0575541431412264,
0.0539160112414913));
#29189=CARTESIAN_POINT('Ctrl Pts',(-0.152615756398934,0.0676785453373198,
0.0531935750919307));
#29190=CARTESIAN_POINT('Ctrl Pts',(-0.147891507930115,0.0774656277419028,
0.05247113894237));
#29191=CARTESIAN_POINT('Ctrl Pts',(-0.142255363256947,0.0867120039246811,
0.0517487027928093));
#29192=CARTESIAN_POINT('Ctrl Pts',(-0.136621244092119,0.0959550571600989,
0.0510265262711557));
#29193=CARTESIAN_POINT('Ctrl Pts',(-0.130076306162921,0.104656981987856,
0.050304349749502));
#29194=CARTESIAN_POINT('Ctrl Pts',(-0.122751565884437,0.112639305186594,
0.0495821732278483));
#29195=CARTESIAN_POINT('Ctrl Pts',(-0.11542826033528,0.120620064852326,
0.048860138162109));
#29196=CARTESIAN_POINT('Ctrl Pts',(-0.107326090505026,0.127880844210078,
0.0481381030963697));
#29197=CARTESIAN_POINT('Ctrl Pts',(-0.0986138651527419,0.134279058678697,
0.0474160680306305));
#29198=CARTESIAN_POINT('Ctrl Pts',(-0.0898809033414771,0.140692501898468,
0.0466923144085044));
#29199=CARTESIAN_POINT('Ctrl Pts',(-0.0805357626312733,0.146238792804792,
0.0459685607863782));
#29200=CARTESIAN_POINT('Ctrl Pts',(-0.0707758351420504,0.150818901865599,
0.0452448071642521));
#29201=CARTESIAN_POINT('Ctrl Pts',(-0.0672833339567882,0.152457852189888,
0.0449858185205451));
#29202=CARTESIAN_POINT('Ctrl Pts',(-0.0637379152078948,0.153973529339594,
0.044726829876838));
#29203=CARTESIAN_POINT('Ctrl Pts',(-0.0601491615363001,0.155362924684366,
0.044467841233131));
#29204=CARTESIAN_POINT('Ctrl Pts',(-0.0500871093811335,0.159258474421843,
0.0437416957578361));
#29205=CARTESIAN_POINT('Ctrl Pts',(-0.0396085706270415,0.162186610709678,
0.0430155502825413));
#29206=CARTESIAN_POINT('Ctrl Pts',(-0.0289208966445087,0.164070538907135,
0.0422894048072465));
#29207=CARTESIAN_POINT('Ctrl Pts',(-0.0179575253928811,0.166003064569302,
0.0415445278170466));
#29208=CARTESIAN_POINT('Ctrl Pts',(-0.00677497403134137,0.166836279722674,
0.0407996508268468));
#29209=CARTESIAN_POINT('Ctrl Pts',(0.00438737489389764,0.16654221969681,
0.040054773836647));
#29210=CARTESIAN_POINT('Ctrl Pts',(0.015243375983249,0.166256230073792,
0.0393303398065695));
#29211=CARTESIAN_POINT('Ctrl Pts',(0.0260793197013875,0.164904216308862,
0.038605905776492));
#29212=CARTESIAN_POINT('Ctrl Pts',(0.0366743509548406,0.162513236328741,
0.0378814717464145));
#29213=CARTESIAN_POINT('Ctrl Pts',(0.0477178574160074,0.160021048979093,
0.0371263732761536));
#29214=CARTESIAN_POINT('Ctrl Pts',(0.0584985092249134,0.156399957609841,
0.0363712748058926));
#29215=CARTESIAN_POINT('Ctrl Pts',(0.0687813422296158,0.151738877553159,
0.0356161763356316));
#29216=CARTESIAN_POINT('Ctrl Pts',(0.0790641752343186,0.147077797496476,
0.0348610778653706));
#29217=CARTESIAN_POINT('Ctrl Pts',(0.0888482470888435,0.141377313875567,
0.0341059793951096));
#29218=CARTESIAN_POINT('Ctrl Pts',(0.0979290929616005,0.134779274191985,
0.0333508809248486));
#29219=CARTESIAN_POINT('Ctrl Pts',(0.106657202728024,0.128437528565149,
0.0326251134770529));
#29220=CARTESIAN_POINT('Ctrl Pts',(0.114797950788352,0.121221776032182,
0.0318993460292573));
#29221=CARTESIAN_POINT('Ctrl Pts',(0.122174628985777,0.113264822571652,
0.0311735785814616));
#29222=CARTESIAN_POINT('Ctrl Pts',(0.12974649655419,0.105097325462697,0.0304286070843869));
#29223=CARTESIAN_POINT('Ctrl Pts',(0.136512390637496,0.0961493361664923,
0.0296836355873123));
#29224=CARTESIAN_POINT('Ctrl Pts',(0.142319108061956,0.0866073408000109,
0.0289386640902376));
#29225=CARTESIAN_POINT('Ctrl Pts',(0.147963582781976,0.077331953746084,
0.0282145074841902));
#29226=CARTESIAN_POINT('Ctrl Pts',(0.152701412631395,0.0674962147486724,
0.0274903508781428));
#29227=CARTESIAN_POINT('Ctrl Pts',(0.156435984337242,0.0573004607698592,
0.0267661942720954));
#29228=CARTESIAN_POINT('Ctrl Pts',(0.160331573775527,0.0466651122898616,
0.0260108153295071));
#29229=CARTESIAN_POINT('Ctrl Pts',(0.163134817554856,0.0356389106652969,
0.0252554363869188));
#29230=CARTESIAN_POINT('Ctrl Pts',(0.164793439816337,0.0244679830288367,
0.0245000574443305));
#29231=CARTESIAN_POINT('Ctrl Pts',(0.166452062077817,0.0132970553923761,
0.0237446785017422));
#29232=CARTESIAN_POINT('Ctrl Pts',(0.166966048451613,0.0019825153896915,
0.0229892995591539));
#29233=CARTESIAN_POINT('Ctrl Pts',(0.166344308986419,-0.00922663903221849,
0.0222339206165656));
#29234=CARTESIAN_POINT('Ctrl Pts',(0.165754249536044,-0.0198646439645363,
0.0215170311336875));
#29235=CARTESIAN_POINT('Ctrl Pts',(0.164136945659952,-0.0304899505688286,
0.0208001416508095));
#29236=CARTESIAN_POINT('Ctrl Pts',(0.161504983847412,-0.0408864304194841,
0.0200832521679314));
#29237=CARTESIAN_POINT('Ctrl Pts',(0.158761774196747,-0.051722348981587,
0.0193360611796274));
#29238=CARTESIAN_POINT('Ctrl Pts',(0.154916029353243,-0.06230855393879,
0.0185888701913233));
#29239=CARTESIAN_POINT('Ctrl Pts',(0.150041776687632,-0.0724087373762231,
0.0178416792030193));
#29240=CARTESIAN_POINT('Ctrl Pts',(0.145375225859147,-0.0820785314187703,
0.017126327545091));
#29241=CARTESIAN_POINT('Ctrl Pts',(0.139766704504901,-0.0913020834547842,
0.0164109758871627));
#29242=CARTESIAN_POINT('Ctrl Pts',(0.133329944446156,-0.0998933727230443,
0.0156956242292345));
#29243=CARTESIAN_POINT('Ctrl Pts',(0.12689205686693,-0.108486166918397,
0.0149801472639098));
#29244=CARTESIAN_POINT('Ctrl Pts',(0.119626238227325,-0.116445760369784,
0.014264670298585));
#29245=CARTESIAN_POINT('Ctrl Pts',(0.111686655558303,-0.123618974960161,
0.0135491933332603));
#29246=CARTESIAN_POINT('Ctrl Pts',(0.103726328226589,-0.130810931835026,
0.012831846958808));
#29247=CARTESIAN_POINT('Ctrl Pts',(0.0950894792843525,-0.137211862084236,
0.0121145005843559));
#29248=CARTESIAN_POINT('Ctrl Pts',(0.0859617718008449,-0.142709963873794,
0.0113971542099036));
#29249=CARTESIAN_POINT('Ctrl Pts',(0.0847733510398566,-0.143425812658885,
0.0113037562426968));
#29250=CARTESIAN_POINT('Ctrl Pts',(0.0835766414215304,-0.14412642177342,
0.0112103582754899));
#29251=CARTESIAN_POINT('Ctrl Pts',(0.0823720791733835,-0.144811603722401,
0.011116960308283));
#29252=CARTESIAN_POINT('Ctrl Pts',(0.0727647703535419,-0.150276455864141,
0.0103720398066797));
#29253=CARTESIAN_POINT('Ctrl Pts',(0.0625826554862529,-0.154797868787369,
0.0096271193050763));
#29254=CARTESIAN_POINT('Ctrl Pts',(0.0520293316166242,-0.158267206494357,
0.00888219880347299));
#29255=CARTESIAN_POINT('Ctrl Pts',(0.0415003014352618,-0.161728557806747,
0.00813899310439756));
#29256=CARTESIAN_POINT('Ctrl Pts',(0.0306025347797131,-0.164142306937139,
0.0073957874053221));
#29257=CARTESIAN_POINT('Ctrl Pts',(0.019559542774564,-0.165447829500571,
0.00665258170624666));
#29258=CARTESIAN_POINT('Ctrl Pts',(0.00853395449654739,-0.166751294563785,
0.00591054729745052));
#29259=CARTESIAN_POINT('Ctrl Pts',(-0.00263556846420341,-0.166949863901546,
0.00516851288865437));
#29260=CARTESIAN_POINT('Ctrl Pts',(-0.0137173127653849,-0.166034319736904,
0.00442647847985822));
#29261=CARTESIAN_POINT('Ctrl Pts',(-0.0248064277508162,-0.165118166625984,
0.0036839505295057));
#29262=CARTESIAN_POINT('Ctrl Pts',(-0.0358067961519084,-0.163086461087822,
0.00294142257915325));
#29263=CARTESIAN_POINT('Ctrl Pts',(-0.0464896508237926,-0.159982100143366,
0.00219889462880074));
#29264=CARTESIAN_POINT('Ctrl Pts',(-0.0570349201958577,-0.1569177205002,
0.00146592975253386));
#29265=CARTESIAN_POINT('Ctrl Pts',(-0.0672700612540289,-0.152808496958899,
0.000732964876266929));
#29266=CARTESIAN_POINT('Ctrl Pts',(-0.0769902040670455,-0.147743251885542,
5.55111512312578E-17));
#29267=CARTESIAN_POINT('Origin',(0.,0.,0.));
#29268=CARTESIAN_POINT('',(-0.166599954470727,-0.000123167981316404,0.00714803633902117));
#29269=CARTESIAN_POINT('Ctrl Pts',(-0.156342830367367,0.0575541431412261,
0.00322368732047967));
#29270=CARTESIAN_POINT('Ctrl Pts',(-0.160075959044492,0.0474132936445152,
0.00394482237290883));
#29271=CARTESIAN_POINT('Ctrl Pts',(-0.16282449732221,0.0368910332598892,
0.004665957425338));
#29272=CARTESIAN_POINT('Ctrl Pts',(-0.164527021450747,0.0261996032898461,
0.00538709247776717));
#29273=CARTESIAN_POINT('Ctrl Pts',(-0.165912822627511,0.0174971150340725,
0.00597407376485183));
#29274=CARTESIAN_POINT('Ctrl Pts',(-0.166606465027433,0.00868316658102717,
0.00656105505193651));
#29275=CARTESIAN_POINT('Ctrl Pts',(-0.166599954470727,-0.000123167981316404,
0.00714803633902117));
#29276=CARTESIAN_POINT('Ctrl Pts',(-0.166599958397467,-0.000117736835231835,
0.00723493944780304));
#29277=CARTESIAN_POINT('Ctrl Pts',(-0.166592368206091,-0.0108580082624692,
0.00790617652409698));
#29278=CARTESIAN_POINT('Ctrl Pts',(-0.165546235023722,-0.0215724161967638,
0.00855403105481129));
#29279=CARTESIAN_POINT('Ctrl Pts',(-0.162441244087431,-0.0373794110721927,
0.00955409310228141));
#29280=CARTESIAN_POINT('Ctrl Pts',(-0.161152620668966,-0.0425934270508658,
0.00989185324071785));
#29281=CARTESIAN_POINT('Ctrl Pts',(-0.159055055717249,-0.0496071060965288,
0.0103680472660056));
#29282=CARTESIAN_POINT('Ctrl Pts',(-0.158462514085925,-0.0514685001513247,
0.0104965848910276));
#29283=CARTESIAN_POINT('Ctrl Pts',(-0.157350802925274,-0.0547594435620609,
0.0107284149417728));
#29284=CARTESIAN_POINT('Ctrl Pts',(-0.156844552891193,-0.0561930377736858,
0.0108310190040426));
#29285=CARTESIAN_POINT('Ctrl Pts',(-0.155543472955219,-0.0597228008901498,
0.0110876343866849));
#29286=CARTESIAN_POINT('Ctrl Pts',(-0.154725867189838,-0.0618101100221925,
0.0112428263475635));
#29287=CARTESIAN_POINT('Ctrl Pts',(-0.150165835048625,-0.0727937397929403,
0.0120755817193222));
#29288=CARTESIAN_POINT('Ctrl Pts',(-0.145697941630321,-0.0813682410202298,
0.0127813383790904));
#29289=CARTESIAN_POINT('Ctrl Pts',(-0.135157226586141,-0.0979156585876231,
0.0142067535748699));
#29290=CARTESIAN_POINT('Ctrl Pts',(-0.129056335196386,-0.105827549577747,
0.0149229165520539));
#29291=CARTESIAN_POINT('Ctrl Pts',(-0.120037218891217,-0.115574936681505,
0.0158413941168924));
#29292=CARTESIAN_POINT('Ctrl Pts',(-0.117718951883375,-0.117935367779911,
0.0160672245974781));
#29293=CARTESIAN_POINT('Ctrl Pts',(-0.113458916973888,-0.122022005173732,
0.0164648200388858));
#29294=CARTESIAN_POINT('Ctrl Pts',(-0.111544231225263,-0.123774720228262,
0.0166377011249371));
#29295=CARTESIAN_POINT('Ctrl Pts',(-0.10725320154447,-0.127522274301523,
0.0170131168076669));
#29296=CARTESIAN_POINT('Ctrl Pts',(-0.104860493546977,-0.129496944483681,
0.0172147810714845));
#29297=CARTESIAN_POINT('Ctrl Pts',(-0.0973081156948805,-0.135383142208357,
0.017829906463473));
#29298=CARTESIAN_POINT('Ctrl Pts',(-0.0919744243385157,-0.139061794399417,
0.0182345513585974));
#29299=CARTESIAN_POINT('Ctrl Pts',(-0.0779129673261363,-0.147596126968494,
0.0192487804156516));
#29300=CARTESIAN_POINT('Ctrl Pts',(-0.0689391260660634,-0.151994836564664,
0.0198481246745527));
#29301=CARTESIAN_POINT('Ctrl Pts',(-0.0551441590205115,-0.157282297394672,
0.0207662746777883));
#29302=CARTESIAN_POINT('Ctrl Pts',(-0.0505904342340529,-0.15880553729486,
0.0210691251433191));
#29303=CARTESIAN_POINT('Ctrl Pts',(-0.0441746294974275,-0.160647693709756,
0.0215035785467938));
#29304=CARTESIAN_POINT('Ctrl Pts',(-0.0423629661008501,-0.161134905313752,
0.0216271032871064));
#29305=CARTESIAN_POINT('Ctrl Pts',(-0.0391022697005884,-0.161953019748277,
0.0218515749498044));
#29306=CARTESIAN_POINT('Ctrl Pts',(-0.0376563782906403,-0.162295300820419,
0.0219519065039507));
#29307=CARTESIAN_POINT('Ctrl Pts',(-0.0344156680042966,-0.163016828708008,
0.0221784773177518));
#29308=CARTESIAN_POINT('Ctrl Pts',(-0.0326188426827027,-0.16338584711307,
0.0223052104047674));
#29309=CARTESIAN_POINT('Ctrl Pts',(-0.0245482288464476,-0.164904900506212,
0.0228783100832908));
#29310=CARTESIAN_POINT('Ctrl Pts',(-0.0182180557007977,-0.165723651928309,
0.02333803504725));
#29311=CARTESIAN_POINT('Ctrl Pts',(-0.00266982004660984,-0.166833060022998,
0.024470488153681));
#29312=CARTESIAN_POINT('Ctrl Pts',(0.00655685279637343,-0.166725607649479,
0.0251444914691373));
#29313=CARTESIAN_POINT('Ctrl Pts',(0.0214036166788052,-0.165317727473419,
0.02620817517656));
#29314=CARTESIAN_POINT('Ctrl Pts',(0.027048668748578,-0.164488443891499,
0.0266079380167437));
#29315=CARTESIAN_POINT('Ctrl Pts',(0.0354882404179006,-0.162802264009165,
0.0271978686362366));
#29316=CARTESIAN_POINT('Ctrl Pts',(0.0383206014720584,-0.162158952090207,
0.027394550835668));
#29317=CARTESIAN_POINT('Ctrl Pts',(0.0436379708253891,-0.160804103888315,
0.0277616805416717));
#29318=CARTESIAN_POINT('Ctrl Pts',(0.0461260205228799,-0.160108162928327,
0.0279325756683645));
#29319=CARTESIAN_POINT('Ctrl Pts',(0.0519592080958445,-0.158329265883714,
0.0283316986612704));
#29320=CARTESIAN_POINT('Ctrl Pts',(0.0552882965295458,-0.157197719114055,
0.0285582573366589));
#29321=CARTESIAN_POINT('Ctrl Pts',(0.0682544247256167,-0.152327631974431,
0.0294393615905225));
#29322=CARTESIAN_POINT('Ctrl Pts',(0.0775706675717061,-0.147801187405166,
0.0300679352278671));
#29323=CARTESIAN_POINT('Ctrl Pts',(0.0917563256834444,-0.13919578656551,
0.0310798904630806));
#29324=CARTESIAN_POINT('Ctrl Pts',(0.0969173310599853,-0.135652910945856,
0.0314617418059934));
#29325=CARTESIAN_POINT('Ctrl Pts',(0.104003512100219,-0.130177273155847,
0.0320234510840598));
#29326=CARTESIAN_POINT('Ctrl Pts',(0.106099843565373,-0.128474412091306,
0.0321947291697927));
#29327=CARTESIAN_POINT('Ctrl Pts',(0.109817288218199,-0.125301661601329,
0.03250977571567));
#29328=CARTESIAN_POINT('Ctrl Pts',(0.111452611561631,-0.123849333474221,
0.0326525543144872));
#29329=CARTESIAN_POINT('Ctrl Pts',(0.114148068623023,-0.121358880726997,
0.0328959944787813));
#29330=CARTESIAN_POINT('Ctrl Pts',(0.115223743450111,-0.120338057850148,
0.0329954332102852));
#29331=CARTESIAN_POINT('Ctrl Pts',(0.117628426211631,-0.117994190888653,
0.0332231479315271));
#29332=CARTESIAN_POINT('Ctrl Pts',(0.118948878478074,-0.116662930084048,
0.0333519923055864));
#29333=CARTESIAN_POINT('Ctrl Pts',(0.123212799975926,-0.112216457135386,
0.0337798979674513));
#29334=CARTESIAN_POINT('Ctrl Pts',(0.126058385322084,-0.109010112184116,
0.0340846098461402));
#29335=CARTESIAN_POINT('Ctrl Pts',(0.135780660084974,-0.0971649913331188,
0.0351869742860296));
#29336=CARTESIAN_POINT('Ctrl Pts',(0.141919086720901,-0.087956919649469,
0.0359998247712268));
#29337=CARTESIAN_POINT('Ctrl Pts',(0.150003673060108,-0.0727507328644793,
0.0372322330029602));
#29338=CARTESIAN_POINT('Ctrl Pts',(0.152599775061937,-0.0671349060529186,
0.0376670365958292));
#29339=CARTESIAN_POINT('Ctrl Pts',(0.155977327425111,-0.0586134399364334,
0.0382963863519817));
#29340=CARTESIAN_POINT('Ctrl Pts',(0.157002052364009,-0.0558105686102229,
0.0384987729075076));
#29341=CARTESIAN_POINT('Ctrl Pts',(0.158777867577763,-0.0505164247947176,
0.0388728636293751));
#29342=CARTESIAN_POINT('Ctrl Pts',(0.159546950652165,-0.0480322000286018,
0.0390451156607787));
#29343=CARTESIAN_POINT('Ctrl Pts',(0.161187407552089,-0.042258189614945,
0.0394385112086754));
#29344=CARTESIAN_POINT('Ctrl Pts',(0.162016790525698,-0.0389576326242932,
0.0396582455843352));
#29345=CARTESIAN_POINT('Ctrl Pts',(0.164360440706438,-0.0282538518820897,
0.0403570546296552));
#29346=CARTESIAN_POINT('Ctrl Pts',(0.165472557282312,-0.0207721785598963,
0.0408241048564408));
#29347=CARTESIAN_POINT('Ctrl Pts',(0.166729528251484,-0.00500592924388155,
0.0417931774538173));
#29348=CARTESIAN_POINT('Ctrl Pts',(0.166772658709673,0.00326539906077528,
0.0422930461371366));
#29349=CARTESIAN_POINT('Ctrl Pts',(0.16589872011113,0.0158899850704833,
0.0430826823877555));
#29350=CARTESIAN_POINT('Ctrl Pts',(0.165421832421319,0.020260489237606,
0.0433611254795038));
#29351=CARTESIAN_POINT('Ctrl Pts',(0.164502508173179,0.0264165420258095,
0.0437669086990131));
#29352=CARTESIAN_POINT('Ctrl Pts',(0.16420243155374,0.0282217935483682,
0.0438875793531755));
#29353=CARTESIAN_POINT('Ctrl Pts',(0.163601369373112,0.0315026833445796,
0.0441105555291625));
#29354=CARTESIAN_POINT('Ctrl Pts',(0.163310006948505,0.0329798126116908,
0.0442123581354838));
#29355=CARTESIAN_POINT('Ctrl Pts',(0.162520207385939,0.0367164188842215,
0.044473306171508));
#29356=CARTESIAN_POINT('Ctrl Pts',(0.161994660715965,0.0389697544497462,
0.044633816515132));
#29357=CARTESIAN_POINT('Ctrl Pts',(0.159542247628278,0.0485757295139883,
0.0453295725218254));
#29358=CARTESIAN_POINT('Ctrl Pts',(0.157160471842514,0.055802309349271,
0.0458816939421));
#29359=CARTESIAN_POINT('Ctrl Pts',(0.15128179773945,0.070236397576997,0.0470160618690842));
#29360=CARTESIAN_POINT('Ctrl Pts',(0.147741471496556,0.0774067841388483,
0.0475968391062373));
#29361=CARTESIAN_POINT('Ctrl Pts',(0.141010981183482,0.0888803208855026,
0.048542005694306));
#29362=CARTESIAN_POINT('Ctrl Pts',(0.138103698186968,0.0933337413707272,
0.04891343187207));
#29363=CARTESIAN_POINT('Ctrl Pts',(0.133309512225687,0.0999616803598096,
0.0494731580193658));
#29364=CARTESIAN_POINT('Ctrl Pts',(0.131571215043564,0.102238841634508,
0.0496668486853999));
#29365=CARTESIAN_POINT('Ctrl Pts',(0.128130948366677,0.106512410466517,
0.0500334252771629));
#29366=CARTESIAN_POINT('Ctrl Pts',(0.126438878506964,0.108515643282706,
0.0502066325359914));
#29367=CARTESIAN_POINT('Ctrl Pts',(0.122638968076052,0.112804719032673,
0.050581118478324));
#29368=CARTESIAN_POINT('Ctrl Pts',(0.12051298923741,0.115073205116196,0.0507815652600641));
#29369=CARTESIAN_POINT('Ctrl Pts',(0.109219872710163,0.126466817527054,
0.0518041790836088));
#29370=CARTESIAN_POINT('Ctrl Pts',(0.099076625939989,0.134561062337971,
0.0525811797134423));
#29371=CARTESIAN_POINT('Ctrl Pts',(0.0822802446722472,0.145025918412974,
0.0537957833936754));
#29372=CARTESIAN_POINT('Ctrl Pts',(0.0762442217714142,0.148288076622371,
0.0542210374384404));
#29373=CARTESIAN_POINT('Ctrl Pts',(0.0681818604012453,0.152022764751916,
0.0547965324269851));
#29374=CARTESIAN_POINT('Ctrl Pts',(0.0663231457275668,0.15284281623537,
0.0549297129416109));
#29375=CARTESIAN_POINT('Ctrl Pts',(0.0632178415163958,0.154145547979268,
0.055153797117645));
#29376=CARTESIAN_POINT('Ctrl Pts',(0.0619796373186184,0.15464756626802,
0.0552435823339178));
#29377=CARTESIAN_POINT('Ctrl Pts',(0.0589549166825762,0.155831749423144,
0.055464056201819));
#29378=CARTESIAN_POINT('Ctrl Pts',(0.0571625872232252,0.156498096218549,
0.0555955943497492));
#29379=CARTESIAN_POINT('Ctrl Pts',(0.0508956524107808,0.158705984870631,
0.0560576521350662));
#29380=CARTESIAN_POINT('Ctrl Pts',(0.0463674110114099,0.160087514516793,
0.0563952002162176));
#29381=CARTESIAN_POINT('Ctrl Pts',(0.0315119747698736,0.163936629537465,
0.057502197453484));
#29382=CARTESIAN_POINT('Ctrl Pts',(0.0210051869178905,0.165611078142225,
0.0582827516981497));
#29383=CARTESIAN_POINT('Ctrl Pts',(0.00434482380566355,0.166654190916582,
0.0594765282641642));
#29384=CARTESIAN_POINT('Ctrl Pts',(-0.00173765817253539,0.166701807412088,
0.0599037483930031));
#29385=CARTESIAN_POINT('Ctrl Pts',(-0.0107704108373828,0.166277908332304,
0.0605243993235179));
#29386=CARTESIAN_POINT('Ctrl Pts',(-0.0137269451190884,0.166059981624386,
0.0607253865402798));
#29387=CARTESIAN_POINT('Ctrl Pts',(-0.0192548989393031,0.165503853496326,
0.0610974911352458));
#29388=CARTESIAN_POINT('Ctrl Pts',(-0.0218272444225489,0.165184289034333,
0.0612691384770206));
#29389=CARTESIAN_POINT('Ctrl Pts',(-0.0278163545184306,0.164297897039467,
0.0616658175862565));
#29390=CARTESIAN_POINT('Ctrl Pts',(-0.0312250363416327,0.163684294949153,
0.0618893045697229));
#29391=CARTESIAN_POINT('Ctrl Pts',(-0.0424408363650814,0.161302156188398,
0.0626199091541332));
#29392=CARTESIAN_POINT('Ctrl Pts',(-0.0501397394947855,0.159077448715882,
0.0631131610859068));
#29393=CARTESIAN_POINT('Ctrl Pts',(-0.0651021964221637,0.153558985352872,
0.064088440714332));
#29394=CARTESIAN_POINT('Ctrl Pts',(-0.0723483781403307,0.150280930274018,
0.0645693842021876));
#29395=CARTESIAN_POINT('Ctrl Pts',(-0.0831251800423115,0.144445024272915,
0.0653342910209706));
#29396=CARTESIAN_POINT('Ctrl Pts',(-0.0868361443326735,0.14224499293338,
0.0656076354806959));
#29397=CARTESIAN_POINT('Ctrl Pts',(-0.0919812432414162,0.138918337239207,
0.0660071111989614));
#29398=CARTESIAN_POINT('Ctrl Pts',(-0.093488958250325,0.137908185032123,
0.0661267942824281));
#29399=CARTESIAN_POINT('Ctrl Pts',(-0.0962138620331477,0.136017311492476,
0.066348533201565));
#29400=CARTESIAN_POINT('Ctrl Pts',(-0.097436157328333,0.135144407202752,
0.0664501044180121));
#29401=CARTESIAN_POINT('Ctrl Pts',(-0.10051080020847,0.132885256902538,
0.0667108162502505));
#29402=CARTESIAN_POINT('Ctrl Pts',(-0.102346319394633,0.131476773628673,
0.0668713303880289));
#29403=CARTESIAN_POINT('Ctrl Pts',(-0.110011714962414,0.125336952892199,
0.0675606381958586));
#29404=CARTESIAN_POINT('Ctrl Pts',(-0.115547179363288,0.120252901228537,
0.0681058875832981));
#29405=CARTESIAN_POINT('Ctrl Pts',(-0.126270803986498,0.108977555315009,
0.0692385558110044));
#29406=CARTESIAN_POINT('Ctrl Pts',(-0.13139106418083,0.102746439399671,
0.0698245284256865));
#29407=CARTESIAN_POINT('Ctrl Pts',(-0.139123253083575,0.0918084760142583,
0.0707765744402518));
#29408=CARTESIAN_POINT('Ctrl Pts',(-0.141994577432469,0.0873019267885008,
0.0711498417046757));
#29409=CARTESIAN_POINT('Ctrl Pts',(-0.146067692229229,0.0801748940696286,
0.0717116070706711));
#29410=CARTESIAN_POINT('Ctrl Pts',(-0.147426208465994,0.0776485620823815,
0.0719055645261873));
#29411=CARTESIAN_POINT('Ctrl Pts',(-0.149899905865631,0.0727491877081231,
0.0722723242475758));
#29412=CARTESIAN_POINT('Ctrl Pts',(-0.151025615460698,0.0703824614936514,
0.0724454558319081));
#29413=CARTESIAN_POINT('Ctrl Pts',(-0.153360678588948,0.0651588789322013,
0.0728194286729711));
#29414=CARTESIAN_POINT('Ctrl Pts',(-0.154547038060658,0.0622927944332981,
0.0730194484095675));
#29415=CARTESIAN_POINT('Ctrl Pts',(-0.155886421924921,0.0587827612910115,
0.0732589751331156));
#29416=CARTESIAN_POINT('Ctrl Pts',(-0.156116449063536,0.0581690961475399,
0.0733006546124061));
#29417=CARTESIAN_POINT('Ctrl Pts',(-0.156342830139253,0.0575541437608846,
0.0733422317177101));
#29418=CARTESIAN_POINT('Origin',(0.,0.,0.2));
#29419=CARTESIAN_POINT('',(-0.156342827686702,0.0575541504231124,0.143092354725971));
#29420=CARTESIAN_POINT('',(-0.156342837828316,0.0575541228739426,0.124011319110561));
#29421=CARTESIAN_POINT('',(-0.156342830367367,0.0575541431412265,0.2));
#29422=CARTESIAN_POINT('',(-0.16659993550101,0.000146598291904576,0.0578519636609792));
#29423=CARTESIAN_POINT('Ctrl Pts',(-0.156342837828316,0.0575541228739415,
0.124011319110561));
#29424=CARTESIAN_POINT('Ctrl Pts',(-0.154725453069797,0.0619476660361069,
0.123722051905057));
#29425=CARTESIAN_POINT('Ctrl Pts',(-0.152922562753768,0.0662738589531047,
0.123429120845098));
#29426=CARTESIAN_POINT('Ctrl Pts',(-0.149942023782046,0.0726532095146394,
0.122976715419712));
#29427=CARTESIAN_POINT('Ctrl Pts',(-0.148900753953121,0.0747640516607849,
0.122823516026912));
#29428=CARTESIAN_POINT('Ctrl Pts',(-0.147120475791605,0.0781881938864711,
0.12256803993962));
#29429=CARTESIAN_POINT('Ctrl Pts',(-0.146407752373643,0.07951476552139,
0.122467290584307));
#29430=CARTESIAN_POINT('Ctrl Pts',(-0.144807331138743,0.0823990922031432,
0.12224403303186));
#29431=CARTESIAN_POINT('Ctrl Pts',(-0.143912376649387,0.083952371568136,
0.122121131200895));
#29432=CARTESIAN_POINT('Ctrl Pts',(-0.140865319360235,0.0890489022939992,
0.121709695815543));
#29433=CARTESIAN_POINT('Ctrl Pts',(-0.138606166721996,0.0925260493602986,
0.121415688135929));
#29434=CARTESIAN_POINT('Ctrl Pts',(-0.131987601239479,0.101925833718144,
0.12059029845356));
#29435=CARTESIAN_POINT('Ctrl Pts',(-0.127362172181142,0.107649781884699,
0.120052423258189));
#29436=CARTESIAN_POINT('Ctrl Pts',(-0.116462988824626,0.119447950595325,
0.118885914487657));
#29437=CARTESIAN_POINT('Ctrl Pts',(-0.11005860773267,0.125373765505653,
0.11826102472132));
#29438=CARTESIAN_POINT('Ctrl Pts',(-0.100468907855806,0.132942979895767,
0.117412556444811));
#29439=CARTESIAN_POINT('Ctrl Pts',(-0.0976505636797978,0.135026693569089,
0.117172469667474));
#29440=CARTESIAN_POINT('Ctrl Pts',(-0.0926342284172894,0.138496184859958,
0.116760554500891));
#29441=CARTESIAN_POINT('Ctrl Pts',(-0.0904657639718171,0.139922265405343,
0.116587232103598));
#29442=CARTESIAN_POINT('Ctrl Pts',(-0.0857711637345476,0.142854862961744,
0.116221519981974));
#29443=CARTESIAN_POINT('Ctrl Pts',(-0.0832366528606942,0.144346339767803,
0.116029727666112));
#29444=CARTESIAN_POINT('Ctrl Pts',(-0.0755056016015739,0.148624423514541,
0.115460033985964));
#29445=CARTESIAN_POINT('Ctrl Pts',(-0.0701991573316435,0.151203187919349,
0.115089370955084));
#29446=CARTESIAN_POINT('Ctrl Pts',(-0.0556577900395314,0.157338853934701,
0.114111547890421));
#29447=CARTESIAN_POINT('Ctrl Pts',(-0.0462251194274684,0.160363766118285,
0.113516912455412));
#29448=CARTESIAN_POINT('Ctrl Pts',(-0.0311216899010314,0.163762948705462,
0.112560746042685));
#29449=CARTESIAN_POINT('Ctrl Pts',(-0.0256054261249472,0.164715550481705,
0.112210379323951));
#29450=CARTESIAN_POINT('Ctrl Pts',(-0.018123180340744,0.165622723613347,
0.111721282727405));
#29451=CARTESIAN_POINT('Ctrl Pts',(-0.0161902152254486,0.16582283415089,
0.11159368952016));
#29452=CARTESIAN_POINT('Ctrl Pts',(-0.0127795267112629,0.166115726831495,
0.111365671898325));
#29453=CARTESIAN_POINT('Ctrl Pts',(-0.01130331371372,0.166222698840556,
0.111265992609563));
#29454=CARTESIAN_POINT('Ctrl Pts',(-0.00776304744822872,0.166431863274377,
0.111024563412211));
#29455=CARTESIAN_POINT('Ctrl Pts',(-0.00569827357786861,0.16651534067669,
0.110881892695468));
#29456=CARTESIAN_POINT('Ctrl Pts',(0.00423235326266446,0.16673192324821,
0.110188420029989));
#29457=CARTESIAN_POINT('Ctrl Pts',(0.0120988786260143,0.166346149194,0.109617582559482));
#29458=CARTESIAN_POINT('Ctrl Pts',(0.0318398590412613,0.163970172156667,
0.108170343222935));
#29459=CARTESIAN_POINT('Ctrl Pts',(0.0435834322893147,0.161246922250911,
0.107298267785005));
#29460=CARTESIAN_POINT('Ctrl Pts',(0.0580754321810927,0.156185414531604,
0.10623496321242));
#29461=CARTESIAN_POINT('Ctrl Pts',(0.0611844572555237,0.154993885334271,
0.106007371138603));
#29462=CARTESIAN_POINT('Ctrl Pts',(0.0666406373702529,0.152713019271826,
0.105608558145339));
#29463=CARTESIAN_POINT('Ctrl Pts',(0.0690019636772164,0.151660710490881,
0.105436159952716));
#29464=CARTESIAN_POINT('Ctrl Pts',(0.0740554998370496,0.149266158336814,
0.105067194513687));
#29465=CARTESIAN_POINT('Ctrl Pts',(0.0767378024219951,0.147905086639286,
0.104871352485375));
#29466=CARTESIAN_POINT('Ctrl Pts',(0.0850494095566094,0.143400531892607,
0.104262918887946));
#29467=CARTESIAN_POINT('Ctrl Pts',(0.090534187284117,0.140002459102811,
0.103859306912318));
#29468=CARTESIAN_POINT('Ctrl Pts',(0.105965446622745,0.129155020432404,
0.102694982052404));
#29469=CARTESIAN_POINT('Ctrl Pts',(0.115291283275941,0.120903114810049,
0.101955332677491));
#29470=CARTESIAN_POINT('Ctrl Pts',(0.125746101264497,0.109332513463304,
0.10096833221906));
#29471=CARTESIAN_POINT('Ctrl Pts',(0.127810701941582,0.106911654663264,
0.100764003702223));
#29472=CARTESIAN_POINT('Ctrl Pts',(0.130836062803379,0.103151307872684,
0.100447212848912));
#29473=CARTESIAN_POINT('Ctrl Pts',(0.131848437439142,0.10185409482531,0.100338030597141));
#29474=CARTESIAN_POINT('Ctrl Pts',(0.133794582534161,0.099282749825201,
0.100121330854277));
#29475=CARTESIAN_POINT('Ctrl Pts',(0.134729761177099,0.0980099255780957,
0.100013916830774));
#29476=CARTESIAN_POINT('Ctrl Pts',(0.137275900406215,0.0944391992219327,
0.0997126070083064));
#29477=CARTESIAN_POINT('Ctrl Pts',(0.138847054607245,0.0921136709067474,
0.0995164068019336));
#29478=CARTESIAN_POINT('Ctrl Pts',(0.142435093693316,0.0865023772640151,
0.0990450609108452));
#29479=CARTESIAN_POINT('Ctrl Pts',(0.144398131673898,0.0831840934769976,
0.0987679606953816));
#29480=CARTESIAN_POINT('Ctrl Pts',(0.153425932652054,0.0666396281994464,
0.0974035161330653));
#29481=CARTESIAN_POINT('Ctrl Pts',(0.158799789250376,0.0525657110113161,
0.0963033912044357));
#29482=CARTESIAN_POINT('Ctrl Pts',(0.162949719096844,0.034832132070562,
0.0950457811875245));
#29483=CARTESIAN_POINT('Ctrl Pts',(0.163591350470555,0.0316821862647794,
0.0948266727454539));
#29484=CARTESIAN_POINT('Ctrl Pts',(0.164582577603962,0.0259764547574814,
0.0944370841661147));
#29485=CARTESIAN_POINT('Ctrl Pts',(0.164964713628559,0.0234274536875381,
0.0942656232792111));
#29486=CARTESIAN_POINT('Ctrl Pts',(0.165681181264564,0.0177532588292906,
0.0938891790859353));
#29487=CARTESIAN_POINT('Ctrl Pts',(0.165986543889806,0.0146253683559193,
0.0936851661898293));
#29488=CARTESIAN_POINT('Ctrl Pts',(0.166747334164281,0.00362102136062357,
0.0929775905649838));
#29489=CARTESIAN_POINT('Ctrl Pts',(0.166731841480788,-0.00427764075400164,
0.0924884779303847));
#29490=CARTESIAN_POINT('Ctrl Pts',(0.165322441031495,-0.0235578378170679,
0.0913033146014094));
#29491=CARTESIAN_POINT('Ctrl Pts',(0.163314946520931,-0.0348518931422863,
0.0906172204000628));
#29492=CARTESIAN_POINT('Ctrl Pts',(0.159436228682321,-0.0484013730270312,
0.089717251263363));
#29493=CARTESIAN_POINT('Ctrl Pts',(0.158644994611962,-0.0509349359524964,
0.0895454300186187));
#29494=CARTESIAN_POINT('Ctrl Pts',(0.157295639567099,-0.0549185888629535,
0.0892680193261755));
#29495=CARTESIAN_POINT('Ctrl Pts',(0.156777124854499,-0.0563817569866432,
0.0891645470378549));
#29496=CARTESIAN_POINT('Ctrl Pts',(0.155654717293024,-0.0594137548381485,
0.0889464217676151));
#29497=CARTESIAN_POINT('Ctrl Pts',(0.155047393287019,-0.0609810668870776,
0.0888316053855021));
#29498=CARTESIAN_POINT('Ctrl Pts',(0.15314061379648,-0.065689152528482,
0.0884810099145395));
#29499=CARTESIAN_POINT('Ctrl Pts',(0.15176872246785,-0.0687994446702336,
0.088241652952466));
#29500=CARTESIAN_POINT('Ctrl Pts',(0.148064879562693,-0.0765458475822932,
0.0876293882844434));
#29501=CARTESIAN_POINT('Ctrl Pts',(0.145609657750549,-0.0811190339744501,
0.0872529061625451));
#29502=CARTESIAN_POINT('Ctrl Pts',(0.136553237937524,-0.0962478443415829,
0.0859697178505096));
#29503=CARTESIAN_POINT('Ctrl Pts',(0.128983760603936,-0.106177802244518,
0.0850656205665919));
#29504=CARTESIAN_POINT('Ctrl Pts',(0.118112647291995,-0.117540193372558,
0.0839774413062043));
#29505=CARTESIAN_POINT('Ctrl Pts',(0.115778188720078,-0.119840344493579,
0.0837536172618009));
#29506=CARTESIAN_POINT('Ctrl Pts',(0.111487991152771,-0.123825022607398,
0.0833590242619421));
#29507=CARTESIAN_POINT('Ctrl Pts',(0.109558157093893,-0.125535731540204,
0.0831871630467895));
#29508=CARTESIAN_POINT('Ctrl Pts',(0.105270337051431,-0.129162459165449,
0.0828168761828334));
#29509=CARTESIAN_POINT('Ctrl Pts',(0.102898067324608,-0.131060193831256,
0.082619236805612));
#29510=CARTESIAN_POINT('Ctrl Pts',(0.0950999059168477,-0.136956112569433,
0.0819906157271924));
#29511=CARTESIAN_POINT('Ctrl Pts',(0.0894827650630372,-0.140690504316021,
0.0815696259483865));
#29512=CARTESIAN_POINT('Ctrl Pts',(0.0763374955651345,-0.148323065231777,
0.0806330391153741));
#29513=CARTESIAN_POINT('Ctrl Pts',(0.0687078403585891,-0.152007807266612,
0.0801223234772568));
#29514=CARTESIAN_POINT('Ctrl Pts',(0.0554300225198149,-0.157215572582331,
0.0792426026030043));
#29515=CARTESIAN_POINT('Ctrl Pts',(0.0499221337018299,-0.159050276688578,
0.0788798991546911));
#29516=CARTESIAN_POINT('Ctrl Pts',(0.042442022341175,-0.161115090709825,
0.0783765994065113));
#29517=CARTESIAN_POINT('Ctrl Pts',(0.0405446977138068,-0.161602983684703,
0.078248029831134));
#29518=CARTESIAN_POINT('Ctrl Pts',(0.0372006286201932,-0.162400310139741,
0.0780191212582774));
#29519=CARTESIAN_POINT('Ctrl Pts',(0.0357576137834182,-0.162724122638414,
0.0779195589888421));
#29520=CARTESIAN_POINT('Ctrl Pts',(0.0323087220935698,-0.163449964455691,
0.0776797076049208));
#29521=CARTESIAN_POINT('Ctrl Pts',(0.0302995175186563,-0.16383431463467,
0.0775385346668134));
#29522=CARTESIAN_POINT('Ctrl Pts',(0.0211806703824121,-0.165405235804386,
0.0768928206973488));
#29523=CARTESIAN_POINT('Ctrl Pts',(0.0140061956319152,-0.166166541799788,
0.0763714424499903));
#29524=CARTESIAN_POINT('Ctrl Pts',(-0.00628354264827478,-0.166996086718071,
0.0748943540378242));
#29525=CARTESIAN_POINT('Ctrl Pts',(-0.0193928594358192,-0.165985577880484,
0.073941091492511));
#29526=CARTESIAN_POINT('Ctrl Pts',(-0.0354215676844072,-0.162822985381798,
0.0728124145833674));
#29527=CARTESIAN_POINT('Ctrl Pts',(-0.0385746652365065,-0.162104934439796,
0.0725919070534207));
#29528=CARTESIAN_POINT('Ctrl Pts',(-0.0442005701508189,-0.160650283112852,
0.0722008581169207));
#29529=CARTESIAN_POINT('Ctrl Pts',(-0.0466808725415322,-0.159947182789996,
0.0720293023114863));
#29530=CARTESIAN_POINT('Ctrl Pts',(-0.0521298598916357,-0.15826497675637,
0.0716538172858228));
#29531=CARTESIAN_POINT('Ctrl Pts',(-0.0550893554399453,-0.157259308702417,
0.0714508273699702));
#29532=CARTESIAN_POINT('Ctrl Pts',(-0.065206559548865,-0.153500671661056,
0.070758183119521));
#29533=CARTESIAN_POINT('Ctrl Pts',(-0.072201645883046,-0.150337263384917,
0.0702820435634966));
#29534=CARTESIAN_POINT('Ctrl Pts',(-0.08651008007617,-0.14263655597519,
0.0692849242386713));
#29535=CARTESIAN_POINT('Ctrl Pts',(-0.0937398511852317,-0.137992791231213,
0.0687668848107746));
#29536=CARTESIAN_POINT('Ctrl Pts',(-0.104304676945384,-0.129992036812475,
0.067942971452615));
#29537=CARTESIAN_POINT('Ctrl Pts',(-0.10790917241171,-0.127015738556284,
0.0676481263927458));
#29538=CARTESIAN_POINT('Ctrl Pts',(-0.112798051628228,-0.122620462677744,
0.0672206736105204));
#29539=CARTESIAN_POINT('Ctrl Pts',(-0.114190652083881,-0.121324657383668,
0.0670955428489492));
#29540=CARTESIAN_POINT('Ctrl Pts',(-0.116635044305425,-0.118970799032179,
0.0668691317276555));
#29541=CARTESIAN_POINT('Ctrl Pts',(-0.117695333627289,-0.117921975903445,
0.0667685040492619));
#29542=CARTESIAN_POINT('Ctrl Pts',(-0.12027268540814,-0.115303109619265,
0.0665179532752511));
#29543=CARTESIAN_POINT('Ctrl Pts',(-0.121773167546282,-0.113717282952366,
0.0663669053068981));
#29544=CARTESIAN_POINT('Ctrl Pts',(-0.125050274746943,-0.110114535429565,
0.0660261141656472));
#29545=CARTESIAN_POINT('Ctrl Pts',(-0.126810122722278,-0.108083177820856,
0.0658355453019171));
#29546=CARTESIAN_POINT('Ctrl Pts',(-0.132451779600306,-0.101243598795633,
0.0652012989581215));
#29547=CARTESIAN_POINT('Ctrl Pts',(-0.13611520834504,-0.0962620625635409,
0.0647511564415182));
#29548=CARTESIAN_POINT('Ctrl Pts',(-0.145131157189463,-0.0824550401687818,
0.0635516510615432));
#29549=CARTESIAN_POINT('Ctrl Pts',(-0.149956011002495,-0.0733153436261364,
0.0628074513511484));
#29550=CARTESIAN_POINT('Ctrl Pts',(-0.155250743850838,-0.0605402244058745,
0.0618471089470116));
#29551=CARTESIAN_POINT('Ctrl Pts',(-0.156493391212513,-0.0572514975734302,
0.0616063024412582));
#29552=CARTESIAN_POINT('Ctrl Pts',(-0.158473444105204,-0.0514635698880582,
0.0611931911762856));
#29553=CARTESIAN_POINT('Ctrl Pts',(-0.159257974906303,-0.0489819381026251,
0.061019387551213));
#29554=CARTESIAN_POINT('Ctrl Pts',(-0.16080711851628,-0.0436501116847052,
0.0606525674310059));
#29555=CARTESIAN_POINT('Ctrl Pts',(-0.161554811480781,-0.0407959103372634,
0.0604601530192477));
#29556=CARTESIAN_POINT('Ctrl Pts',(-0.163075217572048,-0.0342919783698597,
0.060029533881489));
#29557=CARTESIAN_POINT('Ctrl Pts',(-0.163801961467106,-0.0306330998243484,
0.0597927924426006));
#29558=CARTESIAN_POINT('Ctrl Pts',(-0.165874058716733,-0.0179937793481434,
0.0589892825605912));
#29559=CARTESIAN_POINT('Ctrl Pts',(-0.166608027402805,-0.00892999310321975,
0.0584384547184699));
#29560=CARTESIAN_POINT('Ctrl Pts',(-0.166599933793721,0.000148525849286412,
0.0578834975791045));
#29561=CARTESIAN_POINT('Ctrl Pts',(-0.16659993550101,0.000146598291904576,
0.0578519636609792));
#29562=CARTESIAN_POINT('Ctrl Pts',(-0.166590005045457,0.0114319498000848,
0.0570962429544575));
#29563=CARTESIAN_POINT('Ctrl Pts',(-0.165432367526071,0.0226678146584585,
0.0563405222479359));
#29564=CARTESIAN_POINT('Ctrl Pts',(-0.163162736528589,0.0336672156333481,
0.0555848015414142));
#29565=CARTESIAN_POINT('Ctrl Pts',(-0.161492128961394,0.0417635460604719,
0.0550285381081066));
#29566=CARTESIAN_POINT('Ctrl Pts',(-0.159212613341451,0.0497585272529405,
0.054472274674799));
#29567=CARTESIAN_POINT('Ctrl Pts',(-0.156342830367367,0.0575541431412264,
0.0539160112414913));
#29568=CARTESIAN_POINT('Ctrl Pts',(-0.156342830139253,0.0575541437608846,
0.0733422317177101));
#29569=CARTESIAN_POINT('Ctrl Pts',(-0.158731568701549,0.0510652600265771,
0.0737809469876743));
#29570=CARTESIAN_POINT('Ctrl Pts',(-0.160714366236737,0.0444330332437999,
0.0742078829840241));
#29571=CARTESIAN_POINT('Ctrl Pts',(-0.164155729589764,0.0296179894956481,
0.0751392325202815));
#29572=CARTESIAN_POINT('Ctrl Pts',(-0.165426253207922,0.0214119367621838,
0.0756406851706057));
#29573=CARTESIAN_POINT('Ctrl Pts',(-0.166428115376428,0.00875472451724462,
0.0764325626370999));
#29574=CARTESIAN_POINT('Ctrl Pts',(-0.16660137025941,0.00435192527033506,
0.0767115180698701));
#29575=CARTESIAN_POINT('Ctrl Pts',(-0.166599419703309,-0.0018801275691792,
0.0771177228895507));
#29576=CARTESIAN_POINT('Ctrl Pts',(-0.166568761872395,-0.00370787877507483,
0.077238240040562));
#29577=CARTESIAN_POINT('Ctrl Pts',(-0.166458179634013,-0.0070347046420041,
0.0774607273232043));
#29578=CARTESIAN_POINT('Ctrl Pts',(-0.166388057010376,-0.00853383941535998,
0.0775621891408969));
#29579=CARTESIAN_POINT('Ctrl Pts',(-0.166159419576139,-0.0123239897934098,
0.0778215854643722));
#29580=CARTESIAN_POINT('Ctrl Pts',(-0.16597377233047,-0.014612973676749,
0.0779808597947969));
#29581=CARTESIAN_POINT('Ctrl Pts',(-0.165040542856652,-0.0237667937472071,
0.0786264356294616));
#29582=CARTESIAN_POINT('Ctrl Pts',(-0.163913836992091,-0.0305856087662146,
0.0791265682126842));
#29583=CARTESIAN_POINT('Ctrl Pts',(-0.159519813605947,-0.0497055720309509,
0.0805538325089489));
#29584=CARTESIAN_POINT('Ctrl Pts',(-0.155262421133131,-0.0617325198928841,
0.0814780379372874));
#29585=CARTESIAN_POINT('Ctrl Pts',(-0.148236899397541,-0.076106113386055,
0.0825843105672843));
#29586=CARTESIAN_POINT('Ctrl Pts',(-0.146709724896258,-0.079009987410744,
0.0828082094017459));
#29587=CARTESIAN_POINT('Ctrl Pts',(-0.143829337061509,-0.0841150644512558,
0.0832029108509888));
#29588=CARTESIAN_POINT('Ctrl Pts',(-0.142508841221774,-0.0863333870869027,
0.083374807973937));
#29589=CARTESIAN_POINT('Ctrl Pts',(-0.139495127439928,-0.0911384725099449,
0.0837484823681112));
#29590=CARTESIAN_POINT('Ctrl Pts',(-0.137780373782819,-0.0937106311398644,
0.0839493851038715));
#29591=CARTESIAN_POINT('Ctrl Pts',(-0.131812663653349,-0.102144040124414,
0.0846129280015447));
#29592=CARTESIAN_POINT('Ctrl Pts',(-0.127249291977263,-0.107775775054225,
0.0850637453988705));
#29593=CARTESIAN_POINT('Ctrl Pts',(-0.116616450167382,-0.119277375299619,
0.0860264985571724));
#29594=CARTESIAN_POINT('Ctrl Pts',(-0.110438886896686,-0.125018934101555,
0.0865349149072511));
#29595=CARTESIAN_POINT('Ctrl Pts',(-0.0998806502011885,-0.133436262561785,
0.087370585027736));
#29596=CARTESIAN_POINT('Ctrl Pts',(-0.0957649046141287,-0.136420137754885,
0.0876894342529002));
#29597=CARTESIAN_POINT('Ctrl Pts',(-0.0899892939877273,-0.140217121976961,
0.0881371598444122));
#29598=CARTESIAN_POINT('Ctrl Pts',(-0.088442498884166,-0.141197868345446,
0.0882570987166956));
#29599=CARTESIAN_POINT('Ctrl Pts',(-0.08560925556339,-0.142929468948643,
0.088477449447536));
#29600=CARTESIAN_POINT('Ctrl Pts',(-0.084328378741345,-0.143688907055701,
0.0885773327247469));
#29601=CARTESIAN_POINT('Ctrl Pts',(-0.0813994549110805,-0.145372825718199,
0.0888065181417483));
#29602=CARTESIAN_POINT('Ctrl Pts',(-0.0797456869976875,-0.146286548653578,
0.0889364029348654));
#29603=CARTESIAN_POINT('Ctrl Pts',(-0.0737029494236593,-0.149492308915269,
0.0894117491729622));
#29604=CARTESIAN_POINT('Ctrl Pts',(-0.0692281786999842,-0.151616375908853,
0.0897651155026648));
#29605=CARTESIAN_POINT('Ctrl Pts',(-0.0546984672671851,-0.157735891793943,
0.0909031406874023));
#29606=CARTESIAN_POINT('Ctrl Pts',(-0.0443449302284133,-0.16095368818613,
0.0916983423316182));
#29607=CARTESIAN_POINT('Ctrl Pts',(-0.028043655700116,-0.164326196580587,
0.0928864723613127));
#29608=CARTESIAN_POINT('Ctrl Pts',(-0.0222762787499561,-0.165206920140448,
0.0932955254708856));
#29609=CARTESIAN_POINT('Ctrl Pts',(-0.013554452584087,-0.166073612141291,
0.0938965596568784));
#29610=CARTESIAN_POINT('Ctrl Pts',(-0.0106276164896238,-0.166286570451353,
0.0940953540341691));
#29611=CARTESIAN_POINT('Ctrl Pts',(-0.0050990113525662,-0.166542251475757,
0.0944657765890206));
#29612=CARTESIAN_POINT('Ctrl Pts',(-0.00249893778050202,-0.166601554765496,
0.0946378718472534));
#29613=CARTESIAN_POINT('Ctrl Pts',(0.00363072837520992,-0.16659781704208,
0.0950391938336234));
#29614=CARTESIAN_POINT('Ctrl Pts',(0.00715909356496179,-0.166483528040061,
0.095266759389338));
#29615=CARTESIAN_POINT('Ctrl Pts',(0.0182055568661425,-0.16577383560427,
0.0959712970743524));
#29616=CARTESIAN_POINT('Ctrl Pts',(0.0256886009519762,-0.164780211620841,
0.096436609201887));
#29617=CARTESIAN_POINT('Ctrl Pts',(0.0444685958962533,-0.16097560912945,
0.0976093198693883));
#29618=CARTESIAN_POINT('Ctrl Pts',(0.0555838564147703,-0.15748323447659,
0.0983073280844476));
#29619=CARTESIAN_POINT('Ctrl Pts',(0.0682753030885989,-0.151983370873411,
0.0991989393429221));
#29620=CARTESIAN_POINT('Ctrl Pts',(0.0702889323316825,-0.151062658622837,
0.0993434731960589));
#29621=CARTESIAN_POINT('Ctrl Pts',(0.0736272800862409,-0.149455037228192,
0.0995892598562026));
#29622=CARTESIAN_POINT('Ctrl Pts',(0.0749621564246813,-0.148789984166298,
0.0996892541357239));
#29623=CARTESIAN_POINT('Ctrl Pts',(0.0779536206656289,-0.147249119968105,
0.0999174396498739));
#29624=CARTESIAN_POINT('Ctrl Pts',(0.0796045475391126,-0.146363197318752,
0.100046182497588));
#29625=CARTESIAN_POINT('Ctrl Pts',(0.0854320084960557,-0.143108302141588,
0.10050980369882));
#29626=CARTESIAN_POINT('Ctrl Pts',(0.089520384598724,-0.140587007099171,
0.100852103650648));
#29627=CARTESIAN_POINT('Ctrl Pts',(0.101796270308284,-0.132263746396208,
0.101921751699661));
#29628=CARTESIAN_POINT('Ctrl Pts',(0.109573941582535,-0.125895777948557,
0.102658898418855));
#29629=CARTESIAN_POINT('Ctrl Pts',(0.121299019503133,-0.114381338025699,
0.103837663887317));
#29630=CARTESIAN_POINT('Ctrl Pts',(0.12560469053346,-0.109635859558593,
0.104289156339918));
#29631=CARTESIAN_POINT('Ctrl Pts',(0.131544946046503,-0.102278099295703,
0.104939686720676));
#29632=CARTESIAN_POINT('Ctrl Pts',(0.133397359197836,-0.0998500332202134,
0.10514716007322));
#29633=CARTESIAN_POINT('Ctrl Pts',(0.136692251923254,-0.0952757279756303,
0.1055253754771));
#29634=CARTESIAN_POINT('Ctrl Pts',(0.138153495069931,-0.0931442384514785,
0.105696808662908));
#29635=CARTESIAN_POINT('Ctrl Pts',(0.141383066170064,-0.0881900031280215,
0.106084984690867));
#29636=CARTESIAN_POINT('Ctrl Pts',(0.143117547028203,-0.0853464601952437,
0.106300424735804));
#29637=CARTESIAN_POINT('Ctrl Pts',(0.146640467112326,-0.0791611164753061,
0.106755206475045));
#29638=CARTESIAN_POINT('Ctrl Pts',(0.148402480185767,-0.0758064357466371,
0.106993617703762));
#29639=CARTESIAN_POINT('Ctrl Pts',(0.153470499573445,-0.065302178370474,
0.10771987981065));
#29640=CARTESIAN_POINT('Ctrl Pts',(0.156385275056003,-0.0579760350646747,
0.108198024157016));
#29641=CARTESIAN_POINT('Ctrl Pts',(0.16113041955213,-0.0430488687509527,
0.109155576867591));
#29642=CARTESIAN_POINT('Ctrl Pts',(0.162966247267559,-0.0354710286416337,
0.109633889342117));
#29643=CARTESIAN_POINT('Ctrl Pts',(0.164650804379381,-0.0255149581869932,
0.110283308696252));
#29644=CARTESIAN_POINT('Ctrl Pts',(0.164988859264248,-0.0232287635746161,
0.110433865791516));
#29645=CARTESIAN_POINT('Ctrl Pts',(0.165468015784193,-0.0194461394340785,
0.110686427201184));
#29646=CARTESIAN_POINT('Ctrl Pts',(0.165636610683883,-0.017953540089206,
0.110786988443198));
#29647=CARTESIAN_POINT('Ctrl Pts',(0.165964679388636,-0.0146489846224926,
0.111011883307279));
#29648=CARTESIAN_POINT('Ctrl Pts',(0.166114693332733,-0.0128364903485683,
0.111136659037984));
#29649=CARTESIAN_POINT('Ctrl Pts',(0.166521791127041,-0.00669660083592011,
0.111563350221079));
#29650=CARTESIAN_POINT('Ctrl Pts',(0.166639628152342,-0.00236201361199573,
0.111871273478218));
#29651=CARTESIAN_POINT('Ctrl Pts',(0.166493356417696,0.00999566398742779,
0.11275983799172));
#29652=CARTESIAN_POINT('Ctrl Pts',(0.165818805075273,0.0180020400740708,
0.113347865646239));
#29653=CARTESIAN_POINT('Ctrl Pts',(0.163340509477403,0.0337319062118775,
0.114501662729232));
#29654=CARTESIAN_POINT('Ctrl Pts',(0.161557491146787,0.0414387455357853,
0.115066166066754));
#29655=CARTESIAN_POINT('Ctrl Pts',(0.158217411307254,0.0522949462364381,
0.115854295690599));
#29656=CARTESIAN_POINT('Ctrl Pts',(0.157098191252812,0.0555668249778272,
0.116090980937147));
#29657=CARTESIAN_POINT('Ctrl Pts',(0.154962537692382,0.0612282431337444,
0.116499378285595));
#29658=CARTESIAN_POINT('Ctrl Pts',(0.153990608941746,0.0636331636134118,
0.116672496318482));
#29659=CARTESIAN_POINT('Ctrl Pts',(0.15178507890664,0.0687436173802246,
0.117040021672601));
#29660=CARTESIAN_POINT('Ctrl Pts',(0.150534400460544,0.0714408232299727,
0.11723377517437));
#29661=CARTESIAN_POINT('Ctrl Pts',(0.146484711528603,0.0795951574184007,
0.117820316762781));
#29662=CARTESIAN_POINT('Ctrl Pts',(0.143455988434335,0.0849326249752648,
0.118205144931576));
#29663=CARTESIAN_POINT('Ctrl Pts',(0.134275106575857,0.0992137338964782,
0.11925524156172));
#29664=CARTESIAN_POINT('Ctrl Pts',(0.127534271121405,0.10774117659579,0.119905035831017));
#29665=CARTESIAN_POINT('Ctrl Pts',(0.116866608477696,0.118820595415067,
0.120862540862049));
#29666=CARTESIAN_POINT('Ctrl Pts',(0.113588373994323,0.121958238504356,
0.12114923180295));
#29667=CARTESIAN_POINT('Ctrl Pts',(0.108783723971115,0.126194926374547,
0.121566149143035));
#29668=CARTESIAN_POINT('Ctrl Pts',(0.107360251990939,0.12740813774358,0.121689293944694));
#29669=CARTESIAN_POINT('Ctrl Pts',(0.104764995533598,0.129545675696416,
0.121913784456072));
#29670=CARTESIAN_POINT('Ctrl Pts',(0.103600698997363,0.130478660696752,
0.1220145340679));
#29671=CARTESIAN_POINT('Ctrl Pts',(0.100673599456555,0.13276035681628,0.122267800637389));
#29672=CARTESIAN_POINT('Ctrl Pts',(0.0988961522915688,0.134089655855697,
0.122421517376751));
#29673=CARTESIAN_POINT('Ctrl Pts',(0.0948568619017735,0.136986519536498,
0.122769725219848));
#29674=CARTESIAN_POINT('Ctrl Pts',(0.0925816622860175,0.138534345640703,
0.122965100443091));
#29675=CARTESIAN_POINT('Ctrl Pts',(0.0848292208046589,0.143532077417796,
0.123625819111869));
#29676=CARTESIAN_POINT('Ctrl Pts',(0.0791895631431683,0.146718988234542,
0.124098128204155));
#29677=CARTESIAN_POINT('Ctrl Pts',(0.0644873049629697,0.153931933053163,
0.12528975302735));
#29678=CARTESIAN_POINT('Ctrl Pts',(0.0552231197177241,0.157493213162172,
0.126003855350414));
#29679=CARTESIAN_POINT('Ctrl Pts',(0.0422968848716561,0.16118011439569,
0.126937860618442));
#29680=CARTESIAN_POINT('Ctrl Pts',(0.0388673222194977,0.162041322837214,
0.127180178827783));
#29681=CARTESIAN_POINT('Ctrl Pts',(0.0328710030423227,0.163345716702232,
0.12759474474347));
#29682=CARTESIAN_POINT('Ctrl Pts',(0.0303165747025702,0.163839044876704,
0.127768537166059));
#29683=CARTESIAN_POINT('Ctrl Pts',(0.0248607737704458,0.164760725825824,
0.128134205077161));
#29684=CARTESIAN_POINT('Ctrl Pts',(0.0219575128959662,0.16517271035205,
0.128325506240987));
#29685=CARTESIAN_POINT('Ctrl Pts',(0.0132716063530174,0.166172184108819,
0.128889417174658));
#29686=CARTESIAN_POINT('Ctrl Pts',(0.00746731810995964,0.16653401965539,
0.129255042994606));
#29687=CARTESIAN_POINT('Ctrl Pts',(-0.00791475756262302,0.166686878683553,
0.130208698672406));
#29688=CARTESIAN_POINT('Ctrl Pts',(-0.0174751900192594,0.165957145666238,
0.130785111547883));
#29689=CARTESIAN_POINT('Ctrl Pts',(-0.0327114808037987,0.163462409139054,
0.131736586375272));
#29690=CARTESIAN_POINT('Ctrl Pts',(-0.0384482258989823,0.162208878508564,
0.132102921378725));
#29691=CARTESIAN_POINT('Ctrl Pts',(-0.0458794555952046,0.16016871334915,
0.132601984904978));
#29692=CARTESIAN_POINT('Ctrl Pts',(-0.0476443715759621,0.159652605171078,
0.132722378729787));
#29693=CARTESIAN_POINT('Ctrl Pts',(-0.0508234901009825,0.158665540073413,
0.132943246903609));
#29694=CARTESIAN_POINT('Ctrl Pts',(-0.052240524163696,0.158204640056292,
0.133043181342801));
#29695=CARTESIAN_POINT('Ctrl Pts',(-0.0554341705340749,0.157118297006656,
0.133271984687267));
#29696=CARTESIAN_POINT('Ctrl Pts',(-0.05720655624845,0.156481678290817,
0.133401423888684));
#29697=CARTESIAN_POINT('Ctrl Pts',(-0.0635423209783082,0.154083932177527,
0.133872085045294));
#29698=CARTESIAN_POINT('Ctrl Pts',(-0.0680381110361262,0.152152198135693,
0.134221016081875));
#29699=CARTESIAN_POINT('Ctrl Pts',(-0.0818891571540374,0.145464030439865,
0.135330893849588));
#29700=CARTESIAN_POINT('Ctrl Pts',(-0.0908851122010791,0.140019776222052,
0.136102091463427));
#29701=CARTESIAN_POINT('Ctrl Pts',(-0.104211792718098,0.130125879207635,
0.137289251566725));
#29702=CARTESIAN_POINT('Ctrl Pts',(-0.108910971520107,0.126219086706141,
0.137718533451768));
#29703=CARTESIAN_POINT('Ctrl Pts',(-0.115560970176955,0.120041819804754,
0.138341549979697));
#29704=CARTESIAN_POINT('Ctrl Pts',(-0.117682133397078,0.117963103504322,
0.138542916082223));
#29705=CARTESIAN_POINT('Ctrl Pts',(-0.12155019648595,0.113964198452355,
0.1389155621846));
#29706=CARTESIAN_POINT('Ctrl Pts',(-0.123309959121088,0.112057771109521,
0.139087376881126));
#29707=CARTESIAN_POINT('Ctrl Pts',(-0.127313232954601,0.107512285988707,
0.139484261169915));
#29708=CARTESIAN_POINT('Ctrl Pts',(-0.129520439022757,0.104842784943497,
0.139707790081093));
#29709=CARTESIAN_POINT('Ctrl Pts',(-0.136909041057994,0.0953168511878716,
0.1404760362223));
#29710=CARTESIAN_POINT('Ctrl Pts',(-0.141642233818867,0.0881299368017429,
0.141004178464014));
#29711=CARTESIAN_POINT('Ctrl Pts',(-0.149897036826922,0.0731992596415132,
0.142046693057115));
#29712=CARTESIAN_POINT('Ctrl Pts',(-0.153420822366363,0.0654916244530294,
0.142559592849312));
#29713=CARTESIAN_POINT('Ctrl Pts',(-0.156342827686701,0.0575541504231135,
0.143092354725971));
#29714=CARTESIAN_POINT('Origin',(0.,0.,0.2));
#29715=CARTESIAN_POINT('',(-0.156342826453536,0.0575541537729419,0.213195533534746));
#29716=CARTESIAN_POINT('',(-0.156342830468371,0.0575541428668533,0.193775546749386));
#29717=CARTESIAN_POINT('',(-0.156342830367367,0.0575541431412265,0.2));
#29718=CARTESIAN_POINT('Ctrl Pts',(-0.156342830468371,0.0575541428668533,
0.193775546749386));
#29719=CARTESIAN_POINT('Ctrl Pts',(-0.155590902035664,0.0595967172780662,
0.193634523991676));
#29720=CARTESIAN_POINT('Ctrl Pts',(-0.154798947284683,0.0616245505665048,
0.193494759036807));
#29721=CARTESIAN_POINT('Ctrl Pts',(-0.149148386705545,0.0752959884263723,
0.192552560946363));
#29722=CARTESIAN_POINT('Ctrl Pts',(-0.143020724015013,0.0863702545555471,
0.191793645064661));
#29723=CARTESIAN_POINT('Ctrl Pts',(-0.131629352358015,0.102364767391474,
0.190589141621333));
#29724=CARTESIAN_POINT('Ctrl Pts',(-0.127200442878323,0.107818632368816,
0.190154220094669));
#29725=CARTESIAN_POINT('Ctrl Pts',(-0.121059808696202,0.114473725183815,
0.189567839731538));
#29726=CARTESIAN_POINT('Ctrl Pts',(-0.119650909384679,0.115945547388078,
0.1894342989407));
#29727=CARTESIAN_POINT('Ctrl Pts',(-0.117172763263459,0.11844109634221,
0.189200306920669));
#29728=CARTESIAN_POINT('Ctrl Pts',(-0.116116256578284,0.11947704506158,
0.189100780647165));
#29729=CARTESIAN_POINT('Ctrl Pts',(-0.11362150329092,0.121858906923574,
0.188866231017912));
#29730=CARTESIAN_POINT('Ctrl Pts',(-0.112173021772356,0.123193553000966,
0.188730467904189));
#29731=CARTESIAN_POINT('Ctrl Pts',(-0.106273048007432,0.128439526015559,
0.188180325182671));
#29732=CARTESIAN_POINT('Ctrl Pts',(-0.10163827341088,0.132137506705327,
0.187754626058332));
#29733=CARTESIAN_POINT('Ctrl Pts',(-0.0890019407409316,0.14116101133562,
0.186628763234608));
#29734=CARTESIAN_POINT('Ctrl Pts',(-0.0807184683879038,0.146055909391843,
0.185925283003518));
#29735=CARTESIAN_POINT('Ctrl Pts',(-0.0668126365563965,0.152726855323599,
0.184824564205049));
#29736=CARTESIAN_POINT('Ctrl Pts',(-0.0614373858124439,0.154967357349003,
0.18441629444234));
#29737=CARTESIAN_POINT('Ctrl Pts',(-0.0531950930173772,0.15790639534627,
0.183816252723021));
#29738=CARTESIAN_POINT('Ctrl Pts',(-0.050409231874744,0.158817690631178,
0.183617696139746));
#29739=CARTESIAN_POINT('Ctrl Pts',(-0.0451115338023832,0.160397181358762,
0.183247701624332));
#29740=CARTESIAN_POINT('Ctrl Pts',(-0.0426053245089632,0.161081016528133,
0.183075797932162));
#29741=CARTESIAN_POINT('Ctrl Pts',(-0.0366628688997014,0.162554044933457,
0.182674948952671));
#29742=CARTESIAN_POINT('Ctrl Pts',(-0.033215483821488,0.163293349532899,
0.182447659854307));
#29743=CARTESIAN_POINT('Ctrl Pts',(-0.0197395081635329,0.165738831654405,
0.181575877948731));
#29744=CARTESIAN_POINT('Ctrl Pts',(-0.00958645302438748,0.166634729867992,
0.18095614298273));
#29745=CARTESIAN_POINT('Ctrl Pts',(0.00689262840600602,0.166576798932987,
0.179949859274636));
#29746=CARTESIAN_POINT('Ctrl Pts',(0.0131928945247958,0.166196500623152,
0.17956456532207));
#29747=CARTESIAN_POINT('Ctrl Pts',(0.0221521436094454,0.165143004859335,
0.17899841390869));
#29748=CARTESIAN_POINT('Ctrl Pts',(0.0248399578027051,0.164760142030998,
0.178826162305901));
#29749=CARTESIAN_POINT('Ctrl Pts',(0.029684533436926,0.163948827837131,
0.178509408415356));
#29750=CARTESIAN_POINT('Ctrl Pts',(0.0318444763770192,0.163543015218502,
0.178365897848983));
#29751=CARTESIAN_POINT('Ctrl Pts',(0.0354527561390169,0.162790901329742,
0.178121344799342));
#29752=CARTESIAN_POINT('Ctrl Pts',(0.0369055734403406,0.162467701013107,
0.178021531692569));
#29753=CARTESIAN_POINT('Ctrl Pts',(0.0401827612432522,0.161692416017313,
0.177793123764577));
#29754=CARTESIAN_POINT('Ctrl Pts',(0.0420040120680982,0.161228886601921,
0.177663962869292));
#29755=CARTESIAN_POINT('Ctrl Pts',(0.0482462721053503,0.159527221104174,
0.17721447277793));
#29756=CARTESIAN_POINT('Ctrl Pts',(0.0526234378921112,0.158137292776665,
0.176887490232039));
#29757=CARTESIAN_POINT('Ctrl Pts',(0.0670704799769513,0.152883528423915,
0.175779823493162));
#29758=CARTESIAN_POINT('Ctrl Pts',(0.0768229309850354,0.14822308765669,
0.174986498453452));
#29759=CARTESIAN_POINT('Ctrl Pts',(0.09129374676517,0.139493449006873,0.173777628477773));
#29760=CARTESIAN_POINT('Ctrl Pts',(0.0963535057220681,0.136047741278424,
0.173347574493332));
#29761=CARTESIAN_POINT('Ctrl Pts',(0.103570467091752,0.130527884452616,
0.172723881325657));
#29762=CARTESIAN_POINT('Ctrl Pts',(0.105879640505845,0.128661859059181,
0.172522574862355));
#29763=CARTESIAN_POINT('Ctrl Pts',(0.110108259199288,0.12505375008256,0.172150231457662));
#29764=CARTESIAN_POINT('Ctrl Pts',(0.112039275086575,0.123326685174374,
0.171978655809551));
#29765=CARTESIAN_POINT('Ctrl Pts',(0.116448399811759,0.119194170961235,
0.17158265686525));
#29766=CARTESIAN_POINT('Ctrl Pts',(0.118893599701594,0.116755277795925,
0.171359759730468));
#29767=CARTESIAN_POINT('Ctrl Pts',(0.128937022687202,0.10609475610264,0.170426264555767));
#29768=CARTESIAN_POINT('Ctrl Pts',(0.135772186646139,0.0971946163639783,
0.169747273057942));
#29769=CARTESIAN_POINT('Ctrl Pts',(0.144689020781048,0.0827870663522616,
0.168711724052762));
#29770=CARTESIAN_POINT('Ctrl Pts',(0.147459278694621,0.0777455110692841,
0.168359194745196));
#29771=CARTESIAN_POINT('Ctrl Pts',(0.151090206733628,0.0702424552119781,
0.167834790130663));
#29772=CARTESIAN_POINT('Ctrl Pts',(0.152162694457713,0.0678878933111996,
0.167670239700088));
#29773=CARTESIAN_POINT('Ctrl Pts',(0.154014696946497,0.0635573806249942,
0.167365946902588));
#29774=CARTESIAN_POINT('Ctrl Pts',(0.15481208495677,0.0615896483756529,
0.167227074075299));
#29775=CARTESIAN_POINT('Ctrl Pts',(0.156102165787375,0.0582226140286415,
0.16698754336893));
#29776=CARTESIAN_POINT('Ctrl Pts',(0.156614147729788,0.0568310422347938,
0.166887973384925));
#29777=CARTESIAN_POINT('Ctrl Pts',(0.157739271601525,0.0536422158914378,
0.166658363647349));
#29778=CARTESIAN_POINT('Ctrl Pts',(0.158340340527467,0.0518411118861126,
0.166527716714829));
#29779=CARTESIAN_POINT('Ctrl Pts',(0.160345837373133,0.0454710750182586,
0.166063243410058));
#29780=CARTESIAN_POINT('Ctrl Pts',(0.161584218240311,0.0408526438405171,
0.165722224096999));
#29781=CARTESIAN_POINT('Ctrl Pts',(0.164917292327175,0.0258743442318358,
0.16461507909304));
#29782=CARTESIAN_POINT('Ctrl Pts',(0.166226155251371,0.015365034748537,
0.163838291744793));
#29783=CARTESIAN_POINT('Ctrl Pts',(0.166705620416753,-0.00126067209229211,
0.162648997264998));
#29784=CARTESIAN_POINT('Ctrl Pts',(0.166549233607682,-0.00732946559802726,
0.16222265838447));
#29785=CARTESIAN_POINT('Ctrl Pts',(0.165824269247632,-0.0163292683755717,
0.161602980602769));
#29786=CARTESIAN_POINT('Ctrl Pts',(0.165507737203547,-0.0192749621936129,
0.161402128481368));
#29787=CARTESIAN_POINT('Ctrl Pts',(0.164767340939304,-0.0247789865963232,
0.161030178585746));
#29788=CARTESIAN_POINT('Ctrl Pts',(0.164361987864978,-0.0273388560043736,
0.160858554083711));
#29789=CARTESIAN_POINT('Ctrl Pts',(0.163275616212723,-0.0332961300145443,
0.160461791025231));
#29790=CARTESIAN_POINT('Ctrl Pts',(0.162548009707945,-0.0366838714002988,
0.160238199069174));
#29791=CARTESIAN_POINT('Ctrl Pts',(0.159782317291051,-0.0478522076821318,
0.159505033078864));
#29792=CARTESIAN_POINT('Ctrl Pts',(0.157286713533681,-0.0555079323622843,
0.159009472486989));
#29793=CARTESIAN_POINT('Ctrl Pts',(0.151260348080733,-0.0702735030734023,
0.158034106395609));
#29794=CARTESIAN_POINT('Ctrl Pts',(0.147755980486726,-0.0773706424300446,
0.157555295301287));
#29795=CARTESIAN_POINT('Ctrl Pts',(0.141587242675839,-0.087904036955393,
0.156793263465665));
#29796=CARTESIAN_POINT('Ctrl Pts',(0.139270442342352,-0.0915303464660786,
0.156520554856046));
#29797=CARTESIAN_POINT('Ctrl Pts',(0.135781533181735,-0.0965516594783797,
0.156121854157343));
#29798=CARTESIAN_POINT('Ctrl Pts',(0.134722728798156,-0.0980236366031589,
0.156002268099135));
#29799=CARTESIAN_POINT('Ctrl Pts',(0.132744028542351,-0.100681851957852,
0.155780711342193));
#29800=CARTESIAN_POINT('Ctrl Pts',(0.131831761309077,-0.101873443162347,
0.155679223821334));
#29801=CARTESIAN_POINT('Ctrl Pts',(0.129473301841012,-0.104869302236903,
0.15541868250659));
#29802=CARTESIAN_POINT('Ctrl Pts',(0.12800545952853,-0.106656023792567,
0.155258256550875));
#29803=CARTESIAN_POINT('Ctrl Pts',(0.119362343667243,-0.116741326940189,
0.154326027947316));
#29804=CARTESIAN_POINT('Ctrl Pts',(0.111418820572436,-0.124345208204153,
0.153518728661181));
#29805=CARTESIAN_POINT('Ctrl Pts',(0.0970805142324918,-0.135585746186237,
0.152197679270653));
#29806=CARTESIAN_POINT('Ctrl Pts',(0.0910885028183082,-0.139681876623671,
0.151678087187401));
#29807=CARTESIAN_POINT('Ctrl Pts',(0.0815306895320326,-0.145338107714882,
0.150902313722887));
#29808=CARTESIAN_POINT('Ctrl Pts',(0.0781459892782143,-0.147185690476561,
0.150636877706001));
#29809=CARTESIAN_POINT('Ctrl Pts',(0.072341070658559,-0.150097615404206,
0.150196680025051));
#29810=CARTESIAN_POINT('Ctrl Pts',(0.0699542688818522,-0.151224754272853,
0.150019782273406));
#29811=CARTESIAN_POINT('Ctrl Pts',(0.0649767576493632,-0.153432242642399,
0.149658827159847));
#29812=CARTESIAN_POINT('Ctrl Pts',(0.062383500741416,-0.154504797749321,
0.149475082271993));
#29813=CARTESIAN_POINT('Ctrl Pts',(0.0551518849417202,-0.157283964654651,
0.148973432313726));
#29814=CARTESIAN_POINT('Ctrl Pts',(0.0504626632964563,-0.158850566446669,
0.148660165730293));
#29815=CARTESIAN_POINT('Ctrl Pts',(0.0342057473093257,-0.16348901522866,
0.14760408728698));
#29816=CARTESIAN_POINT('Ctrl Pts',(0.0223815903126587,-0.165522640945428,
0.146888982761485));
#29817=CARTESIAN_POINT('Ctrl Pts',(0.00530916725011301,-0.16659478022368,
0.145828901672124));
#29818=CARTESIAN_POINT('Ctrl Pts',(0.000164819562926936,-0.166679244793301,
0.1455054857326));
#29819=CARTESIAN_POINT('Ctrl Pts',(-0.00688125831788664,-0.166468755776044,
0.145047256534455));
#29820=CARTESIAN_POINT('Ctrl Pts',(-0.00878663292579114,-0.16637906309048,
0.144921806069434));
#29821=CARTESIAN_POINT('Ctrl Pts',(-0.0121719502584552,-0.166161394621268,
0.144695509294848));
#29822=CARTESIAN_POINT('Ctrl Pts',(-0.0136524385420175,-0.166046306084744,
0.144595336410489));
#29823=CARTESIAN_POINT('Ctrl Pts',(-0.0172784335945231,-0.165715614264605,
0.144347098568819));
#29824=CARTESIAN_POINT('Ctrl Pts',(-0.0194215619929738,-0.165478128081504,
0.144197947602235));
#29825=CARTESIAN_POINT('Ctrl Pts',(-0.0318903552419107,-0.163850885983391,
0.143318251045313));
#29826=CARTESIAN_POINT('Ctrl Pts',(-0.0420713689804899,-0.161536619775714,
0.142553668126449));
#29827=CARTESIAN_POINT('Ctrl Pts',(-0.0604440373342564,-0.155504501269342,
0.141148708857975));
#29828=CARTESIAN_POINT('Ctrl Pts',(-0.0686830615100061,-0.152045416485342,
0.140508302268918));
#29829=CARTESIAN_POINT('Ctrl Pts',(-0.0797162728052445,-0.146332294961448,
0.139645447249649));
#29830=CARTESIAN_POINT('Ctrl Pts',(-0.0827748121162779,-0.144624197098786,
0.139405491890529));
#29831=CARTESIAN_POINT('Ctrl Pts',(-0.0880020640675056,-0.141484737043617,
0.138993700586152));
#29832=CARTESIAN_POINT('Ctrl Pts',(-0.0901952663251361,-0.14009678561939,
0.138820374482131));
#29833=CARTESIAN_POINT('Ctrl Pts',(-0.0948036295396262,-0.137027317600559,
0.138454555610715));
#29834=CARTESIAN_POINT('Ctrl Pts',(-0.097208494089901,-0.135331904610645,
0.138262662743777));
#29835=CARTESIAN_POINT('Ctrl Pts',(-0.104302604970533,-0.13004387120222,
0.137692189543588));
#29836=CARTESIAN_POINT('Ctrl Pts',(-0.108847131272712,-0.126264620886427,
0.137320878541945));
#29837=CARTESIAN_POINT('Ctrl Pts',(-0.121052015337821,-0.114965226557501,
0.136290488975881));
#29838=CARTESIAN_POINT('Ctrl Pts',(-0.128199964147166,-0.106936194929914,
0.135647424750198));
#29839=CARTESIAN_POINT('Ctrl Pts',(-0.137436833345354,-0.0942922007309623,
0.134675459640571));
#29840=CARTESIAN_POINT('Ctrl Pts',(-0.140168561216021,-0.0901813033894219,
0.13436460105883));
#29841=CARTESIAN_POINT('Ctrl Pts',(-0.14368688933537,-0.0843397671946393,
0.133921024278536));
#29842=CARTESIAN_POINT('Ctrl Pts',(-0.144632588931071,-0.0827075082849191,
0.133796883946168));
#29843=CARTESIAN_POINT('Ctrl Pts',(-0.146274149461862,-0.0797599295986753,
0.13357171084227));
#29844=CARTESIAN_POINT('Ctrl Pts',(-0.146980452351105,-0.0784507436157472,
0.13347130949505));
#29845=CARTESIAN_POINT('Ctrl Pts',(-0.148681773339479,-0.0751935794775488,
0.133220655932239));
#29846=CARTESIAN_POINT('Ctrl Pts',(-0.149656091040029,-0.0732352193604272,
0.133069260942201));
#29847=CARTESIAN_POINT('Ctrl Pts',(-0.155630203440044,-0.0606100273830332,
0.132091473816664));
#29848=CARTESIAN_POINT('Ctrl Pts',(-0.159525009679967,-0.0494579107513059,
0.131222514451045));
#29849=CARTESIAN_POINT('Ctrl Pts',(-0.163508981470423,-0.0324465017915527,
0.129957685487496));
#29850=CARTESIAN_POINT('Ctrl Pts',(-0.164522156241036,-0.0268408734114021,
0.129549674378269));
#29851=CARTESIAN_POINT('Ctrl Pts',(-0.165801581778434,-0.0168653587799454,
0.128842252073758));
#29852=CARTESIAN_POINT('Ctrl Pts',(-0.166186499120239,-0.0125163247783635,
0.128539949306401));
#29853=CARTESIAN_POINT('Ctrl Pts',(-0.166533192612882,-0.00544373934164217,
0.128058017625432));
#29854=CARTESIAN_POINT('Ctrl Pts',(-0.166599819476558,-0.00272767396764765,
0.127875232829596));
#29855=CARTESIAN_POINT('Ctrl Pts',(-0.16660017871232,0.00268931537233102,
0.127514860709453));
#29856=CARTESIAN_POINT('Ctrl Pts',(-0.166534704148222,0.00538940658455499,
0.127337303502265));
#29857=CARTESIAN_POINT('Ctrl Pts',(-0.166196755190487,0.0123434026956459,
0.126884545791726));
#29858=CARTESIAN_POINT('Ctrl Pts',(-0.165826640331689,0.016590693821595,
0.126612434879661));
#29859=CARTESIAN_POINT('Ctrl Pts',(-0.164608846604945,0.0262592663037333,
0.125998963190014));
#29860=CARTESIAN_POINT('Ctrl Pts',(-0.16365552465737,0.0316622257808932,
0.125660532292121));
#29861=CARTESIAN_POINT('Ctrl Pts',(-0.160847749804357,0.0439860623525317,
0.12488598223878));
#29862=CARTESIAN_POINT('Ctrl Pts',(-0.15881135259047,0.0508485284896533,
0.124452809833924));
#29863=CARTESIAN_POINT('Ctrl Pts',(-0.156342837828316,0.0575541228739415,
0.124011319110561));
#29864=CARTESIAN_POINT('',(-0.166599923034401,0.00015352495594109,0.147169404797459));
#29865=CARTESIAN_POINT('Ctrl Pts',(-0.156342827686701,0.0575541504231135,
0.143092354725971));
#29866=CARTESIAN_POINT('Ctrl Pts',(-0.157207830902492,0.0552044146052684,
0.143250068585474));
#29867=CARTESIAN_POINT('Ctrl Pts',(-0.158020096597853,0.0528345395338793,
0.143409565583159));
#29868=CARTESIAN_POINT('Ctrl Pts',(-0.159414773378702,0.0484448168207871,
0.143707332104699));
#29869=CARTESIAN_POINT('Ctrl Pts',(-0.160012730606153,0.0464316190751424,
0.143844777283244));
#29870=CARTESIAN_POINT('Ctrl Pts',(-0.160967856923629,0.0429780132186727,
0.144082919624032));
#29871=CARTESIAN_POINT('Ctrl Pts',(-0.161344110448094,0.0415432095565857,
0.144182575146344));
#29872=CARTESIAN_POINT('Ctrl Pts',(-0.162172013564278,0.0382050250841271,
0.144416214233127));
#29873=CARTESIAN_POINT('Ctrl Pts',(-0.162609358618676,0.0362985059418777,
0.144550908200014));
#29874=CARTESIAN_POINT('Ctrl Pts',(-0.163513054328321,0.0320142298178966,
0.144855733414944));
#29875=CARTESIAN_POINT('Ctrl Pts',(-0.163961297132591,0.0296331167687854,
0.145026611900388));
#29876=CARTESIAN_POINT('Ctrl Pts',(-0.165841657288797,0.0182889637884391,
0.14584514452929));
#29877=CARTESIAN_POINT('Ctrl Pts',(-0.16659156282375,0.00922899163928618,
0.146510942918575));
#29878=CARTESIAN_POINT('Ctrl Pts',(-0.166599929207376,0.000153584169586965,
0.147169411303433));
#29879=CARTESIAN_POINT('Ctrl Pts',(-0.16659992926123,0.000153525741263837,
0.147169415542714));
#29880=CARTESIAN_POINT('Ctrl Pts',(-0.166605625680848,-0.00602799859208348,
0.147617917514895));
#29881=CARTESIAN_POINT('Ctrl Pts',(-0.166267281624384,-0.0122056333318352,
0.148062450528948));
#29882=CARTESIAN_POINT('Ctrl Pts',(-0.165189874066178,-0.0219275111866966,
0.148751907981414));
#29883=CARTESIAN_POINT('Ctrl Pts',(-0.164677680629216,-0.0254906855498114,
0.149002485427659));
#29884=CARTESIAN_POINT('Ctrl Pts',(-0.163531726110651,-0.0319654991952331,
0.149453920762822));
#29885=CARTESIAN_POINT('Ctrl Pts',(-0.162934544150922,-0.0348820139747416,
0.149655804269974));
#29886=CARTESIAN_POINT('Ctrl Pts',(-0.161671516362904,-0.0403063684151372,
0.15002890081508));
#29887=CARTESIAN_POINT('Ctrl Pts',(-0.161024634906989,-0.0428176456555105,
0.150200662167841));
#29888=CARTESIAN_POINT('Ctrl Pts',(-0.159397633237737,-0.0485740578146641,
0.150592686419893));
#29889=CARTESIAN_POINT('Ctrl Pts',(-0.158376565343913,-0.0518064736815498,
0.150811550875058));
#29890=CARTESIAN_POINT('Ctrl Pts',(-0.153584009957701,-0.0655080661938805,
0.151737213874922));
#29891=CARTESIAN_POINT('Ctrl Pts',(-0.148867624185716,-0.075616222069114,
0.152412634347927));
#29892=CARTESIAN_POINT('Ctrl Pts',(-0.138793270197616,-0.0925502350409985,
0.153616654347345));
#29893=CARTESIAN_POINT('Ctrl Pts',(-0.133846100035282,-0.0995705983922593,
0.154142436139106));
#29894=CARTESIAN_POINT('Ctrl Pts',(-0.12705548513444,-0.107781221067798,
0.154831617195679));
#29895=CARTESIAN_POINT('Ctrl Pts',(-0.125699785833086,-0.109359273690093,
0.154967836722193));
#29896=CARTESIAN_POINT('Ctrl Pts',(-0.123327943956184,-0.112017750412008,
0.155204698726309));
#29897=CARTESIAN_POINT('Ctrl Pts',(-0.122326312244992,-0.113110702994342,
0.155304337001842));
#29898=CARTESIAN_POINT('Ctrl Pts',(-0.119982086112629,-0.115601096559505,
0.155536751218561));
#29899=CARTESIAN_POINT('Ctrl Pts',(-0.11862954728311,-0.116988649747368,
0.155670204503956));
#29900=CARTESIAN_POINT('Ctrl Pts',(-0.113409381584476,-0.122160340888496,
0.156181801333983));
#29901=CARTESIAN_POINT('Ctrl Pts',(-0.109382668231441,-0.125778606018597,
0.156569330727374));
#29902=CARTESIAN_POINT('Ctrl Pts',(-0.0984496870463127,-0.1346800334709,
0.157589571267426));
#29903=CARTESIAN_POINT('Ctrl Pts',(-0.091292688907217,-0.139630610861674,
0.158226416037452));
#29904=CARTESIAN_POINT('Ctrl Pts',(-0.0778142376804457,-0.147472632573918,
0.159347635218781));
#29905=CARTESIAN_POINT('Ctrl Pts',(-0.0716356169777629,-0.150570889720812,
0.1598356122158));
#29906=CARTESIAN_POINT('Ctrl Pts',(-0.0624679655483101,-0.154475457779061,
0.160521188375843));
#29907=CARTESIAN_POINT('Ctrl Pts',(-0.0596215337375366,-0.15559623597791,
0.160729034718313));
#29908=CARTESIAN_POINT('Ctrl Pts',(-0.0543169627543738,-0.157517936771051,
0.161107589070845));
#29909=CARTESIAN_POINT('Ctrl Pts',(-0.0518679964467142,-0.158341229852286,
0.161278997943488));
#29910=CARTESIAN_POINT('Ctrl Pts',(-0.046281499610808,-0.160075764855271,
0.161662988426492));
#29911=CARTESIAN_POINT('Ctrl Pts',(-0.0431342859016978,-0.160952363852486,
0.161874386212139));
#29912=CARTESIAN_POINT('Ctrl Pts',(-0.0277784785747813,-0.164746613536699,
0.162885549921719));
#29913=CARTESIAN_POINT('Ctrl Pts',(-0.0152926835334805,-0.166370828963469,
0.163642668815421));
#29914=CARTESIAN_POINT('Ctrl Pts',(0.00478243539284979,-0.166701298274293,
0.164872228546539));
#29915=CARTESIAN_POINT('Ctrl Pts',(0.0123059306299837,-0.166315161011472,
0.165336848226466));
#29916=CARTESIAN_POINT('Ctrl Pts',(0.0218201068601663,-0.165177717960094,
0.165957002913224));
#29917=CARTESIAN_POINT('Ctrl Pts',(0.0238587848729861,-0.164895582018341,
0.166091833794408));
#29918=CARTESIAN_POINT('Ctrl Pts',(0.0273555759523047,-0.164345455543821,
0.166327265812509));
#29919=CARTESIAN_POINT('Ctrl Pts',(0.0288162367433764,-0.164095644057096,
0.166426905294689));
#29920=CARTESIAN_POINT('Ctrl Pts',(0.0321976072447013,-0.163470801685953,
0.166660664573319));
#29921=CARTESIAN_POINT('Ctrl Pts',(0.0341152699392348,-0.163081379671758,
0.16679549736432));
#29922=CARTESIAN_POINT('Ctrl Pts',(0.0409666040260846,-0.161563948038689,
0.167284307121912));
#29923=CARTESIAN_POINT('Ctrl Pts',(0.0458548389375537,-0.160245113937415,
0.167646260047763));
#29924=CARTESIAN_POINT('Ctrl Pts',(0.0604420331525334,-0.155587407094808,
0.168753089634216));
#29925=CARTESIAN_POINT('Ctrl Pts',(0.0699011321755486,-0.151573534196052,
0.169506030037643));
#29926=CARTESIAN_POINT('Ctrl Pts',(0.0842070112049225,-0.143877130440362,
0.170666934228259));
#29927=CARTESIAN_POINT('Ctrl Pts',(0.0893263019083245,-0.140756086154151,
0.171087778486058));
#29928=CARTESIAN_POINT('Ctrl Pts',(0.0967031956664319,-0.135693710774486,
0.17170165775218));
#29929=CARTESIAN_POINT('Ctrl Pts',(0.0990947615182789,-0.133957162504324,
0.171901977417331));
#29930=CARTESIAN_POINT('Ctrl Pts',(0.103498732515959,-0.130576851982278,
0.172273717423411));
#29931=CARTESIAN_POINT('Ctrl Pts',(0.105521308121374,-0.128947883778591,
0.172445644891415));
#29932=CARTESIAN_POINT('Ctrl Pts',(0.11017071750791,-0.125020592131762,
0.172844305624989));
#29933=CARTESIAN_POINT('Ctrl Pts',(0.112765098637182,-0.12268565847008,
0.17306945035868));
#29934=CARTESIAN_POINT('Ctrl Pts',(0.123075693176806,-0.112802541486161,
0.173979158633384));
#29935=CARTESIAN_POINT('Ctrl Pts',(0.130123044235029,-0.104594737947926,
0.17463494929481));
#29936=CARTESIAN_POINT('Ctrl Pts',(0.141356126293413,-0.0886033014285764,
0.175828828586252));
#29937=CARTESIAN_POINT('Ctrl Pts',(0.145812588780287,-0.081060171487749,
0.176364561517838));
#29938=CARTESIAN_POINT('Ctrl Pts',(0.150570586755112,-0.0713329723810846,
0.177064943667778));
#29939=CARTESIAN_POINT('Ctrl Pts',(0.151450196708202,-0.0694458885927025,
0.177201262316261));
#29940=CARTESIAN_POINT('Ctrl Pts',(0.152895273924036,-0.06618756354419,
0.177438227684291));
#29941=CARTESIAN_POINT('Ctrl Pts',(0.153478190168795,-0.0648244022885793,
0.177537867185466));
#29942=CARTESIAN_POINT('Ctrl Pts',(0.154780367724299,-0.0616631758267649,
0.177770191323627));
#29943=CARTESIAN_POINT('Ctrl Pts',(0.155486564542927,-0.0598601443253176,
0.177903550859198));
#29944=CARTESIAN_POINT('Ctrl Pts',(0.157901813076877,-0.0533623258749696,
0.178386164144234));
#29945=CARTESIAN_POINT('Ctrl Pts',(0.159430806045108,-0.0486038016221794,
0.178743240805891));
#29946=CARTESIAN_POINT('Ctrl Pts',(0.163460338477686,-0.033810320831613,
0.179850976722343));
#29947=CARTESIAN_POINT('Ctrl Pts',(0.165243092525473,-0.0236043297934682,
0.1806103537174));
#29948=CARTESIAN_POINT('Ctrl Pts',(0.16654824663301,-0.00730631698408415,
0.181778976521868));
#29949=CARTESIAN_POINT('Ctrl Pts',(0.166703470502951,-0.00129166154309381,
0.182201354869788));
#29950=CARTESIAN_POINT('Ctrl Pts',(0.166449387102815,0.00767517422182518,
0.182816897532829));
#29951=CARTESIAN_POINT('Ctrl Pts',(0.166286907649266,0.0106288788954641,
0.183017409057976));
#29952=CARTESIAN_POINT('Ctrl Pts',(0.165834303711017,0.0161642520348871,
0.183389313121233));
#29953=CARTESIAN_POINT('Ctrl Pts',(0.165562287343944,0.0187464565362648,
0.183561217882721));
#29954=CARTESIAN_POINT('Ctrl Pts',(0.164784095153417,0.0247770569001441,
0.183959542241661));
#29955=CARTESIAN_POINT('Ctrl Pts',(0.164229849752982,0.0282180760389901,
0.184184382318598));
#29956=CARTESIAN_POINT('Ctrl Pts',(0.161506393703004,0.0422976901310394,
0.18509788626771));
#29957=CARTESIAN_POINT('Ctrl Pts',(0.158407925923691,0.0527291680819541,
0.185757342828778));
#29958=CARTESIAN_POINT('Ctrl Pts',(0.15114705282707,0.0705751146936732,
0.186934433089028));
#29959=CARTESIAN_POINT('Ctrl Pts',(0.147392953926587,0.0781125058201587,
0.18744956604288));
#29960=CARTESIAN_POINT('Ctrl Pts',(0.14195214390841,0.0872356244517537,
0.188134281604874));
#29961=CARTESIAN_POINT('Ctrl Pts',(0.14077996132329,0.0891149068743666,
0.188278863129681));
#29962=CARTESIAN_POINT('Ctrl Pts',(0.138756245700188,0.0922197878926013,
0.188524708693242));
#29963=CARTESIAN_POINT('Ctrl Pts',(0.137925103827489,0.0934582821002332,
0.188624713028148));
#29964=CARTESIAN_POINT('Ctrl Pts',(0.136012709746073,0.0962268781693752,
0.188852890118991));
#29965=CARTESIAN_POINT('Ctrl Pts',(0.134922168309857,0.097750074197185,
0.18898161376892));
#29966=CARTESIAN_POINT('Ctrl Pts',(0.131217578079425,0.102744280326106,
0.189413514952243));
#29967=CARTESIAN_POINT('Ctrl Pts',(0.128493592515529,0.106131192994354,
0.189722542481169));
#29968=CARTESIAN_POINT('Ctrl Pts',(0.118428227559485,0.117689989594474,
0.190825445750196));
#29969=CARTESIAN_POINT('Ctrl Pts',(0.110414401223879,0.12523922081087,0.191633994785601));
#29970=CARTESIAN_POINT('Ctrl Pts',(0.0968345030863189,0.135707847528305,
0.192860912450915));
#29971=CARTESIAN_POINT('Ctrl Pts',(0.0917481224649588,0.139197121646909,
0.193294370168409));
#29972=CARTESIAN_POINT('Ctrl Pts',(0.0839356871501263,0.143941717437132,
0.193921893403291));
#29973=CARTESIAN_POINT('Ctrl Pts',(0.081350812955834,0.145418241016336,
0.194123764838301));
#29974=CARTESIAN_POINT('Ctrl Pts',(0.076442563281422,0.148050049664259,
0.194496850916425));
#29975=CARTESIAN_POINT('Ctrl Pts',(0.0741291190797553,0.149221840491351,
0.194668613555299));
#29976=CARTESIAN_POINT('Ctrl Pts',(0.0686756394787373,0.151825955937863,
0.195064660712538));
#29977=CARTESIAN_POINT('Ctrl Pts',(0.065516534993131,0.15321569999824,0.195287427000071));
#29978=CARTESIAN_POINT('Ctrl Pts',(0.0518930867986485,0.158710382295016,
0.196223762158694));
#29979=CARTESIAN_POINT('Ctrl Pts',(0.041071043084029,0.161848924712238,
0.196905393699765));
#29980=CARTESIAN_POINT('Ctrl Pts',(0.0243820682081625,0.164905624061368,
0.197942400090388));
#29981=CARTESIAN_POINT('Ctrl Pts',(0.0187003777396083,0.165646123699925,
0.198293591720041));
#29982=CARTESIAN_POINT('Ctrl Pts',(0.0104175768276488,0.166294027087593,
0.198816331882399));
#29983=CARTESIAN_POINT('Ctrl Pts',(0.00783873437374219,0.166435519523091,
0.198980607756016));
#29984=CARTESIAN_POINT('Ctrl Pts',(0.00313794493456894,0.166583947379469,
0.199284490054942));
#29985=CARTESIAN_POINT('Ctrl Pts',(0.00101714039397208,0.166610391570087,
0.199423231885452));
#29986=CARTESIAN_POINT('Ctrl Pts',(-0.00258791625656352,0.166586513227281,
0.19966274225901));
#29987=CARTESIAN_POINT('Ctrl Pts',(-0.00407198749604368,0.16655684403106,
0.199762429514658));
#29988=CARTESIAN_POINT('Ctrl Pts',(-0.00746008985252719,0.166443799556119,
0.199992638799527));
#29989=CARTESIAN_POINT('Ctrl Pts',(-0.00936330456397102,0.166347585073477,
0.200123777833097));
#29990=CARTESIAN_POINT('Ctrl Pts',(-0.016070824833594,0.165893028742002,
0.200591427416699));
#29991=CARTESIAN_POINT('Ctrl Pts',(-0.0208605101823373,0.165359001067689,
0.200935241265144));
#29992=CARTESIAN_POINT('Ctrl Pts',(-0.0360211930504809,0.162999514396192,
0.202042537545302));
#29993=CARTESIAN_POINT('Ctrl Pts',(-0.0462465694391194,0.16039840035885,
0.202816338009499));
#29994=CARTESIAN_POINT('Ctrl Pts',(-0.0618612298308068,0.154807762288508,
0.204002175665906));
#29995=CARTESIAN_POINT('Ctrl Pts',(-0.0674492542301364,0.152456118863135,
0.204427919311286));
#29996=CARTESIAN_POINT('Ctrl Pts',(-0.0755618554496771,0.148508406481849,
0.205047107824646));
#29997=CARTESIAN_POINT('Ctrl Pts',(-0.0781914418032904,0.147140888914951,
0.205248037889767));
#29998=CARTESIAN_POINT('Ctrl Pts',(-0.0830528163131384,0.144445573515816,
0.205620303382369));
#29999=CARTESIAN_POINT('Ctrl Pts',(-0.0852927224837764,0.143134366202129,
0.205792162078511));
#30000=CARTESIAN_POINT('Ctrl Pts',(-0.090457155303148,0.1399468801662,0.206189770569471));
#30001=CARTESIAN_POINT('Ctrl Pts',(-0.0933554888902937,0.138030365087695,
0.206413960107696));
#30002=CARTESIAN_POINT('Ctrl Pts',(-0.105159994529664,0.129682616066465,
0.207335117468991));
#30003=CARTESIAN_POINT('Ctrl Pts',(-0.113479061074266,0.122469321394276,
0.20800198532963));
#30004=CARTESIAN_POINT('Ctrl Pts',(-0.126878605028953,0.108304467259712,
0.209193402839564));
#30005=CARTESIAN_POINT('Ctrl Pts',(-0.1322457630047,0.101681178473,0.209715235239889));
#30006=CARTESIAN_POINT('Ctrl Pts',(-0.138286966326421,0.0929341981984925,
0.210402129554638));
#30007=CARTESIAN_POINT('Ctrl Pts',(-0.139457747041079,0.0911678999101304,
0.21054075441043));
#30008=CARTESIAN_POINT('Ctrl Pts',(-0.141390814187281,0.0881271867654087,
0.210780140544676));
#30009=CARTESIAN_POINT('Ctrl Pts',(-0.142170300227297,0.0868640822841078,
0.210879824105563));
#30010=CARTESIAN_POINT('Ctrl Pts',(-0.143912574579825,0.0839545568065187,
0.211110128948597));
#30011=CARTESIAN_POINT('Ctrl Pts',(-0.144864087232386,0.0823018355832543,
0.211241369910425));
#30012=CARTESIAN_POINT('Ctrl Pts',(-0.148123220865612,0.0764092385242126,
0.211709798941993));
#30013=CARTESIAN_POINT('Ctrl Pts',(-0.150274591475002,0.0720860536809101,
0.212054318696934));
#30014=CARTESIAN_POINT('Ctrl Pts',(-0.153715123657116,0.0643466838147546,
0.212665597669531));
#30015=CARTESIAN_POINT('Ctrl Pts',(-0.155085027347194,0.0609708987775182,
0.212930493239721));
#30016=CARTESIAN_POINT('Ctrl Pts',(-0.156342826453536,0.0575541537729419,
0.213195533534746));
#30017=CARTESIAN_POINT('Origin',(0.,0.,0.2));
#30018=CARTESIAN_POINT('',(-0.156342830333322,0.0575541432337077,0.283376736141222));
#30019=CARTESIAN_POINT('',(-0.156300294001537,0.0575377421133558,0.263912142181176));
#30020=CARTESIAN_POINT('',(-0.156342830367367,0.0575541431412265,0.2));
#30021=CARTESIAN_POINT('',(-0.166650872726138,-0.000148155484504217,0.197851963660979));
#30022=CARTESIAN_POINT('Ctrl Pts',(-0.15630029400153,0.0575377421133763,
0.263912142181174));
#30023=CARTESIAN_POINT('Ctrl Pts',(-0.141758267767125,0.0958745908958741,
0.261171457150951));
#30024=CARTESIAN_POINT('Ctrl Pts',(-0.0744350248633557,0.17443115827656,
0.254725118684631));
#30025=CARTESIAN_POINT('Ctrl Pts',(0.0976303930414628,0.171027438849501,
0.244573126782223));
#30026=CARTESIAN_POINT('Ctrl Pts',(0.196642115264692,0.0106749753152867,
0.233456166473938));
#30027=CARTESIAN_POINT('Ctrl Pts',(0.115571003264758,-0.159453494582782,
0.222339206165656));
#30028=CARTESIAN_POINT('Ctrl Pts',(-0.0713388377936634,-0.183556113035458,
0.211222245857374));
#30029=CARTESIAN_POINT('Ctrl Pts',(-0.160605486403313,-0.0778296844639771,
0.203059831689148));
#30030=CARTESIAN_POINT('Ctrl Pts',(-0.166754308078833,-0.0113680704511269,
0.198603070957016));
#30031=CARTESIAN_POINT('Ctrl Pts',(-0.166650872726138,-0.000148155484504217,
0.197851963660979));
#30032=CARTESIAN_POINT('Ctrl Pts',(-0.166599936070599,-0.000145949553695321,
0.197881206782592));
#30033=CARTESIAN_POINT('Ctrl Pts',(-0.166607880412107,0.00892243574673455,
0.197221034893899));
#30034=CARTESIAN_POINT('Ctrl Pts',(-0.165875392816583,0.0179775326027426,
0.196562455001654));
#30035=CARTESIAN_POINT('Ctrl Pts',(-0.163808322359624,0.0305976080986405,
0.19566088627383));
#30036=CARTESIAN_POINT('Ctrl Pts',(-0.163084763984722,0.034245342762625,
0.195402084438451));
#30037=CARTESIAN_POINT('Ctrl Pts',(-0.161569670616894,0.0407368625285207,
0.194944761351184));
#30038=CARTESIAN_POINT('Ctrl Pts',(-0.160823524757165,0.0435895199993533,
0.194744929991676));
#30039=CARTESIAN_POINT('Ctrl Pts',(-0.159279286931285,0.0489121318494712,
0.194373860417207));
#30040=CARTESIAN_POINT('Ctrl Pts',(-0.15849844211326,0.051386117030454,
0.194202122394274));
#30041=CARTESIAN_POINT('Ctrl Pts',(-0.157235648286962,0.0550838988379044,
0.193946182973806));
#30042=CARTESIAN_POINT('Ctrl Pts',(-0.156796525399903,0.0563217042233158,
0.193860636377096));
#30043=CARTESIAN_POINT('Ctrl Pts',(-0.156342830468371,0.0575541428668533,
0.193775546749386));
#30044=CARTESIAN_POINT('Ctrl Pts',(-0.156342826453536,0.0575541537729419,
0.213195533534746));
#30045=CARTESIAN_POINT('Ctrl Pts',(-0.158013874670123,0.0530148393326334,
0.213547652653047));
#30046=CARTESIAN_POINT('Ctrl Pts',(-0.159487053569706,0.0484032252857811,
0.213899981616352));
#30047=CARTESIAN_POINT('Ctrl Pts',(-0.162125560420288,0.038704199699571,
0.214625286460061));
#30048=CARTESIAN_POINT('Ctrl Pts',(-0.163256833304157,0.0336143850816674,
0.21499722941801));
#30049=CARTESIAN_POINT('Ctrl Pts',(-0.164852919071802,0.0244150085645269,
0.215651935390286));
#30050=CARTESIAN_POINT('Ctrl Pts',(-0.165406951817498,0.0203254273816211,
0.215936934039846));
#30051=CARTESIAN_POINT('Ctrl Pts',(-0.166069685598577,0.0135502970378199,
0.216399412636238));
#30052=CARTESIAN_POINT('Ctrl Pts',(-0.166266287755632,0.0108753867459279,
0.21657955244516));
#30053=CARTESIAN_POINT('Ctrl Pts',(-0.166533323150183,0.00545443404261039,
0.216940061722184));
#30054=CARTESIAN_POINT('Ctrl Pts',(-0.16660060327145,0.00270906783495527,
0.217120277603702));
#30055=CARTESIAN_POINT('Ctrl Pts',(-0.166598992421068,-0.00457385922341503,
0.217592998041431));
#30056=CARTESIAN_POINT('Ctrl Pts',(-0.166412657240988,-0.00910920072422569,
0.217881816963357));
#30057=CARTESIAN_POINT('Ctrl Pts',(-0.165545774120846,-0.0196683698132305,
0.218546558482778));
#30058=CARTESIAN_POINT('Ctrl Pts',(-0.164721301166187,-0.0256738714392414,
0.218918662560577));
#30059=CARTESIAN_POINT('Ctrl Pts',(-0.161406702268013,-0.0428196808940766,
0.219986283957887));
#30060=CARTESIAN_POINT('Ctrl Pts',(-0.158097917259412,-0.0537645505050713,
0.220673286897026));
#30061=CARTESIAN_POINT('Ctrl Pts',(-0.152906470220314,-0.0661768907999307,
0.221544216055461));
#30062=CARTESIAN_POINT('Ctrl Pts',(-0.152079948010202,-0.06805481572343,
0.221678652252109));
#30063=CARTESIAN_POINT('Ctrl Pts',(-0.150597118826183,-0.0712619372852545,
0.221913681311089));
#30064=CARTESIAN_POINT('Ctrl Pts',(-0.149957390744214,-0.0725984604713507,
0.222013324615797));
#30065=CARTESIAN_POINT('Ctrl Pts',(-0.148413218123421,-0.0757170361266824,
0.22224991952157));
#30066=CARTESIAN_POINT('Ctrl Pts',(-0.147494443597159,-0.0774915547013823,
0.222387661425436));
#30067=CARTESIAN_POINT('Ctrl Pts',(-0.143565618903204,-0.0847565765542724,
0.222963290728941));
#30068=CARTESIAN_POINT('Ctrl Pts',(-0.140279357335519,-0.0900913486878508,
0.223413879428073));
#30069=CARTESIAN_POINT('Ctrl Pts',(-0.128588364761337,-0.106873927309439,
0.224898342131217));
#30070=CARTESIAN_POINT('Ctrl Pts',(-0.119018771814515,-0.117437998868827,
0.225935915846639));
#30071=CARTESIAN_POINT('Ctrl Pts',(-0.105780308475964,-0.128749444235293,
0.227138301806463));
#30072=CARTESIAN_POINT('Ctrl Pts',(-0.103276350320605,-0.13076655159761,
0.227357458811051));
#30073=CARTESIAN_POINT('Ctrl Pts',(-0.0986609977515632,-0.134269203962835,
0.227747228535292));
#30074=CARTESIAN_POINT('Ctrl Pts',(-0.0965705438903173,-0.135780495442718,
0.227918820747597));
#30075=CARTESIAN_POINT('Ctrl Pts',(-0.0918536540908315,-0.139026497490396,
0.228295685383191));
#30076=CARTESIAN_POINT('Ctrl Pts',(-0.0892114289958802,-0.140736576083803,
0.228499981788515));
#30077=CARTESIAN_POINT('Ctrl Pts',(-0.0797437088460053,-0.146490336682967,
0.229210601248832));
#30078=CARTESIAN_POINT('Ctrl Pts',(-0.0726792989690239,-0.150120676405412,
0.229702285219482));
#30079=CARTESIAN_POINT('Ctrl Pts',(-0.0547317303879042,-0.15777860177778,
0.230898377705696));
#30080=CARTESIAN_POINT('Ctrl Pts',(-0.0436375106229962,-0.161199745833712,
0.231592576451132));
#30081=CARTESIAN_POINT('Ctrl Pts',(-0.0297796122578413,-0.16393666216094,
0.232496448752344));
#30082=CARTESIAN_POINT('Ctrl Pts',(-0.0272686370472332,-0.164372972897154,
0.232661735832045));
#30083=CARTESIAN_POINT('Ctrl Pts',(-0.0233786147963693,-0.164957328374244,
0.232921501356426));
#30084=CARTESIAN_POINT('Ctrl Pts',(-0.0220059416149619,-0.165146050923071,
0.233013872771803));
#30085=CARTESIAN_POINT('Ctrl Pts',(-0.0189933058995384,-0.165522018194618,
0.233218459816807));
#30086=CARTESIAN_POINT('Ctrl Pts',(-0.0173526398411447,-0.165702050374126,
0.233331055966956));
#30087=CARTESIAN_POINT('Ctrl Pts',(-0.0125195424540853,-0.166159830263259,
0.233665678199766));
#30088=CARTESIAN_POINT('Ctrl Pts',(-0.00932160953375049,-0.1663698668312,
0.233890836701062));
#30089=CARTESIAN_POINT('Ctrl Pts',(-0.00140443826681245,-0.166660891887333,
0.234454470469612));
#30090=CARTESIAN_POINT('Ctrl Pts',(0.00331598940546039,-0.166633804733525,
0.23479591649902));
#30091=CARTESIAN_POINT('Ctrl Pts',(0.0208649802300617,-0.165787116739579,
0.236073030885685));
#30092=CARTESIAN_POINT('Ctrl Pts',(0.033588965269019,-0.16368446200656,
0.237010029590515));
#30093=CARTESIAN_POINT('Ctrl Pts',(0.0492670428176448,-0.159186233397758,
0.238141742873034));
#30094=CARTESIAN_POINT('Ctrl Pts',(0.0525579972065923,-0.158130194544769,
0.238378300126216));
#30095=CARTESIAN_POINT('Ctrl Pts',(0.0582573777544368,-0.156103693397571,
0.238786559998225));
#30096=CARTESIAN_POINT('Ctrl Pts',(0.0606802988456382,-0.155177923028128,
0.238959665357378));
#30097=CARTESIAN_POINT('Ctrl Pts',(0.0658328096441823,-0.15307005784718,
0.239327244447322));
#30098=CARTESIAN_POINT('Ctrl Pts',(0.0685543753168823,-0.151870671619624,
0.239521062377182));
#30099=CARTESIAN_POINT('Ctrl Pts',(0.0767932179601608,-0.147973196098629,
0.240108208915414));
#30100=CARTESIAN_POINT('Ctrl Pts',(0.0821948403294156,-0.145042355729224,
0.24049355083225));
#30101=CARTESIAN_POINT('Ctrl Pts',(0.0966868869790263,-0.13610893657387,
0.241546475088437));
#30102=CARTESIAN_POINT('Ctrl Pts',(0.105368654715595,-0.129504536304905,
0.242198459367192));
#30103=CARTESIAN_POINT('Ctrl Pts',(0.116641470576333,-0.119040200006501,
0.243156359183624));
#30104=CARTESIAN_POINT('Ctrl Pts',(0.119813224956166,-0.115847251693067,
0.243440807111423));
#30105=CARTESIAN_POINT('Ctrl Pts',(0.124111378507851,-0.111154866251031,
0.243855035324084));
#30106=CARTESIAN_POINT('Ctrl Pts',(0.12534790373456,-0.109758556971357,
0.24397785581041));
#30107=CARTESIAN_POINT('Ctrl Pts',(0.1275315454847,-0.107207713437634,0.244202082635381));
#30108=CARTESIAN_POINT('Ctrl Pts',(0.12848702674732,-0.1060607006107,0.244302903427742));
#30109=CARTESIAN_POINT('Ctrl Pts',(0.130829816153224,-0.103170166138626,
0.244556842789446));
#30110=CARTESIAN_POINT('Ctrl Pts',(0.132197745273909,-0.101411433694743,
0.244711176785054));
#30111=CARTESIAN_POINT('Ctrl Pts',(0.13820263159745,-0.0933630064398376,
0.24541474726208));
#30112=CARTESIAN_POINT('Ctrl Pts',(0.142428556144468,-0.0867796302816796,
0.245982514097691));
#30113=CARTESIAN_POINT('Ctrl Pts',(0.151740976762294,-0.0697478753508089,
0.247395582125085));
#30114=CARTESIAN_POINT('Ctrl Pts',(0.15622826059357,-0.0590161254118924,
0.248236279954064));
#30115=CARTESIAN_POINT('Ctrl Pts',(0.160535351934762,-0.0446695033769497,
0.249274798940772));
#30116=CARTESIAN_POINT('Ctrl Pts',(0.161407845562433,-0.0414062075949876,
0.249505875430124));
#30117=CARTESIAN_POINT('Ctrl Pts',(0.162773567102417,-0.0355955395346767,
0.249908653138473));
#30118=CARTESIAN_POINT('Ctrl Pts',(0.163307616172096,-0.03305904395857,
0.250081610968232));
#30119=CARTESIAN_POINT('Ctrl Pts',(0.164328665052132,-0.0275780773856131,
0.25044965963089));
#30120=CARTESIAN_POINT('Ctrl Pts',(0.164796184198639,-0.0246308757122054,
0.250644075487269));
#30121=CARTESIAN_POINT('Ctrl Pts',(0.165993843992824,-0.0155025241209201,
0.251237010003819));
#30122=CARTESIAN_POINT('Ctrl Pts',(0.166457088974391,-0.00929161102473129,
0.251627280334064));
#30123=CARTESIAN_POINT('Ctrl Pts',(0.166779117532808,0.00818780566235569,
0.252707938403439));
#30124=CARTESIAN_POINT('Ctrl Pts',(0.165844937298942,0.0194356889517013,
0.253381472223035));
#30125=CARTESIAN_POINT('Ctrl Pts',(0.163043528075442,0.0344777653773826,
0.254337796592959));
#30126=CARTESIAN_POINT('Ctrl Pts',(0.162158837769444,0.0384241358473211,
0.254594292560082));
#30127=CARTESIAN_POINT('Ctrl Pts',(0.160661109801641,0.0441247747326446,
0.25497814543172));
#30128=CARTESIAN_POINT('Ctrl Pts',(0.160160847174491,0.0459074092844677,
0.255100118369454));
#30129=CARTESIAN_POINT('Ctrl Pts',(0.159207132046795,0.0491003320412027,
0.255322712968891));
#30130=CARTESIAN_POINT('Ctrl Pts',(0.158764399894478,0.0505135444543569,
0.255422754763808));
#30131=CARTESIAN_POINT('Ctrl Pts',(0.157605638394064,0.0540465396610759,
0.255676554163721));
#30132=CARTESIAN_POINT('Ctrl Pts',(0.156865662545228,0.0561580659159468,
0.255831563477038));
#30133=CARTESIAN_POINT('Ctrl Pts',(0.153178878261691,0.0660363029233616,
0.256570458931958));
#30134=CARTESIAN_POINT('Ctrl Pts',(0.149696567311978,0.0735899274956155,
0.257175312946058));
#30135=CARTESIAN_POINT('Ctrl Pts',(0.140364180784835,0.0904035553586888,
0.258575268428833));
#30136=CARTESIAN_POINT('Ctrl Pts',(0.134134987637219,0.0994121738869732,
0.259365596016227));
#30137=CARTESIAN_POINT('Ctrl Pts',(0.124817794720238,0.110400087299701,
0.26036561864635));
#30138=CARTESIAN_POINT('Ctrl Pts',(0.122485317503679,0.112982349496397,
0.260603872147409));
#30139=CARTESIAN_POINT('Ctrl Pts',(0.118274309102531,0.117360488550731,
0.261013981091134));
#30140=CARTESIAN_POINT('Ctrl Pts',(0.116431536645231,0.119188904907139,
0.261187280952365));
#30141=CARTESIAN_POINT('Ctrl Pts',(0.112396982712582,0.123009116952367,
0.261554248403444));
#30142=CARTESIAN_POINT('Ctrl Pts',(0.1101932896409,0.124987060576263,0.26174728517579));
#30143=CARTESIAN_POINT('Ctrl Pts',(0.103340215161879,0.130815867692492,
0.262327066442521));
#30144=CARTESIAN_POINT('Ctrl Pts',(0.0985330994265482,0.134473903847019,
0.262706149922257));
#30145=CARTESIAN_POINT('Ctrl Pts',(0.0849012835348428,0.143722834163063,
0.263725736413042));
#30146=CARTESIAN_POINT('Ctrl Pts',(0.0757338543323991,0.148757697181544,
0.264352065201648));
#30147=CARTESIAN_POINT('Ctrl Pts',(0.0616537990455089,0.154849711343599,
0.265303739042205));
#30148=CARTESIAN_POINT('Ctrl Pts',(0.0570681958412173,0.156597688776115,
0.265612497220262));
#30149=CARTESIAN_POINT('Ctrl Pts',(0.0505907987241755,0.1587444951795,0.266055660652341));
#30150=CARTESIAN_POINT('Ctrl Pts',(0.0487587682294856,0.159316745399522,
0.266181768875695));
#30151=CARTESIAN_POINT('Ctrl Pts',(0.0454937171895573,0.160275023181045,
0.266408550901073));
#30152=CARTESIAN_POINT('Ctrl Pts',(0.0440647293426925,0.160673770269329,
0.266508529087392));
#30153=CARTESIAN_POINT('Ctrl Pts',(0.0405971498252868,0.161591633666692,
0.266752861409693));
#30154=CARTESIAN_POINT('Ctrl Pts',(0.0385538054137087,0.162091294240902,
0.266898201692077));
#30155=CARTESIAN_POINT('Ctrl Pts',(0.0340107123621782,0.163111462585334,
0.267223543929586));
#30156=CARTESIAN_POINT('Ctrl Pts',(0.0315073503017247,0.163613456809074,
0.2674042705655));
#30157=CARTESIAN_POINT('Ctrl Pts',(0.0234756848323748,0.165032876738857,
0.267986802157955));
#30158=CARTESIAN_POINT('Ctrl Pts',(0.0179123408133515,0.165728997658714,
0.268394239156344));
#30159=CARTESIAN_POINT('Ctrl Pts',(0.000864808309352493,0.166993610074473,
0.269638653064323));
#30160=CARTESIAN_POINT('Ctrl Pts',(-0.0106542005062909,0.166655878373019,
0.27047132454534));
#30161=CARTESIAN_POINT('Ctrl Pts',(-0.0254064044734264,0.164686229793299,
0.271503396493623));
#30162=CARTESIAN_POINT('Ctrl Pts',(-0.0287505045182122,0.16413546561642,
0.271735282997761));
#30163=CARTESIAN_POINT('Ctrl Pts',(-0.0346200707000522,0.162983844976806,
0.2721389586499));
#30164=CARTESIAN_POINT('Ctrl Pts',(-0.0371525529631806,0.162425281696877,
0.272312023398853));
#30165=CARTESIAN_POINT('Ctrl Pts',(-0.042562617500353,0.161098873626916,
0.272679793213341));
#30166=CARTESIAN_POINT('Ctrl Pts',(-0.0454347579348769,0.160312532598328,
0.272873835642583));
#30167=CARTESIAN_POINT('Ctrl Pts',(-0.0541896176281827,0.157661390847867,
0.273463067168614));
#30168=CARTESIAN_POINT('Ctrl Pts',(-0.059991267237877,0.155546418960814,
0.273850176825087));
#30169=CARTESIAN_POINT('Ctrl Pts',(-0.0757855077521142,0.148773094610652,
0.274912853909615));
#30170=CARTESIAN_POINT('Ctrl Pts',(-0.0854522666934945,0.143439068563106,
0.275572390129796));
#30171=CARTESIAN_POINT('Ctrl Pts',(-0.0980605983259332,0.134752177815339,
0.276527108451761));
#30172=CARTESIAN_POINT('Ctrl Pts',(-0.101503674562533,0.132178016396924,
0.276799109988353));
#30173=CARTESIAN_POINT('Ctrl Pts',(-0.106301138027923,0.128293210937801,
0.277200808394139));
#30174=CARTESIAN_POINT('Ctrl Pts',(-0.107739063164974,0.127088053758241,
0.277324316788668));
#30175=CARTESIAN_POINT('Ctrl Pts',(-0.110282749976672,0.124881938610211,
0.277549103028597));
#30176=CARTESIAN_POINT('Ctrl Pts',(-0.111395946549046,0.12388997531534,
0.27764977294472));
#30177=CARTESIAN_POINT('Ctrl Pts',(-0.114125744409702,0.121390932981677,
0.277902295753151));
#30178=CARTESIAN_POINT('Ctrl Pts',(-0.115725881895297,0.119866438990252,
0.278055331244349));
#30179=CARTESIAN_POINT('Ctrl Pts',(-0.119237531832613,0.116384932094863,
0.278401669841419));
#30180=CARTESIAN_POINT('Ctrl Pts',(-0.121132118404769,0.114411754894627,
0.278595843742501));
#30181=CARTESIAN_POINT('Ctrl Pts',(-0.127293002899583,0.107670690581312,
0.279249867545239));
#30182=CARTESIAN_POINT('Ctrl Pts',(-0.131333102519906,0.102703927847197,
0.27971656943918));
#30183=CARTESIAN_POINT('Ctrl Pts',(-0.140944517137165,0.0893905509998384,
0.280911528153118));
#30184=CARTESIAN_POINT('Ctrl Pts',(-0.146066969095307,0.0807497519062215,
0.281634542467625));
#30185=CARTESIAN_POINT('Ctrl Pts',(-0.15190184730056,0.0685117655169172,
0.282576563831391));
#30186=CARTESIAN_POINT('Ctrl Pts',(-0.153320142551815,0.0652761089841767,
0.282818652891452));
#30187=CARTESIAN_POINT('Ctrl Pts',(-0.155225145752001,0.0605246431545676,
0.283164473075707));
#30188=CARTESIAN_POINT('Ctrl Pts',(-0.155794613410234,0.0590433459318386,
0.283270958807161));
#30189=CARTESIAN_POINT('Ctrl Pts',(-0.156342830333322,0.0575541432337077,
0.283376736141222));
#30190=CARTESIAN_POINT('Origin',(0.,0.,0.2));
#30191=CARTESIAN_POINT('',(-0.156342830367367,0.0575541431412265,0.353210893432962));
#30192=CARTESIAN_POINT('',(-0.156342830367367,0.0575541431412265,0.333924682624943));
#30193=CARTESIAN_POINT('',(-0.156342830367367,0.0575541431412265,0.2));
#30194=CARTESIAN_POINT('',(-0.166599956210055,0.000120792416194074,0.357148036344185));
#30195=CARTESIAN_POINT('Ctrl Pts',(-0.156342830367367,0.0575541431412265,
0.353210893432962));
#30196=CARTESIAN_POINT('Ctrl Pts',(-0.160082006381044,0.0473968663699324,
0.353934713614529));
#30197=CARTESIAN_POINT('Ctrl Pts',(-0.162818877487097,0.0368967108312444,
0.354658533796095));
#30198=CARTESIAN_POINT('Ctrl Pts',(-0.164515705202674,0.0262705679738153,
0.355382353977662));
#30199=CARTESIAN_POINT('Ctrl Pts',(-0.164632766007151,0.025537491291983,
0.355432288907398));
#30200=CARTESIAN_POINT('Ctrl Pts',(-0.164744897368182,0.0248038169003774,
0.355482223837133));
#30201=CARTESIAN_POINT('Ctrl Pts',(-0.164852096008479,0.0240696165655247,
0.355532158766869));
#30202=CARTESIAN_POINT('Ctrl Pts',(-0.166008400019439,0.0161501243995043,
0.356070784624253));
#30203=CARTESIAN_POINT('Ctrl Pts',(-0.166594137580341,0.0081459886045818,
0.356609410481637));
#30204=CARTESIAN_POINT('Ctrl Pts',(-0.166599956209999,0.000120792493141786,
0.357148036339021));
#30205=CARTESIAN_POINT('',(0.126907087985239,0.107935865304851,0.4));
#30206=CARTESIAN_POINT('Ctrl Pts',(-0.166599956210055,0.000120792416193977,
0.357148036344186));
#30207=CARTESIAN_POINT('Ctrl Pts',(-0.166607675272906,-0.0105255343436155,
0.357862584225541));
#30208=CARTESIAN_POINT('Ctrl Pts',(-0.165590579468026,-0.0212103033299873,
0.358577132106897));
#30209=CARTESIAN_POINT('Ctrl Pts',(-0.163552894278081,-0.0317176728853632,
0.359291679988253));
#30210=CARTESIAN_POINT('Ctrl Pts',(-0.161517022408263,-0.0422156920146834,
0.360005591999033));
#30211=CARTESIAN_POINT('Ctrl Pts',(-0.158462463953501,-0.0525356940943089,
0.360719504009813));
#30212=CARTESIAN_POINT('Ctrl Pts',(-0.154445125677035,-0.0624680970944765,
0.361433416020594));
#30213=CARTESIAN_POINT('Ctrl Pts',(-0.150429916732076,-0.0723952355694296,
0.362146949632734));
#30214=CARTESIAN_POINT('Ctrl Pts',(-0.145453298561471,-0.0819343154859597,
0.362860483244875));
#30215=CARTESIAN_POINT('Ctrl Pts',(-0.13961945659845,-0.0908953647836543,
0.363574016857016));
#30216=CARTESIAN_POINT('Ctrl Pts',(-0.133772930661803,-0.099875897247618,
0.364289101838147));
#30217=CARTESIAN_POINT('Ctrl Pts',(-0.127066019493771,-0.108275133680505,
0.365004186819279));
#30218=CARTESIAN_POINT('Ctrl Pts',(-0.119645261781961,-0.115933478051536,
0.36571927180041));
#30219=CARTESIAN_POINT('Ctrl Pts',(-0.11642878098275,-0.119252939295227,
0.36602922089199));
#30220=CARTESIAN_POINT('Ctrl Pts',(-0.113078664409795,-0.122433674563659,
0.366339169983571));
#30221=CARTESIAN_POINT('Ctrl Pts',(-0.109608799634176,-0.125465019199596,
0.366649119075151));
#30222=CARTESIAN_POINT('Ctrl Pts',(-0.101483921909479,-0.132563078086924,
0.367374881787193));
#30223=CARTESIAN_POINT('Ctrl Pts',(-0.0926376574341541,-0.138894029613974,
0.368100644499235));
#30224=CARTESIAN_POINT('Ctrl Pts',(-0.0832388006807538,-0.144315148412181,
0.368826407211277));
#30225=CARTESIAN_POINT('Ctrl Pts',(-0.0735911687511109,-0.149879756979392,
0.36957137989229));
#30226=CARTESIAN_POINT('Ctrl Pts',(-0.0633619535574521,-0.154484921721223,
0.370316352573303));
#30227=CARTESIAN_POINT('Ctrl Pts',(-0.0527670590063455,-0.158022775206047,
0.371061325254316));
#30228=CARTESIAN_POINT('Ctrl Pts',(-0.0424682753811155,-0.16146175115453,
0.37178547710042));
#30229=CARTESIAN_POINT('Ctrl Pts',(-0.0318249391874584,-0.163892136062298,
0.372509628946524));
#30230=CARTESIAN_POINT('Ctrl Pts',(-0.0210538606503979,-0.165264318446886,
0.373233780792628));
#30231=CARTESIAN_POINT('Ctrl Pts',(-0.0098182465689913,-0.16669568037313,
0.373989163891096));
#30232=CARTESIAN_POINT('Ctrl Pts',(0.00155535427931255,-0.166975096912089,
0.374744546989564));
#30233=CARTESIAN_POINT('Ctrl Pts',(0.0128153468683916,-0.166106372197585,
0.375499930088031));
#30234=CARTESIAN_POINT('Ctrl Pts',(0.0240753394574707,-0.165237647483082,
0.376255313186499));
#30235=CARTESIAN_POINT('Ctrl Pts',(0.0352206347865155,-0.163221015343348,
0.377010696284967));
#30236=CARTESIAN_POINT('Ctrl Pts',(0.0460104551749553,-0.160120573364554,
0.377766079383434));
#30237=CARTESIAN_POINT('Ctrl Pts',(0.0562505702150188,-0.157178088559903,
0.378482978233383));
#30238=CARTESIAN_POINT('Ctrl Pts',(0.0662497085449184,-0.153236917219443,
0.379199877083332));
#30239=CARTESIAN_POINT('Ctrl Pts',(0.0757999579594132,-0.148357427766025,
0.379916775933281));
#30240=CARTESIAN_POINT('Ctrl Pts',(0.085753716337752,-0.143271774300759,
0.380663964579818));
#30241=CARTESIAN_POINT('Ctrl Pts',(0.0952186826030546,-0.13716680807782,
0.381411153226354));
#30242=CARTESIAN_POINT('Ctrl Pts',(0.103980953453111,-0.130167282060363,
0.38215834187289));
#30243=CARTESIAN_POINT('Ctrl Pts',(0.112369982262007,-0.123465911329659,
0.382873702900726));
#30244=CARTESIAN_POINT('Ctrl Pts',(0.120114332795534,-0.115945468949997,
0.383589063928562));
#30245=CARTESIAN_POINT('Ctrl Pts',(0.127057953112165,-0.10775823194052,
0.384304424956398));
#30246=CARTESIAN_POINT('Ctrl Pts',(0.134002789498536,-0.099569561060709,
0.385019911268864));
#30247=CARTESIAN_POINT('Ctrl Pts',(0.140146049725854,-0.0907146042217684,
0.385735397581329));
#30248=CARTESIAN_POINT('Ctrl Pts',(0.145372698665044,-0.0813777517681734,
0.386450883893795));
#30249=CARTESIAN_POINT('Ctrl Pts',(0.150613002558104,-0.0720165061917496,
0.387168239459907));
#30250=CARTESIAN_POINT('Ctrl Pts',(0.154931550656227,-0.0621717109485352,
0.38788559502602));
#30251=CARTESIAN_POINT('Ctrl Pts',(0.1582606550982,-0.0520492559782427,
0.388602950592133));
#30252=CARTESIAN_POINT('Ctrl Pts',(0.158693934357758,-0.0507318296640838,
0.388696313625327));
#30253=CARTESIAN_POINT('Ctrl Pts',(0.159110524094924,-0.0494097169799387,
0.388789676658522));
#30254=CARTESIAN_POINT('Ctrl Pts',(0.159510338674996,-0.0480833844044693,
0.388883039691717));
#30255=CARTESIAN_POINT('Ctrl Pts',(0.162700330881156,-0.0375010024969307,
0.389627953366905));
#30256=CARTESIAN_POINT('Ctrl Pts',(0.164842651460865,-0.0265681615428049,
0.390372867042094));
#30257=CARTESIAN_POINT('Ctrl Pts',(0.165876691278507,-0.0155075236738458,
0.391117780717282));
#30258=CARTESIAN_POINT('Ctrl Pts',(0.166908350772131,-0.00447234701201396,
0.391860979626866));
#30259=CARTESIAN_POINT('Ctrl Pts',(0.166836640415639,0.00668921134358856,
0.39260417853645));
#30260=CARTESIAN_POINT('Ctrl Pts',(0.165652190126399,0.017745757417684,
0.393347377446034));
#30261=CARTESIAN_POINT('Ctrl Pts',(0.164469606478383,0.0287848788646129,
0.394089405107036));
#30262=CARTESIAN_POINT('Ctrl Pts',(0.162177817279617,0.0397184708520597,
0.394831432768038));
#30263=CARTESIAN_POINT('Ctrl Pts',(0.158819395386297,0.0503185815492748,
0.395573460429041));
#30264=CARTESIAN_POINT('Ctrl Pts',(0.155458738367561,0.0609257469220445,
0.396315981930584));
#30265=CARTESIAN_POINT('Ctrl Pts',(0.15103026034291,0.0711981668756874,
0.397058503432127));
#30266=CARTESIAN_POINT('Ctrl Pts',(0.145626686853412,0.0809223583201725,
0.39780102493367));
#30267=CARTESIAN_POINT('Ctrl Pts',(0.140292464949716,0.0905217456699905,
0.398534016622447));
#30268=CARTESIAN_POINT('Ctrl Pts',(0.134008531813893,0.0995862444050702,
0.399267008311223));
#30269=CARTESIAN_POINT('Ctrl Pts',(0.126907087985239,0.10793586530485,0.4));
#30270=CARTESIAN_POINT('',(-0.126912151695562,0.107929911294333,0.399999950528882));
#30271=CARTESIAN_POINT('Origin',(0.,0.,0.4));
#30272=CARTESIAN_POINT('',(-0.166599974196028,9.27247699980398E-5,0.337851963656908));
#30273=CARTESIAN_POINT('Ctrl Pts',(-0.126912151695562,0.107929911294333,
0.399999950528882));
#30274=CARTESIAN_POINT('Ctrl Pts',(-0.119947535241094,0.116119434007461,
0.399276600529823));
#30275=CARTESIAN_POINT('Ctrl Pts',(-0.112160840526412,0.123662698151552,
0.398553250530764));
#30276=CARTESIAN_POINT('Ctrl Pts',(-0.103696444166919,0.130394046900681,
0.397829900531706));
#30277=CARTESIAN_POINT('Ctrl Pts',(-0.0951773525351325,0.137168892307706,
0.397101876386555));
#30278=CARTESIAN_POINT('Ctrl Pts',(-0.085972380799809,0.14312057361781,
0.396373852241404));
#30279=CARTESIAN_POINT('Ctrl Pts',(-0.0762661277144263,0.148118323523617,
0.395645828096254));
#30280=CARTESIAN_POINT('Ctrl Pts',(-0.0666443076806357,0.153072598849487,
0.394924136909832));
#30281=CARTESIAN_POINT('Ctrl Pts',(-0.0565307295261072,0.157089069983039,
0.394202445723411));
#30282=CARTESIAN_POINT('Ctrl Pts',(-0.0461308220115868,0.160085937110464,
0.39348075453699));
#30283=CARTESIAN_POINT('Ctrl Pts',(-0.0355940231514617,0.163122251239998,
0.392749563912475));
#30284=CARTESIAN_POINT('Ctrl Pts',(-0.0247642098773763,0.165111604793141,
0.39201837328796));
#30285=CARTESIAN_POINT('Ctrl Pts',(-0.0138683517813452,0.166021772123023,
0.391287182663444));
#30286=CARTESIAN_POINT('Ctrl Pts',(-0.00297249368531417,0.166931939452904,
0.390555992038929));
#30287=CARTESIAN_POINT('Ctrl Pts',(0.007988440041223,0.166762970969527,
0.389824801414414));
#30288=CARTESIAN_POINT('Ctrl Pts',(0.0187884890345102,0.165537164044211,
0.389093610789898));
#30289=CARTESIAN_POINT('Ctrl Pts',(0.0295122497374452,0.164320015849489,
0.388367585075533));
#30290=CARTESIAN_POINT('Ctrl Pts',(0.0401551997329114,0.162052204061964,
0.387641559361168));
#30291=CARTESIAN_POINT('Ctrl Pts',(0.0504980366376883,0.158762427216702,
0.386915533646802));
#30292=CARTESIAN_POINT('Ctrl Pts',(0.0611098520847941,0.155387095567805,
0.38617062671637));
#30293=CARTESIAN_POINT('Ctrl Pts',(0.0714047096220906,0.150935892100486,
0.385425719785938));
#30294=CARTESIAN_POINT('Ctrl Pts',(0.0811576670828012,0.145495680601443,
0.384680812855506));
#30295=CARTESIAN_POINT('Ctrl Pts',(0.0906427759753403,0.140204875358548,
0.383956363540678));
#30296=CARTESIAN_POINT('Ctrl Pts',(0.0996146075556019,0.133979282411873,
0.38323191422585));
#30297=CARTESIAN_POINT('Ctrl Pts',(0.107890355537113,0.126945780481572,
0.382507464911022));
#30298=CARTESIAN_POINT('Ctrl Pts',(0.116516649928662,0.119614351541268,
0.381752329172788));
#30299=CARTESIAN_POINT('Ctrl Pts',(0.124385600621863,0.111405537080788,
0.380997193434553));
#30300=CARTESIAN_POINT('Ctrl Pts',(0.131330797395314,0.102507471218009,
0.380242057696319));
#30301=CARTESIAN_POINT('Ctrl Pts',(0.138275994168766,0.0936094053552298,
0.379486921958085));
#30302=CARTESIAN_POINT('Ctrl Pts',(0.144296878889521,0.0840230462814757,
0.37873178621985));
#30303=CARTESIAN_POINT('Ctrl Pts',(0.149278728771727,0.0739690552616248,
0.377976650481616));
#30304=CARTESIAN_POINT('Ctrl Pts',(0.154053604917181,0.0643327629159306,
0.377252887279526));
#30305=CARTESIAN_POINT('Ctrl Pts',(0.157909601642383,0.0541957456425725,
0.376529124077436));
#30306=CARTESIAN_POINT('Ctrl Pts',(0.160751247714667,0.0437561008109459,
0.375805360875347));
#30307=CARTESIAN_POINT('Ctrl Pts',(0.163678129271707,0.0330033176907131,
0.375059888316845));
#30308=CARTESIAN_POINT('Ctrl Pts',(0.165528232910599,0.0219303145823395,
0.374314415758344));
#30309=CARTESIAN_POINT('Ctrl Pts',(0.166251225055711,0.0107745147211016,
0.373568943199843));
#30310=CARTESIAN_POINT('Ctrl Pts',(0.166951509711302,-3.09076012234098E-5,
0.372846884187984));
#30311=CARTESIAN_POINT('Ctrl Pts',(0.166594543597082,-0.0109130254897179,
0.372124825176124));
#30312=CARTESIAN_POINT('Ctrl Pts',(0.165187201660095,-0.0216505983221526,
0.371402766164264));
#30313=CARTESIAN_POINT('Ctrl Pts',(0.163711407839935,-0.0329104373230026,
0.370645586832442));
#30314=CARTESIAN_POINT('Ctrl Pts',(0.161080294950841,-0.0440101868140574,
0.36988840750062));
#30315=CARTESIAN_POINT('Ctrl Pts',(0.15736244965134,-0.0547048392715816,
0.369131228168798));
#30316=CARTESIAN_POINT('Ctrl Pts',(0.153644604351838,-0.0653994917291058,
0.368374048836976));
#30317=CARTESIAN_POINT('Ctrl Pts',(0.148840548557795,-0.0756880211301988,
0.367616869505155));
#30318=CARTESIAN_POINT('Ctrl Pts',(0.143075557820479,-0.0853518878195371,
0.366859690173333));
#30319=CARTESIAN_POINT('Ctrl Pts',(0.137555879679565,-0.0946045364624177,
0.366134730429762));
#30320=CARTESIAN_POINT('Ctrl Pts',(0.131114667484915,-0.103353509144416,
0.365409770686192));
#30321=CARTESIAN_POINT('Ctrl Pts',(0.12386750309171,-0.111410958517667,
0.364684810942622));
#30322=CARTESIAN_POINT('Ctrl Pts',(0.116418269742169,-0.119693069606485,
0.363939637519491));
#30323=CARTESIAN_POINT('Ctrl Pts',(0.108117869668668,-0.127243570141914,
0.36319446409636));
#30324=CARTESIAN_POINT('Ctrl Pts',(0.0991382592325092,-0.13389236556409,
0.362449290673229));
#30325=CARTESIAN_POINT('Ctrl Pts',(0.0904222880731206,-0.140345953896943,
0.361725995368724));
#30326=CARTESIAN_POINT('Ctrl Pts',(0.0810673064246538,-0.145949611427857,
0.36100270006422));
#30327=CARTESIAN_POINT('Ctrl Pts',(0.0712635883715059,-0.15058904665485,
0.360279404759715));
#30328=CARTESIAN_POINT('Ctrl Pts',(0.0610150584167484,-0.155438981204093,
0.359523292277271));
#30329=CARTESIAN_POINT('Ctrl Pts',(0.0502769557916214,-0.159234397099614,
0.358767179794827));
#30330=CARTESIAN_POINT('Ctrl Pts',(0.0392907384715136,-0.161900580203911,
0.358011067312383));
#30331=CARTESIAN_POINT('Ctrl Pts',(0.0283045211514057,-0.164566763308208,
0.357254954829938));
#30332=CARTESIAN_POINT('Ctrl Pts',(0.0170713121684996,-0.166103596998203,
0.356498842347494));
#30333=CARTESIAN_POINT('Ctrl Pts',(0.00584102204421006,-0.166497574941736,
0.35574272986505));
#30334=CARTESIAN_POINT('Ctrl Pts',(-0.0049256806434658,-0.166875289438564,
0.355017829777267));
#30335=CARTESIAN_POINT('Ctrl Pts',(-0.0157686683437115,-0.166205706831982,
0.354292929689485));
#30336=CARTESIAN_POINT('Ctrl Pts',(-0.0264674582994453,-0.164484144072209,
0.353568029601703));
#30337=CARTESIAN_POINT('Ctrl Pts',(-0.0374656822343477,-0.162714398817996,
0.352822841264625));
#30338=CARTESIAN_POINT('Ctrl Pts',(-0.0483105010955349,-0.159832727950378,
0.352077652927547));
#30339=CARTESIAN_POINT('Ctrl Pts',(-0.0587657332681133,-0.155891464145607,
0.351332464590469));
#30340=CARTESIAN_POINT('Ctrl Pts',(-0.0689131274043697,-0.15206624471845,
0.350609217163988));
#30341=CARTESIAN_POINT('Ctrl Pts',(-0.0786927167223967,-0.147243454704251,
0.349885969737508));
#30342=CARTESIAN_POINT('Ctrl Pts',(-0.0879053564862984,-0.141521052501092,
0.349162722311028));
#30343=CARTESIAN_POINT('Ctrl Pts',(-0.0975372173176259,-0.135538252450918,
0.348406563518651));
#30344=CARTESIAN_POINT('Ctrl Pts',(-0.106548233235344,-0.128572340363373,
0.347650404726274));
#30345=CARTESIAN_POINT('Ctrl Pts',(-0.114744722882249,-0.12078579622901,
0.346894245933897));
#30346=CARTESIAN_POINT('Ctrl Pts',(-0.122941212529154,-0.112999252094647,
0.34613808714152));
#30347=CARTESIAN_POINT('Ctrl Pts',(-0.130322469069809,-0.104392957478539,
0.345381928349144));
#30348=CARTESIAN_POINT('Ctrl Pts',(-0.136741702362345,-0.0951696739252992,
0.344625769556767));
#30349=CARTESIAN_POINT('Ctrl Pts',(-0.14296702617097,-0.0862250034201091,
0.343892452489329));
#30350=CARTESIAN_POINT('Ctrl Pts',(-0.148333340221089,-0.0766351629444054,
0.34315913542189));
#30351=CARTESIAN_POINT('Ctrl Pts',(-0.15271467922135,-0.0665866859839123,
0.342425818354452));
#30352=CARTESIAN_POINT('Ctrl Pts',(-0.157269236597204,-0.0561409375828448,
0.341663509238873));
#30353=CARTESIAN_POINT('Ctrl Pts',(-0.160758522692059,-0.0452002413067621,
0.340901200123295));
#30354=CARTESIAN_POINT('Ctrl Pts',(-0.163092875949299,-0.0340040264466811,
0.340138891007716));
#30355=CARTESIAN_POINT('Ctrl Pts',(-0.165427229206539,-0.0228078115866,
0.339376581892137));
#30356=CARTESIAN_POINT('Ctrl Pts',(-0.166606346848609,-0.011357122512868,
0.338614272776558));
#30357=CARTESIAN_POINT('Ctrl Pts',(-0.166599974196062,9.27247088470251E-5,
0.337851963660979));
#30358=CARTESIAN_POINT('Ctrl Pts',(-0.166599974196028,9.27247699982471E-5,
0.337851963656908));
#30359=CARTESIAN_POINT('Ctrl Pts',(-0.166593228454842,0.0122128983487723,
0.337045025483611));
#30360=CARTESIAN_POINT('Ctrl Pts',(-0.165259685224493,0.0242846265757986,
0.336238087310314));
#30361=CARTESIAN_POINT('Ctrl Pts',(-0.162655324506395,0.0360389429606284,
0.335431149137018));
#30362=CARTESIAN_POINT('Ctrl Pts',(-0.161034637677667,0.0433536231480551,
0.334928993632993));
#30363=CARTESIAN_POINT('Ctrl Pts',(-0.158922840566651,0.0505456798939685,
0.334426838128968));
#30364=CARTESIAN_POINT('Ctrl Pts',(-0.156342830367367,0.0575541431412263,
0.333924682624943));
#30365=CARTESIAN_POINT('Origin',(0.,0.,0.2));
#30366=CARTESIAN_POINT('',(-0.166599975890259,8.9629041933745E-5,0.267851966777163));
#30367=CARTESIAN_POINT('Ctrl Pts',(-0.156342830367367,0.0575541431412263,
0.333924682624943));
#30368=CARTESIAN_POINT('Ctrl Pts',(-0.155630595781153,0.0594888912760559,
0.333786058166124));
#30369=CARTESIAN_POINT('Ctrl Pts',(-0.154882719734524,0.0614096680351601,
0.333647433707304));
#30370=CARTESIAN_POINT('Ctrl Pts',(-0.154099774838887,0.0633152382496057,
0.333508809248485));
#30371=CARTESIAN_POINT('Ctrl Pts',(-0.150006198854086,0.0732783870109964,
0.332784020366546));
#30372=CARTESIAN_POINT('Ctrl Pts',(-0.144927306279316,0.0828795908971444,
0.332059231484606));
#30373=CARTESIAN_POINT('Ctrl Pts',(-0.1389496178186,0.0919160688240363,
0.331334442602667));
#30374=CARTESIAN_POINT('Ctrl Pts',(-0.132803455780128,0.10120722843544,
0.330589226464128));
#30375=CARTESIAN_POINT('Ctrl Pts',(-0.125707325343765,0.109900349908042,
0.329844010325589));
#30376=CARTESIAN_POINT('Ctrl Pts',(-0.117806257442659,0.117801722005045,
0.329098794187051));
#30377=CARTESIAN_POINT('Ctrl Pts',(-0.11013940500608,0.125468869620085,
0.328375668878036));
#30378=CARTESIAN_POINT('Ctrl Pts',(-0.101715466852179,0.132389988772537,
0.327652543569021));
#30379=CARTESIAN_POINT('Ctrl Pts',(-0.092705710586656,0.138424026905098,
0.326929418260006));
#30380=CARTESIAN_POINT('Ctrl Pts',(-0.083283094363323,0.144734566715996,
0.326173156706705));
#30381=CARTESIAN_POINT('Ctrl Pts',(-0.0732204191893915,0.150073934404664,
0.325416895153405));
#30382=CARTESIAN_POINT('Ctrl Pts',(-0.0627457002634819,0.154332553592705,
0.324660633600104));
#30383=CARTESIAN_POINT('Ctrl Pts',(-0.0522709813375724,0.158591172780747,
0.323904372046803));
#30384=CARTESIAN_POINT('Ctrl Pts',(-0.0413853152555228,0.161768762188444,
0.323148110493502));
#30385=CARTESIAN_POINT('Ctrl Pts',(-0.0303341135834924,0.163815144455889,
0.322391848940202));
#30386=CARTESIAN_POINT('Ctrl Pts',(-0.0197431633200151,0.165776300668378,
0.321667083549533));
#30387=CARTESIAN_POINT('Ctrl Pts',(-0.00892221477796013,0.166713339777031,
0.320942318158864));
#30388=CARTESIAN_POINT('Ctrl Pts',(0.00191144223773458,0.166589034418751,
0.320217552768195));
#30389=CARTESIAN_POINT('Ctrl Pts',(0.0130508809796042,0.166461220521575,
0.319472330756839));
#30390=CARTESIAN_POINT('Ctrl Pts',(0.0242027780835187,0.165210915452516,
0.318727108745483));
#30391=CARTESIAN_POINT('Ctrl Pts',(0.0351257177818648,0.16285497827917,
0.317981886734126));
#30392=CARTESIAN_POINT('Ctrl Pts',(0.0457244496428421,0.160568968553657,
0.317258783934569));
#30393=CARTESIAN_POINT('Ctrl Pts',(0.0561067201092357,0.157242405567947,
0.316535681135013));
#30394=CARTESIAN_POINT('Ctrl Pts',(0.0660611681537217,0.152942741122832,
0.315812578335456));
#30395=CARTESIAN_POINT('Ctrl Pts',(0.0764723656633846,0.148445791059573,
0.3150562967182));
#30396=CARTESIAN_POINT('Ctrl Pts',(0.0864144302980466,0.14288445654869,
0.314300015100943));
#30397=CARTESIAN_POINT('Ctrl Pts',(0.0956716550808264,0.136390961629044,
0.313543733483687));
#30398=CARTESIAN_POINT('Ctrl Pts',(0.104928879863606,0.129897466709398,
0.312787451866431));
#30399=CARTESIAN_POINT('Ctrl Pts',(0.11350043373518,0.122472580726663,0.312031170249175));
#30400=CARTESIAN_POINT('Ctrl Pts',(0.12121110516053,0.114295354174013,0.311274888631919));
#30401=CARTESIAN_POINT('Ctrl Pts',(0.128600073795149,0.106459295913629,
0.310550160415583));
#30402=CARTESIAN_POINT('Ctrl Pts',(0.135253270227448,0.097874840020428,
0.309825432199247));
#30403=CARTESIAN_POINT('Ctrl Pts',(0.141021614388083,0.0887043644663494,
0.309100703982911));
#30404=CARTESIAN_POINT('Ctrl Pts',(0.146953149202477,0.0792744494857578,
0.308355472677972));
#30405=CARTESIAN_POINT('Ctrl Pts',(0.151948200500906,0.0692254989172822,
0.307610241373032));
#30406=CARTESIAN_POINT('Ctrl Pts',(0.155890032973563,0.0587695296858969,
0.306865010068092));
#30407=CARTESIAN_POINT('Ctrl Pts',(0.159714609240943,0.0486245902314157,
0.306141946877977));
#30408=CARTESIAN_POINT('Ctrl Pts',(0.162547562502924,0.0380974657469978,
0.305418883687861));
#30409=CARTESIAN_POINT('Ctrl Pts',(0.164330987445657,0.0274023094854309,
0.304695820497745));
#30410=CARTESIAN_POINT('Ctrl Pts',(0.166196428392214,0.0162153052319293,
0.303939505135394));
#30411=CARTESIAN_POINT('Ctrl Pts',(0.166913020611866,0.00484546047150204,
0.303183189773042));
#30412=CARTESIAN_POINT('Ctrl Pts',(0.166474931774067,-0.00645423045915291,
0.30242687441069));
#30413=CARTESIAN_POINT('Ctrl Pts',(0.166036842936267,-0.017753921389808,
0.301670559048339));
#30414=CARTESIAN_POINT('Ctrl Pts',(0.164444269118064,-0.0289823423839235,
0.300914243685987));
#30415=CARTESIAN_POINT('Ctrl Pts',(0.161752704107014,-0.0398951464976462,
0.300157928323636));
#30416=CARTESIAN_POINT('Ctrl Pts',(0.15917345289749,-0.050352580404712,
0.299433172538388));
#30417=CARTESIAN_POINT('Ctrl Pts',(0.155566370516096,-0.0605973979856725,
0.298708416753141));
#30418=CARTESIAN_POINT('Ctrl Pts',(0.150987106295862,-0.0704162888286652,
0.297983660967894));
#30419=CARTESIAN_POINT('Ctrl Pts',(0.146278514024313,-0.0805124857972116,
0.297238436555182));
#30420=CARTESIAN_POINT('Ctrl Pts',(0.140542100949058,-0.090157307397608,
0.29649321214247));
#30421=CARTESIAN_POINT('Ctrl Pts',(0.133892745257038,-0.0991377464315882,
0.295747987729758));
#30422=CARTESIAN_POINT('Ctrl Pts',(0.127440869853345,-0.107851473956683,
0.295024895857207));
#30423=CARTESIAN_POINT('Ctrl Pts',(0.120130224668095,-0.115939054735954,
0.294301803984655));
#30424=CARTESIAN_POINT('Ctrl Pts',(0.112109387908945,-0.123235729975854,
0.293578712112103));
#30425=CARTESIAN_POINT('Ctrl Pts',(0.103720296094471,-0.1308674123509,0.292822421429311));
#30426=CARTESIAN_POINT('Ctrl Pts',(0.0945548357077293,-0.137632876796364,
0.292066130746519));
#30427=CARTESIAN_POINT('Ctrl Pts',(0.084822406851203,-0.143390094832136,
0.291309840063728));
#30428=CARTESIAN_POINT('Ctrl Pts',(0.0750899779946767,-0.149147312867908,
0.290553549380936));
#30429=CARTESIAN_POINT('Ctrl Pts',(0.0647916243622132,-0.153895844390901,
0.289797258698145));
#30430=CARTESIAN_POINT('Ctrl Pts',(0.0541627183865265,-0.157549864922131,
0.289040968015353));
#30431=CARTESIAN_POINT('Ctrl Pts',(0.043977080418474,-0.16105149814234,
0.288316217687224));
#30432=CARTESIAN_POINT('Ctrl Pts',(0.0334129151605437,-0.163574190146975,
0.287591467359096));
#30433=CARTESIAN_POINT('Ctrl Pts',(0.0226796340738417,-0.165049066032731,
0.286866717030967));
#30434=CARTESIAN_POINT('Ctrl Pts',(0.0116431192534093,-0.166565609710283,
0.286121491253976));
#30435=CARTESIAN_POINT('Ctrl Pts',(0.000428707759892578,-0.16697376746695,
0.285376265476985));
#30436=CARTESIAN_POINT('Ctrl Pts',(-0.010722328474245,-0.166254598950196,
0.284631039699993));
#30437=CARTESIAN_POINT('Ctrl Pts',(-0.0215420873547145,-0.165556795644536,
0.28390795324872));
#30438=CARTESIAN_POINT('Ctrl Pts',(-0.0323012345614199,-0.163797936127461,
0.283184866797448));
#30439=CARTESIAN_POINT('Ctrl Pts',(-0.0427807792159435,-0.161013555111601,
0.282461780346175));
#30440=CARTESIAN_POINT('Ctrl Pts',(-0.0537416149776651,-0.158101296610015,
0.281705484906324));
#30441=CARTESIAN_POINT('Ctrl Pts',(-0.0643954292253115,-0.154067050397989,
0.280949189466473));
#30442=CARTESIAN_POINT('Ctrl Pts',(-0.0745093508587406,-0.14900978704303,
0.280192894026623));
#30443=CARTESIAN_POINT('Ctrl Pts',(-0.0846232724921697,-0.143952523688071,
0.279436598586772));
#30444=CARTESIAN_POINT('Ctrl Pts',(-0.0941963658250105,-0.137872881702097,
0.278680303146922));
#30445=CARTESIAN_POINT('Ctrl Pts',(-0.103028911236834,-0.130922127424483,
0.277924007707071));
#30446=CARTESIAN_POINT('Ctrl Pts',(-0.111391142551149,-0.124341485902893,
0.27720798337715));
#30447=CARTESIAN_POINT('Ctrl Pts',(-0.119154706145039,-0.116929141929537,
0.27649195904723));
#30448=CARTESIAN_POINT('Ctrl Pts',(-0.126150360403159,-0.108819329947179,
0.27577593471731));
#30449=CARTESIAN_POINT('Ctrl Pts',(-0.133136026511876,-0.100721096869485,
0.275060932701775));
#30450=CARTESIAN_POINT('Ctrl Pts',(-0.13935527853753,-0.0919280094024027,
0.27434593068624));
#30451=CARTESIAN_POINT('Ctrl Pts',(-0.144675018419886,-0.0826117367279351,
0.273630928670705));
#30452=CARTESIAN_POINT('Ctrl Pts',(-0.149989766192038,-0.0733042065598499,
0.272916597621972));
#30453=CARTESIAN_POINT('Ctrl Pts',(-0.154406198060711,-0.0634752687959111,
0.272202266573239));
#30454=CARTESIAN_POINT('Ctrl Pts',(-0.157835917236709,-0.0533233835202424,
0.271487935524506));
#30455=CARTESIAN_POINT('Ctrl Pts',(-0.161272582613367,-0.0431509376597016,
0.270772157743097));
#30456=CARTESIAN_POINT('Ctrl Pts',(-0.163718267329638,-0.032655136419677,
0.270056379961688));
#30457=CARTESIAN_POINT('Ctrl Pts',(-0.165134329484697,-0.022050243210436,
0.269340602180279));
#30458=CARTESIAN_POINT('Ctrl Pts',(-0.166116012306651,-0.0146984179710137,
0.26884439037924));
#30459=CARTESIAN_POINT('Ctrl Pts',(-0.166603948462927,-0.00729447879190147,
0.268348178578201));
#30460=CARTESIAN_POINT('Ctrl Pts',(-0.166599975890259,8.9629041933745E-5,
0.267851966777163));
#30461=CARTESIAN_POINT('Ctrl Pts',(-0.166813199754551,8.97901853038408E-5,
0.267851963660979));
#30462=CARTESIAN_POINT('Ctrl Pts',(-0.166846982879129,0.00527956240150659,
0.267503658240248));
#30463=CARTESIAN_POINT('Ctrl Pts',(-0.166013000560697,0.0248364214798825,
0.266190384413647));
#30464=CARTESIAN_POINT('Ctrl Pts',(-0.161420399274048,0.0440397124427515,
0.264877110587046));
#30465=CARTESIAN_POINT('Ctrl Pts',(-0.15630029400153,0.0575377421133763,
0.263912142181174));
#30466=CARTESIAN_POINT('',(-0.166599950277464,-0.000128714981079622,0.287148036339021));
#30467=CARTESIAN_POINT('Ctrl Pts',(-0.156342830333322,0.0575541432337077,
0.283376736141222));
#30468=CARTESIAN_POINT('Ctrl Pts',(-0.156693002305398,0.0566029193227644,
0.283444301107039));
#30469=CARTESIAN_POINT('Ctrl Pts',(-0.157034504006096,0.0556484700093607,
0.283511577341258));
#30470=CARTESIAN_POINT('Ctrl Pts',(-0.158330006516994,0.0519207991796621,
0.283772374119022));
#30471=CARTESIAN_POINT('Ctrl Pts',(-0.159219458012203,0.0491256176913406,
0.283963729442103));
#30472=CARTESIAN_POINT('Ctrl Pts',(-0.161652435568176,0.0407175964792538,
0.284528245306058));
#30473=CARTESIAN_POINT('Ctrl Pts',(-0.162976209044119,0.0350456580328451,
0.284894394953798));
#30474=CARTESIAN_POINT('Ctrl Pts',(-0.165738035686808,0.0195951430193326,
0.285867353567811));
#30475=CARTESIAN_POINT('Ctrl Pts',(-0.166607857439204,0.00974010186083236,
0.286461354741719));
#30476=CARTESIAN_POINT('Ctrl Pts',(-0.166599946525299,-0.000133483210403523,
0.287070783175954));
#30477=CARTESIAN_POINT('Ctrl Pts',(-0.166599950277464,-0.000128714981079622,
0.287148036339021));
#30478=CARTESIAN_POINT('Ctrl Pts',(-0.166593491893487,-0.00848800960612518,
0.287708823198405));
#30479=CARTESIAN_POINT('Ctrl Pts',(-0.165957778354428,-0.016823530277876,
0.288269610057788));
#30480=CARTESIAN_POINT('Ctrl Pts',(-0.16470404452251,-0.0250626757934412,
0.288830396917171));
#30481=CARTESIAN_POINT('Ctrl Pts',(-0.163083704256697,-0.0357110438081525,
0.289555164412204));
#30482=CARTESIAN_POINT('Ctrl Pts',(-0.16042046221447,-0.0462408744313591,
0.290279931907237));
#30483=CARTESIAN_POINT('Ctrl Pts',(-0.156750395020604,-0.056434684909944,
0.29100469940227));
#30484=CARTESIAN_POINT('Ctrl Pts',(-0.152976753205844,-0.0669161795098307,
0.291749920887535));
#30485=CARTESIAN_POINT('Ctrl Pts',(-0.148138610264182,-0.0770413696170685,
0.2924951423728));
#30486=CARTESIAN_POINT('Ctrl Pts',(-0.142331049133399,-0.0865877153676312,
0.293240363858066));
#30487=CARTESIAN_POINT('Ctrl Pts',(-0.136695862832195,-0.0958507150311191,
0.293963466346453));
#30488=CARTESIAN_POINT('Ctrl Pts',(-0.130148640486049,-0.104568014997532,
0.294686568834841));
#30489=CARTESIAN_POINT('Ctrl Pts',(-0.122822406993161,-0.112562055508978,
0.295409671323228));
#30490=CARTESIAN_POINT('Ctrl Pts',(-0.115160020039955,-0.120922890824665,
0.296165952306933));
#30491=CARTESIAN_POINT('Ctrl Pts',(-0.106645932747233,-0.128491508136188,
0.296922233290638));
#30492=CARTESIAN_POINT('Ctrl Pts',(-0.0974757874352491,-0.135107478933914,
0.297678514274342));
#30493=CARTESIAN_POINT('Ctrl Pts',(-0.0883056421232658,-0.141723449731641,
0.298434795258047));
#30494=CARTESIAN_POINT('Ctrl Pts',(-0.0784804380772645,-0.147386241101972,
0.299191076241752));
#30495=CARTESIAN_POINT('Ctrl Pts',(-0.068226779208863,-0.151989034468889,
0.299947357225456));
#30496=CARTESIAN_POINT('Ctrl Pts',(-0.0584000960596539,-0.156400161521043,
0.300672145683315));
#30497=CARTESIAN_POINT('Ctrl Pts',(-0.0481076509769673,-0.159870587002123,
0.301396934141173));
#30498=CARTESIAN_POINT('Ctrl Pts',(-0.0375517721827202,-0.16231273642551,
0.302121722599031));
#30499=CARTESIAN_POINT('Ctrl Pts',(-0.0266983814205212,-0.16482371656353,
0.30286693884359));
#30500=CARTESIAN_POINT('Ctrl Pts',(-0.015567356247688,-0.16624703322788,
0.303612155088149));
#30501=CARTESIAN_POINT('Ctrl Pts',(-0.00439723288282395,-0.166541959706778,
0.304357371332708));
#30502=CARTESIAN_POINT('Ctrl Pts',(0.00644176450877101,-0.166828143415863,
0.305080496464553));
#30503=CARTESIAN_POINT('Ctrl Pts',(0.0173166088560319,-0.166052040928164,
0.305803621596399));
#30504=CARTESIAN_POINT('Ctrl Pts',(0.0280059699158458,-0.164229186349664,
0.306526746728244));
#30505=CARTESIAN_POINT('Ctrl Pts',(0.0391851629624217,-0.162322800821581,
0.307283008529159));
#30506=CARTESIAN_POINT('Ctrl Pts',(0.0501603522143856,-0.159271323868591,
0.308039270330075));
#30507=CARTESIAN_POINT('Ctrl Pts',(0.060690698754633,-0.155152180405802,
0.30879553213099));
#30508=CARTESIAN_POINT('Ctrl Pts',(0.0712210452948805,-0.151033036943012,
0.309551793931906));
#30509=CARTESIAN_POINT('Ctrl Pts',(0.0813055599547078,-0.145846777599868,
0.310308055732821));
#30510=CARTESIAN_POINT('Ctrl Pts',(0.0907316620926344,-0.139725894142453,
0.311064317533737));
#30511=CARTESIAN_POINT('Ctrl Pts',(0.0997631054822526,-0.133861284186906,
0.311788915627706));
#30512=CARTESIAN_POINT('Ctrl Pts',(0.108256962643401,-0.127095724813711,
0.312513513721675));
#30513=CARTESIAN_POINT('Ctrl Pts',(0.116030006079989,-0.119551652807804,
0.313238111815644));
#30514=CARTESIAN_POINT('Ctrl Pts',(0.124024738902939,-0.111792421745177,
0.313983375651176));
#30515=CARTESIAN_POINT('Ctrl Pts',(0.131255976641635,-0.103210027724542,
0.314728639486707));
#30516=CARTESIAN_POINT('Ctrl Pts',(0.137560067724559,-0.0939829121043548,
0.315473903322238));
#30517=CARTESIAN_POINT('Ctrl Pts',(0.143675290244099,-0.0850322379328126,
0.316196839290341));
#30518=CARTESIAN_POINT('Ctrl Pts',(0.148917729715307,-0.075475816565885,
0.316919775258443));
#30519=CARTESIAN_POINT('Ctrl Pts',(0.153180499596328,-0.0655079731286148,
0.317642711226546));
#30520=CARTESIAN_POINT('Ctrl Pts',(0.157640752861041,-0.0550783446302099,
0.318399138995792));
#30521=CARTESIAN_POINT('Ctrl Pts',(0.16102766860715,-0.0441991294669704,
0.319155566765038));
#30522=CARTESIAN_POINT('Ctrl Pts',(0.163275721001094,-0.0331149351739208,
0.319911994534283));
#30523=CARTESIAN_POINT('Ctrl Pts',(0.165523773395038,-0.022030740880871,
0.320668422303529));
#30524=CARTESIAN_POINT('Ctrl Pts',(0.166632889218102,-0.01074270054802,
0.321424850072775));
#30525=CARTESIAN_POINT('Ctrl Pts',(0.166599254238088,0.000498485017781699,
0.322181277842021));
#30526=CARTESIAN_POINT('Ctrl Pts',(0.16656702045109,0.011271376245462,0.322906193735632));
#30527=CARTESIAN_POINT('Ctrl Pts',(0.165485420152532,0.0220807733691656,
0.323631109629243));
#30528=CARTESIAN_POINT('Ctrl Pts',(0.163358090325391,0.0327061817588259,
0.324356025522854));
#30529=CARTESIAN_POINT('Ctrl Pts',(0.161171280815181,0.0436286742749966,
0.325101209908475));
#30530=CARTESIAN_POINT('Ctrl Pts',(0.157879249630706,0.0543557147090324,
0.325846394294095));
#30531=CARTESIAN_POINT('Ctrl Pts',(0.15354319742141,0.0646532793105646,
0.326591578679716));
#30532=CARTESIAN_POINT('Ctrl Pts',(0.149334804488175,0.0746476696008179,
0.327314823823232));
#30533=CARTESIAN_POINT('Ctrl Pts',(0.144143535428062,0.0842366995458919,
0.328038068966747));
#30534=CARTESIAN_POINT('Ctrl Pts',(0.138074789796087,0.0932250632757434,
0.328761314110263));
#30535=CARTESIAN_POINT('Ctrl Pts',(0.131729906092074,0.102622412582131,
0.329517468116936));
#30536=CARTESIAN_POINT('Ctrl Pts',(0.124426154296712,0.111362075685159,
0.33027362212361));
#30537=CARTESIAN_POINT('Ctrl Pts',(0.116333209720592,0.119256632168214,
0.331029776130283));
#30538=CARTESIAN_POINT('Ctrl Pts',(0.108240265144473,0.127151188651269,
0.331785930136956));
#30539=CARTESIAN_POINT('Ctrl Pts',(0.0993590351697043,0.134199965056974,
0.33254208414363));
#30540=CARTESIAN_POINT('Ctrl Pts',(0.0898976910402409,0.14026391248512,
0.333298238150303));
#30541=CARTESIAN_POINT('Ctrl Pts',(0.0808267551962532,0.146077640146789,
0.334023190587172));
#30542=CARTESIAN_POINT('Ctrl Pts',(0.0711562522558495,0.151029111540782,
0.334748143024041));
#30543=CARTESIAN_POINT('Ctrl Pts',(0.0610735058921922,0.155001893143395,
0.33547309546091));
#30544=CARTESIAN_POINT('Ctrl Pts',(0.050709497637079,0.159085496939445,
0.336218270710716));
#30545=CARTESIAN_POINT('Ctrl Pts',(0.0399106851694592,0.162134323637613,
0.336963445960522));
#30546=CARTESIAN_POINT('Ctrl Pts',(0.0289069036702446,0.164073004849059,
0.337708621210329));
#30547=CARTESIAN_POINT('Ctrl Pts',(0.0182262189919821,0.165954761835291,
0.338431916367888));
#30548=CARTESIAN_POINT('Ctrl Pts',(0.00735340969149694,0.166790658058575,
0.339155211525448));
#30549=CARTESIAN_POINT('Ctrl Pts',(-0.0034902345256906,0.166563436152583,
0.339878506683008));
#30550=CARTESIAN_POINT('Ctrl Pts',(-0.0148259184032063,0.166325903857648,
0.340634621978938));
#30551=CARTESIAN_POINT('Ctrl Pts',(-0.0261286441049934,0.164926216810827,
0.341390737274867));
#30552=CARTESIAN_POINT('Ctrl Pts',(-0.0371490103249585,0.162405391018513,
0.342146852570797));
#30553=CARTESIAN_POINT('Ctrl Pts',(-0.0481693765449237,0.159884565226199,
0.342902967866727));
#30554=CARTESIAN_POINT('Ctrl Pts',(-0.0589063264950848,0.156242998178431,
0.343659083162657));
#30555=CARTESIAN_POINT('Ctrl Pts',(-0.0691302433640257,0.151580240969694,
0.344415198458586));
#30556=CARTESIAN_POINT('Ctrl Pts',(-0.079041259879042,0.147060186249601,
0.345148173039784));
#30557=CARTESIAN_POINT('Ctrl Pts',(-0.0885447161972927,0.141546778420546,
0.345881147620982));
#30558=CARTESIAN_POINT('Ctrl Pts',(-0.0974340198565392,0.135137603111035,
0.34661412220218));
#30559=CARTESIAN_POINT('Ctrl Pts',(-0.106194196036957,0.12882152853031,
0.347336449474731));
#30560=CARTESIAN_POINT('Ctrl Pts',(-0.114357173296284,0.121636065751674,
0.348058776747282));
#30561=CARTESIAN_POINT('Ctrl Pts',(-0.121751122610046,0.11371993731617,
0.348781104019834));
#30562=CARTESIAN_POINT('Ctrl Pts',(-0.12930855528541,0.105628779916766,
0.349519402255355));
#30563=CARTESIAN_POINT('Ctrl Pts',(-0.136061726017171,0.0967748355308142,
0.350257700490876));
#30564=CARTESIAN_POINT('Ctrl Pts',(-0.141866927035433,0.0873460646710723,
0.350995998726398));
#30565=CARTESIAN_POINT('Ctrl Pts',(-0.147672128053695,0.0779172938113303,
0.351734296961919));
#30566=CARTESIAN_POINT('Ctrl Pts',(-0.152528862308024,0.0679145886067279,
0.352472595197441));
#30567=CARTESIAN_POINT('Ctrl Pts',(-0.156342830367367,0.0575541431412265,
0.353210893432962));
#30568=CARTESIAN_POINT('Origin',(0.,0.,0.554592528053768));
#30569=CARTESIAN_POINT('',(-0.205640730232501,-0.000158877854750081,0.309592528053768));
#30570=CARTESIAN_POINT('Ctrl Pts',(0.125373879670659,0.163134317426071,
0.354786983357521));
#30571=CARTESIAN_POINT('Ctrl Pts',(0.174468778198734,0.124883730283729,
0.351399912090603));
#30572=CARTESIAN_POINT('Ctrl Pts',(0.23971402602582,-0.00512738462875954,
0.344307187387591));
#30573=CARTESIAN_POINT('Ctrl Pts',(0.13227703569284,-0.20370800021477,0.333508809248484));
#30574=CARTESIAN_POINT('Ctrl Pts',(-0.0994668003959092,-0.221581469162487,
0.322391848940201));
#30575=CARTESIAN_POINT('Ctrl Pts',(-0.200331019397092,-0.0888856881277869,
0.314419755208629));
#30576=CARTESIAN_POINT('Ctrl Pts',(-0.205728678103024,-0.0104771510256757,
0.310153314913151));
#30577=CARTESIAN_POINT('Ctrl Pts',(-0.205640730232501,-0.000158877854750081,
0.309592528053768));
#30578=CARTESIAN_POINT('Ctrl Pts',(-0.205640730232501,-0.000158877854750081,
0.309592528053768));
#30579=CARTESIAN_POINT('Ctrl Pts',(-0.205147522672671,0.0577055172922507,
0.306447661477057));
#30580=CARTESIAN_POINT('Ctrl Pts',(-0.149444666487041,0.184584641155565,
0.299597141464252));
#30581=CARTESIAN_POINT('Ctrl Pts',(0.0190813655878192,0.223159202921371,
0.291328296299053));
#30582=CARTESIAN_POINT('Ctrl Pts',(0.104339452755073,0.178824647059424,
0.286204317710565));
#30583=CARTESIAN_POINT('Ctrl Pts',(0.125045885691731,0.162713195961808,
0.284785992558171));
#30584=CARTESIAN_POINT('',(-0.205202343170581,0.000114209666698874,0.315407471946233));
#30585=CARTESIAN_POINT('Ctrl Pts',(-0.205202343170581,0.000114209666698874,
0.315407471946233));
#30586=CARTESIAN_POINT('Ctrl Pts',(-0.205338714105211,0.0268973406518496,
0.313959753808734));
#30587=CARTESIAN_POINT('Ctrl Pts',(-0.188013873562118,0.122066992862534,
0.308806382235141));
#30588=CARTESIAN_POINT('Ctrl Pts',(-0.0538860451750873,0.230976530846397,
0.300542700088359));
#30589=CARTESIAN_POINT('Ctrl Pts',(0.079577912064408,0.197485954337428,
0.293726736079075));
#30590=CARTESIAN_POINT('Ctrl Pts',(0.125296449978256,0.163038483752231,
0.290616425505885));
#30591=CARTESIAN_POINT('Ctrl Pts',(0.125005569899291,0.162656434463559,
0.360610754417505));
#30592=CARTESIAN_POINT('Ctrl Pts',(0.14989460202478,0.14362771524947,0.358917889200626));
#30593=CARTESIAN_POINT('Ctrl Pts',(0.215982794706034,0.0658033246759699,
0.353519370547653));
#30594=CARTESIAN_POINT('Ctrl Pts',(0.208602501412145,-0.124451281241526,
0.344415198458586));
#30595=CARTESIAN_POINT('Ctrl Pts',(0.00851095428263868,-0.242724098340208,
0.333298238150303));
#30596=CARTESIAN_POINT('Ctrl Pts',(-0.172282834993387,-0.152290880723065,
0.323628995979519));
#30597=CARTESIAN_POINT('Ctrl Pts',(-0.204989652081738,-0.0416581321254629,
0.317665407244829));
#30598=CARTESIAN_POINT('Ctrl Pts',(-0.205202343170581,0.000114209666698874,
0.315407471946233));
#30599=CARTESIAN_POINT('Ctrl Pts',(0.126643636228966,0.107786740449723,
0.399832185534737));
#30600=CARTESIAN_POINT('Ctrl Pts',(0.162509204878374,0.0656489274283753,
0.396125257297164));
#30601=CARTESIAN_POINT('Ctrl Pts',(0.188237171307053,-0.0564923230466638,
0.388712675623497));
#30602=CARTESIAN_POINT('Ctrl Pts',(0.0542929026994402,-0.189069324461983,
0.377594440513735));
#30603=CARTESIAN_POINT('Ctrl Pts',(-0.129318690295624,-0.147980389363182,
0.366477480205453));
#30604=CARTESIAN_POINT('Ctrl Pts',(-0.194518592522063,0.0283751522978791,
0.35536051989717));
#30605=CARTESIAN_POINT('Ctrl Pts',(-0.0815717939981551,0.178875911116407,
0.344243559588887));
#30606=CARTESIAN_POINT('Ctrl Pts',(0.106073156940092,0.165495539869897,
0.333126599280604));
#30607=CARTESIAN_POINT('Ctrl Pts',(0.196579733944809,0.000591879416301521,
0.322009638972321));
#30608=CARTESIAN_POINT('Ctrl Pts',(0.107059398326759,-0.164872578396621,
0.310892678664038));
#30609=CARTESIAN_POINT('Ctrl Pts',(-0.0805041914350236,-0.179338602839428,
0.299775718355756));
#30610=CARTESIAN_POINT('Ctrl Pts',(-0.194343207489227,-0.0295733312979194,
0.288658758047472));
#30611=CARTESIAN_POINT('Ctrl Pts',(-0.130204543087865,0.147277588040085,
0.277541797739191));
#30612=CARTESIAN_POINT('Ctrl Pts',(0.0531740072575756,0.189251798966039,
0.266424837430907));
#30613=CARTESIAN_POINT('Ctrl Pts',(0.187856398295355,0.0579119037769601,
0.255307877122625));
#30614=CARTESIAN_POINT('Ctrl Pts',(0.150501811766188,-0.126463503045677,
0.244190916814341));
#30615=CARTESIAN_POINT('Ctrl Pts',(-0.0246807683842457,-0.195024735134491,
0.233073956506059));
#30616=CARTESIAN_POINT('Ctrl Pts',(-0.177260962860889,-0.0849844321598874,
0.221956996197776));
#30617=CARTESIAN_POINT('Ctrl Pts',(-0.167507390899782,0.102883792677308,
0.210840035889493));
#30618=CARTESIAN_POINT('Ctrl Pts',(-0.00435228181763329,0.196532072723541,
0.199723075581211));
#30619=CARTESIAN_POINT('Ctrl Pts',(0.162788607054259,0.110198321346856,
0.188606115272927));
#30620=CARTESIAN_POINT('Ctrl Pts',(0.180849360257203,-0.0770539217729518,
0.177489154964645));
#30621=CARTESIAN_POINT('Ctrl Pts',(0.0332901492326799,-0.193740978540385,
0.166372194656362));
#30622=CARTESIAN_POINT('Ctrl Pts',(-0.144755865067518,-0.133002038301909,
0.155255234348079));
#30623=CARTESIAN_POINT('Ctrl Pts',(-0.190235897869724,0.0495387808087312,
0.144138274039796));
#30624=CARTESIAN_POINT('Ctrl Pts',(-0.0614999585747447,0.186712527814268,
0.133021313731514));
#30625=CARTESIAN_POINT('Ctrl Pts',(0.123557201881564,0.152896804553835,
0.121904353423231));
#30626=CARTESIAN_POINT('Ctrl Pts',(0.195461582000762,-0.0209401151255174,
0.110787393114948));
#30627=CARTESIAN_POINT('Ctrl Pts',(0.0883649656983379,-0.175600523395451,
0.0996704328066651));
#30628=CARTESIAN_POINT('Ctrl Pts',(-0.099656720083647,-0.16944734392556,
0.0885534724983826));
#30629=CARTESIAN_POINT('Ctrl Pts',(-0.19641124121612,-0.00811687322483667,
0.0774365121900994));
#30630=CARTESIAN_POINT('Ctrl Pts',(-0.11329927613454,0.160648547782502,
0.0663195518818169));
#30631=CARTESIAN_POINT('Ctrl Pts',(0.0735803580016403,0.182290627941773,
0.0552025915735339));
#30632=CARTESIAN_POINT('Ctrl Pts',(0.193057988403518,0.0369986682686435,
0.0440856312652511));
#30633=CARTESIAN_POINT('Ctrl Pts',(0.135769225220844,-0.142187434876412,
0.0329686709569682));
#30634=CARTESIAN_POINT('Ctrl Pts',(-0.0459207683190805,-0.191138471118919,
0.0218517106486855));
#30635=CARTESIAN_POINT('Ctrl Pts',(-0.185432287088896,-0.0650875272293826,
0.0107347503404028));
#30636=CARTESIAN_POINT('Ctrl Pts',(-0.155367407483271,0.120647823966984,
-0.000382209967880125));
#30637=CARTESIAN_POINT('Ctrl Pts',(0.0174625308446545,0.195743738997455,
-0.0114991702761629));
#30638=CARTESIAN_POINT('Ctrl Pts',(0.12128809756269,0.126513168479806,-0.0189104771483514));
#30639=CARTESIAN_POINT('Ctrl Pts',(0.147094871950923,0.0775866671285812,
-0.0226161305844457));
#30640=CARTESIAN_POINT('Ctrl Pts',(0.136651966898638,0.116304857682842,
0.407420004843589));
#30641=CARTESIAN_POINT('Ctrl Pts',(0.175351901974875,0.0708369984075165,
0.403713076606016));
#30642=CARTESIAN_POINT('Ctrl Pts',(0.203113085414244,-0.0609567704218693,
0.396300494932349));
#30643=CARTESIAN_POINT('Ctrl Pts',(0.058583535370867,-0.204011001557275,
0.385182259822589));
#30644=CARTESIAN_POINT('Ctrl Pts',(-0.139538423815494,-0.15967491041038,
0.374065299514305));
#30645=CARTESIAN_POINT('Ctrl Pts',(-0.20989091167942,0.030617569804638,
0.362948339206022));
#30646=CARTESIAN_POINT('Ctrl Pts',(-0.0880182094041043,0.193012028181579,
0.35183137889774));
#30647=CARTESIAN_POINT('Ctrl Pts',(0.114455853942829,0.178574239571626,
0.340714418589457));
#30648=CARTESIAN_POINT('Ctrl Pts',(0.212114939967467,0.000638654170180345,
0.329597458281175));
#30649=CARTESIAN_POINT('Ctrl Pts',(0.115520035526191,-0.17790204700704,
0.318480497972891));
#30650=CARTESIAN_POINT('Ctrl Pts',(-0.0868662368734497,-0.193511285277326,
0.307363537664609));
#30651=CARTESIAN_POINT('Ctrl Pts',(-0.209701666404921,-0.0319104379022986,
0.296246577356326));
#30652=CARTESIAN_POINT('Ctrl Pts',(-0.140494283344222,0.158916568451797,
0.285129617048043));
#30653=CARTESIAN_POINT('Ctrl Pts',(0.0573762164132184,0.204207896566219,
0.27401265673976));
#30654=CARTESIAN_POINT('Ctrl Pts',(0.202702220861237,0.0624885370762606,
0.262895696431478));
#30655=CARTESIAN_POINT('Ctrl Pts',(0.162395594536428,-0.1364575982392,0.251778736123194));
#30656=CARTESIAN_POINT('Ctrl Pts',(-0.0266312279456287,-0.21043705347998,
0.240661775814911));
#30657=CARTESIAN_POINT('Ctrl Pts',(-0.191269454593774,-0.0917005398472298,
0.229544815506629));
#30658=CARTESIAN_POINT('Ctrl Pts',(-0.180745082170017,0.111014442177949,
0.218427855198346));
#30659=CARTESIAN_POINT('Ctrl Pts',(-0.00469623179329347,0.21206351219877,
0.207310894890063));
#30660=CARTESIAN_POINT('Ctrl Pts',(0.175653384607776,0.118907019802798,
0.196193934581781));
#30661=CARTESIAN_POINT('Ctrl Pts',(0.195141434085374,-0.0831433010063813,
0.185076974273498));
#30662=CARTESIAN_POINT('Ctrl Pts',(0.035920986687165,-0.209051844804459,
0.173960013965215));
#30663=CARTESIAN_POINT('Ctrl Pts',(-0.156195560002925,-0.143512857626925,
0.162843053656931));
#30664=CARTESIAN_POINT('Ctrl Pts',(-0.205269766351514,0.0534537070858774,
0.151726093348649));
#30665=CARTESIAN_POINT('Ctrl Pts',(-0.0663601468946243,0.201467953149315,
0.140609133040367));
#30666=CARTESIAN_POINT('Ctrl Pts',(0.133321619343601,0.164979857629981,
0.129492172732083));
#30667=CARTESIAN_POINT('Ctrl Pts',(0.210908423264415,-0.0225949601905965,
0.118375212423801));
#30668=CARTESIAN_POINT('Ctrl Pts',(0.0953482285187782,-0.189477794739203,
0.107258252115518));
#30669=CARTESIAN_POINT('Ctrl Pts',(-0.107532342086862,-0.182838344844378,
0.0961412918072349));
#30670=CARTESIAN_POINT('Ctrl Pts',(-0.211933131678721,-0.00875832946896322,
0.0850243314989519));
#30671=CARTESIAN_POINT('Ctrl Pts',(-0.122253035312291,0.173344201789962,
0.0739073711906692));
#30672=CARTESIAN_POINT('Ctrl Pts',(0.0793952301547247,0.196696601559939,
0.0627904108823863));
#30673=CARTESIAN_POINT('Ctrl Pts',(0.208314879660736,0.0399225807319636,
0.0516734505741035));
#30674=CARTESIAN_POINT('Ctrl Pts',(0.146498728425558,-0.153424153180541,
0.0405564902658207));
#30675=CARTESIAN_POINT('Ctrl Pts',(-0.0495497720939863,-0.206243667713202,
0.0294395299575379));
#30676=CARTESIAN_POINT('Ctrl Pts',(-0.200086538192865,-0.0702312321511612,
0.0183225696492552));
#30677=CARTESIAN_POINT('Ctrl Pts',(-0.167645706146228,0.130182320549621,
0.00720560934097224));
#30678=CARTESIAN_POINT('Ctrl Pts',(0.0188425510985476,0.211212878424741,
-0.00391135096731048));
#30679=CARTESIAN_POINT('Ctrl Pts',(0.130873193370489,0.136511188608702,
-0.011322657839499));
#30680=CARTESIAN_POINT('Ctrl Pts',(0.158719412765877,0.0837181478985793,
-0.0150283112755933));
#30681=CARTESIAN_POINT('Ctrl Pts',(0.146660297568308,0.124822974915961,
0.415007824152442));
#30682=CARTESIAN_POINT('Ctrl Pts',(0.188194599071376,0.0760250693866577,
0.411300895914869));
#30683=CARTESIAN_POINT('Ctrl Pts',(0.217988999521435,-0.065421217797075,
0.403888314241202));
#30684=CARTESIAN_POINT('Ctrl Pts',(0.0628741680422935,-0.218952678652567,
0.39277007913144));
#30685=CARTESIAN_POINT('Ctrl Pts',(-0.149758157335363,-0.171369431457579,
0.381653118823158));
#30686=CARTESIAN_POINT('Ctrl Pts',(-0.225263230836776,0.0328599873113971,
0.370536158514874));
#30687=CARTESIAN_POINT('Ctrl Pts',(-0.0944646248100532,0.207148145246751,
0.359419198206592));
#30688=CARTESIAN_POINT('Ctrl Pts',(0.122838550945567,0.191652939273356,
0.348302237898309));
#30689=CARTESIAN_POINT('Ctrl Pts',(0.227650145990125,0.000685428924058993,
0.337185277590026));
#30690=CARTESIAN_POINT('Ctrl Pts',(0.123980672725625,-0.190931515617459,
0.326068317281743));
#30691=CARTESIAN_POINT('Ctrl Pts',(-0.093228282311876,-0.207683967715224,
0.314951356973461));
#30692=CARTESIAN_POINT('Ctrl Pts',(-0.225060125320616,-0.0342475445066776,
0.303834396665177));
#30693=CARTESIAN_POINT('Ctrl Pts',(-0.15078402360058,0.170555548863508,
0.292717436356895));
#30694=CARTESIAN_POINT('Ctrl Pts',(0.0615784255688618,0.219163994166401,
0.281600476048612));
#30695=CARTESIAN_POINT('Ctrl Pts',(0.217548043427119,0.0670651703755612,
0.27048351574033));
#30696=CARTESIAN_POINT('Ctrl Pts',(0.174289377306668,-0.146451693432721,
0.259366555432046));
#30697=CARTESIAN_POINT('Ctrl Pts',(-0.0285816875070117,-0.225849371825467,
0.248249595123764));
#30698=CARTESIAN_POINT('Ctrl Pts',(-0.205277946326661,-0.0984166475345728,
0.237132634815481));
#30699=CARTESIAN_POINT('Ctrl Pts',(-0.193982773440251,0.11914509167859,
0.226015674507198));
#30700=CARTESIAN_POINT('Ctrl Pts',(-0.00504018176895369,0.227594951673999,
0.214898714198915));
#30701=CARTESIAN_POINT('Ctrl Pts',(0.188518162161292,0.127615718258739,
0.203781753890632));
#30702=CARTESIAN_POINT('Ctrl Pts',(0.209433507913547,-0.0892326802398108,
0.19266479358235));
#30703=CARTESIAN_POINT('Ctrl Pts',(0.0385518241416503,-0.224362711068533,
0.181547833274067));
#30704=CARTESIAN_POINT('Ctrl Pts',(-0.167635254938332,-0.154023676951941,
0.170430872965784));
#30705=CARTESIAN_POINT('Ctrl Pts',(-0.220303634833304,0.0573686333630237,
0.159313912657501));
#30706=CARTESIAN_POINT('Ctrl Pts',(-0.0712203352145041,0.216223378484361,
0.148196952349218));
#30707=CARTESIAN_POINT('Ctrl Pts',(0.143086036805638,0.177062910706128,
0.137079992040936));
#30708=CARTESIAN_POINT('Ctrl Pts',(0.226355264528068,-0.0242498052556755,
0.125963031732653));
#30709=CARTESIAN_POINT('Ctrl Pts',(0.102331491339218,-0.203355066082957,
0.11484607142437));
#30710=CARTESIAN_POINT('Ctrl Pts',(-0.115407964090077,-0.196229345763195,
0.103729111116087));
#30711=CARTESIAN_POINT('Ctrl Pts',(-0.227455022141321,-0.00939978571308979,
0.0926121508078043));
#30712=CARTESIAN_POINT('Ctrl Pts',(-0.131206794490042,0.186039855797424,
0.0814951904995215));
#30713=CARTESIAN_POINT('Ctrl Pts',(0.0852101023078094,0.211102575178107,
0.0703782301912387));
#30714=CARTESIAN_POINT('Ctrl Pts',(0.223571770917953,0.0428464931952837,
0.0592612698829559));
#30715=CARTESIAN_POINT('Ctrl Pts',(0.157228231630271,-0.164660871484669,
0.048144309574673));
#30716=CARTESIAN_POINT('Ctrl Pts',(-0.0531787758688922,-0.221348864307486,
0.0370273492663903));
#30717=CARTESIAN_POINT('Ctrl Pts',(-0.214740789296835,-0.0753749370729399,
0.0259103889581075));
#30718=CARTESIAN_POINT('Ctrl Pts',(-0.179924004809185,0.139716817132259,
0.0147934286498247));
#30719=CARTESIAN_POINT('Ctrl Pts',(0.0202225713524407,0.226682017852026,
0.00367646834154192));
#30720=CARTESIAN_POINT('Ctrl Pts',(0.140458289178288,0.146509208737597,
-0.0037348385306466));
#30721=CARTESIAN_POINT('Ctrl Pts',(0.17034395358083,0.0898496286685773,
-0.00744049196674088));
#30722=CARTESIAN_POINT('Ctrl Pts',(0.15666862823798,0.133341092149081,0.422595643461294));
#30723=CARTESIAN_POINT('Ctrl Pts',(0.201037296167877,0.0812131403657989,
0.418888715223721));
#30724=CARTESIAN_POINT('Ctrl Pts',(0.232864913628626,-0.0698856651722803,
0.411476133550053));
#30725=CARTESIAN_POINT('Ctrl Pts',(0.0671648007137202,-0.233894355747859,
0.400357898440292));
#30726=CARTESIAN_POINT('Ctrl Pts',(-0.159977890855233,-0.183063952504777,
0.38924093813201));
#30727=CARTESIAN_POINT('Ctrl Pts',(-0.240635549994133,0.0351024048181559,
0.378123977823728));
#30728=CARTESIAN_POINT('Ctrl Pts',(-0.100911040216002,0.221284262311923,
0.367007017515444));
#30729=CARTESIAN_POINT('Ctrl Pts',(0.131221247948303,0.204731638975084,
0.355890057207162));
#30730=CARTESIAN_POINT('Ctrl Pts',(0.243185352012785,0.000732203677937851,
0.344773096898879));
#30731=CARTESIAN_POINT('Ctrl Pts',(0.132441309925057,-0.203960984227879,
0.333656136590596));
#30732=CARTESIAN_POINT('Ctrl Pts',(-0.0995903277503024,-0.221856650153122,
0.322539176282312));
#30733=CARTESIAN_POINT('Ctrl Pts',(-0.240418584236309,-0.0365846511110568,
0.311422215974029));
#30734=CARTESIAN_POINT('Ctrl Pts',(-0.161073763856939,0.182194529275218,
0.300305255665748));
#30735=CARTESIAN_POINT('Ctrl Pts',(0.0657806347245049,0.234120091766581,
0.289188295357465));
#30736=CARTESIAN_POINT('Ctrl Pts',(0.232393865993,0.0716418036748616,0.278071335049182));
#30737=CARTESIAN_POINT('Ctrl Pts',(0.186183160076907,-0.156445788626244,
0.2669543747409));
#30738=CARTESIAN_POINT('Ctrl Pts',(-0.0305321470683947,-0.241261690170956,
0.255837414432615));
#30739=CARTESIAN_POINT('Ctrl Pts',(-0.219286438059546,-0.105132755221915,
0.244720454124334));
#30740=CARTESIAN_POINT('Ctrl Pts',(-0.207220464710484,0.127275741179231,
0.233603493816051));
#30741=CARTESIAN_POINT('Ctrl Pts',(-0.00538413174461367,0.243126391149227,
0.222486533507768));
#30742=CARTESIAN_POINT('Ctrl Pts',(0.201382939714809,0.136324416714681,
0.211369573199485));
#30743=CARTESIAN_POINT('Ctrl Pts',(0.223725581741719,-0.0953220594732403,
0.200252612891201));
#30744=CARTESIAN_POINT('Ctrl Pts',(0.0411826615961353,-0.239673577332608,
0.18913565258292));
#30745=CARTESIAN_POINT('Ctrl Pts',(-0.179074949873739,-0.164534496276958,
0.178018692274637));
#30746=CARTESIAN_POINT('Ctrl Pts',(-0.235337503315095,0.06128355964017,
0.166901731966353));
#30747=CARTESIAN_POINT('Ctrl Pts',(-0.0760805235343836,0.230978803819408,
0.155784771658071));
#30748=CARTESIAN_POINT('Ctrl Pts',(0.152850454267675,0.189145963782275,
0.144667811349788));
#30749=CARTESIAN_POINT('Ctrl Pts',(0.241802105791721,-0.0259046503207544,
0.133550851041506));
#30750=CARTESIAN_POINT('Ctrl Pts',(0.109314754159658,-0.217232337426711,
0.122433890733223));
#30751=CARTESIAN_POINT('Ctrl Pts',(-0.123283586093291,-0.209620346682013,
0.11131693042494));
#30752=CARTESIAN_POINT('Ctrl Pts',(-0.242976912603923,-0.0100412419572166,
0.100199970116657));
#30753=CARTESIAN_POINT('Ctrl Pts',(-0.140160553667793,0.198735509804885,
0.0890830098083741));
#30754=CARTESIAN_POINT('Ctrl Pts',(0.091024974460894,0.225508548796274,
0.0779660495000909));
#30755=CARTESIAN_POINT('Ctrl Pts',(0.23882866217517,0.0457704056586039,
0.0668490891918084));
#30756=CARTESIAN_POINT('Ctrl Pts',(0.167957734834984,-0.175897589788799,
0.0557321288835253));
#30757=CARTESIAN_POINT('Ctrl Pts',(-0.0568077796437977,-0.236454060901771,
0.0446151685752427));
#30758=CARTESIAN_POINT('Ctrl Pts',(-0.229395040400805,-0.0805186419947185,
0.0334982082669599));
#30759=CARTESIAN_POINT('Ctrl Pts',(-0.192202303472141,0.149251313714896,
0.0223812479586771));
#30760=CARTESIAN_POINT('Ctrl Pts',(0.0216025916063335,0.242151157279311,
0.0112642876503943));
#30761=CARTESIAN_POINT('Ctrl Pts',(0.150043384986088,0.156507228866493,
0.00385298077820578));
#30762=CARTESIAN_POINT('Ctrl Pts',(0.181968494395784,0.0959811094385754,
0.000147327342111498));
#30763=CARTESIAN_POINT('Ctrl Pts',(0.181742788875947,0.0958620587959227,
0.));
#30764=CARTESIAN_POINT('Ctrl Pts',(0.174504469275331,0.106933967990604,
-2.81788574158242E-17));
#30765=CARTESIAN_POINT('Ctrl Pts',(0.16615526098928,0.117183932420547,-9.27869193614022E-17));
#30766=CARTESIAN_POINT('Ctrl Pts',(0.156880171409737,0.126533297037827,
2.04697370165263E-16));
#30767=CARTESIAN_POINT('Ctrl Pts',(0.15128023158171,0.13217808125668,3.25645692820429E-16));
#30768=CARTESIAN_POINT('Ctrl Pts',(0.145341937935802,0.13749388649769,2.01225074043376E-16));
#30769=CARTESIAN_POINT('Ctrl Pts',(0.139101245907215,0.142455889753469,
1.66533453693773E-16));
#30770=CARTESIAN_POINT('Ctrl Pts',(0.135040637805532,0.145684498139958,
1.43960784828397E-16));
#30771=CARTESIAN_POINT('Ctrl Pts',(0.130850103351038,0.148764420786474,
-1.1266670458931E-16));
#30772=CARTESIAN_POINT('Ctrl Pts',(0.126545459943985,0.151683176533579,
-1.52655665885959E-16));
#30773=CARTESIAN_POINT('Ctrl Pts',(0.122352033792771,0.154526521619693,
-1.91611449258523E-16));
#30774=CARTESIAN_POINT('Ctrl Pts',(0.118059533786955,0.157210759147407,
9.00868310955262E-17));
#30775=CARTESIAN_POINT('Ctrl Pts',(0.113682253713289,0.159728355552366,
6.59194920871187E-17));
#30776=CARTESIAN_POINT('Ctrl Pts',(0.10257577466787,0.166116256542462,4.59966795815047E-18));
#30777=CARTESIAN_POINT('Ctrl Pts',(0.0909137787356949,0.171441652247163,
8.12077434941466E-17));
#30778=CARTESIAN_POINT('Ctrl Pts',(0.0788520591185822,0.175593194714427,
2.0643209364124E-16));
#30779=CARTESIAN_POINT('Ctrl Pts',(0.0732665345230194,0.177515685312495,
2.64420814148192E-16));
#30780=CARTESIAN_POINT('Ctrl Pts',(0.0675951556350182,0.179185757356502,
3.458479309827E-16));
#30781=CARTESIAN_POINT('Ctrl Pts',(0.0618535813722568,0.180588437047447,
4.28476698566271E-16));
#30782=CARTESIAN_POINT('Ctrl Pts',(0.0574839813535566,0.181655940300613,
4.91360961288444E-16));
#30783=CARTESIAN_POINT('Ctrl Pts',(0.0530766090871315,0.182567386168162,
3.40638383294036E-16));
#30784=CARTESIAN_POINT('Ctrl Pts',(0.0486558084301484,0.183314182850192,
3.10515502199848E-16));
#30785=CARTESIAN_POINT('Ctrl Pts',(0.0379659386233148,0.18512000037568,
2.37675828554995E-16));
#30786=CARTESIAN_POINT('Ctrl Pts',(0.0271690281402411,0.185972684584687,
4.74617282448999E-16));
#30787=CARTESIAN_POINT('Ctrl Pts',(0.0163641619208266,0.185791435560747,
4.23272528138341E-16));
#30788=CARTESIAN_POINT('Ctrl Pts',(0.00736772073510989,0.185640522430428,
4.3031952015864E-16));
#30789=CARTESIAN_POINT('Ctrl Pts',(-0.00163453813579219,0.184771897471073,
6.67878087952716E-16));
#30790=CARTESIAN_POINT('Ctrl Pts',(-0.0105685044149961,0.183215538395939,
5.27355936696949E-16));
#30791=CARTESIAN_POINT('Ctrl Pts',(-0.0151046453702256,0.182425311085791,
3.9707342353691E-16));
#30792=CARTESIAN_POINT('Ctrl Pts',(-0.0196162098916884,0.181458430012929,
3.63725539130059E-16));
#30793=CARTESIAN_POINT('Ctrl Pts',(-0.024079466750711,0.180323824810446,
3.90312782094782E-16));
#30794=CARTESIAN_POINT('Ctrl Pts',(-0.0350902229812683,0.177524778800534,
4.55902924086132E-16));
#30795=CARTESIAN_POINT('Ctrl Pts',(-0.0458352633172663,0.173702776386141,
3.51897032873533E-16));
#30796=CARTESIAN_POINT('Ctrl Pts',(-0.0561677502272309,0.168929888351253,
4.75314232417645E-16));
#30797=CARTESIAN_POINT('Ctrl Pts',(-0.0622728678478303,0.166109749976353,
5.48237288230581E-16));
#30798=CARTESIAN_POINT('Ctrl Pts',(-0.0682334189441441,0.162957096799898,
5.45378188703878E-16));
#30799=CARTESIAN_POINT('Ctrl Pts',(-0.0740150970940476,0.159481877940378,
3.75567632548979E-16));
#30800=CARTESIAN_POINT('Ctrl Pts',(-0.0784470916501901,0.156817919368583,
2.45397906573034E-16));
#30801=CARTESIAN_POINT('Ctrl Pts',(-0.0827700074415804,0.153966080728667,
4.80659032402892E-16));
#30802=CARTESIAN_POINT('Ctrl Pts',(-0.0869532130138509,0.15094253677905,
4.90059381963448E-16));
#30803=CARTESIAN_POINT('Ctrl Pts',(-0.0932798978419366,0.146369725497697,
5.0427648124676E-16));
#30804=CARTESIAN_POINT('Ctrl Pts',(-0.0992975790462204,0.141398564153525,
4.93000331800633E-16));
#30805=CARTESIAN_POINT('Ctrl Pts',(-0.104950075896856,0.136047484562577,
5.88938620094126E-16));
#30806=CARTESIAN_POINT('Ctrl Pts',(-0.109220306833978,0.132004962077368,
6.61416085814314E-16));
#30807=CARTESIAN_POINT('Ctrl Pts',(-0.113281874229585,0.12774440154114,
3.167752875038E-16));
#30808=CARTESIAN_POINT('Ctrl Pts',(-0.117092856033647,0.123291942798165,
3.49980461278321E-16));
#30809=CARTESIAN_POINT('Ctrl Pts',(-0.12264309442135,0.116807470107011,
3.98339818428034E-16));
#30810=CARTESIAN_POINT('Ctrl Pts',(-0.127672471608383,0.109907592598991,
9.25668074629998E-17));
#30811=CARTESIAN_POINT('Ctrl Pts',(-0.132096989238305,0.102614780608902,
6.74915852372227E-17));
#30812=CARTESIAN_POINT('Ctrl Pts',(-0.13264315472071,0.101714550908896,
7.80582634118999E-17));
#30813=CARTESIAN_POINT('Ctrl Pts',(-0.133180081100841,0.100808327459116,
-1.29750824392398E-16));
#30814=CARTESIAN_POINT('Ctrl Pts',(-0.13370774202371,0.0998962637199363,
8.4296718910748E-17));
#30815=CARTESIAN_POINT('Ctrl Pts',(0.126907087985239,0.10793586530485,0.4));
#30816=CARTESIAN_POINT('Ctrl Pts',(0.135120918952714,0.100273232772193,
0.4));
#30817=CARTESIAN_POINT('Ctrl Pts',(0.142440334671478,0.0917705069751104,
0.4));
#30818=CARTESIAN_POINT('Ctrl Pts',(0.148860643047527,0.08262174487072,0.4));
#30819=CARTESIAN_POINT('Ctrl Pts',(0.153627635655852,0.0758289120700936,
0.4));
#30820=CARTESIAN_POINT('Ctrl Pts',(0.157898622412177,0.0686786359713564,
0.4));
#30821=CARTESIAN_POINT('Ctrl Pts',(0.161661540307137,0.0612359751064182,
0.4));
#30822=CARTESIAN_POINT('Ctrl Pts',(0.164102874102171,0.056407270361387,
0.4));
#30823=CARTESIAN_POINT('Ctrl Pts',(0.166331409569869,0.0514502806578965,
0.4));
#30824=CARTESIAN_POINT('Ctrl Pts',(0.168329235075816,0.0464171379264235,
0.4));
#30825=CARTESIAN_POINT('Ctrl Pts',(0.172801737816196,0.0351495149071816,
0.4));
#30826=CARTESIAN_POINT('Ctrl Pts',(0.176138845697143,0.0234718063959593,
0.4));
#30827=CARTESIAN_POINT('Ctrl Pts',(0.17831042601693,0.0115813652209228,
0.4));
#30828=CARTESIAN_POINT('Ctrl Pts',(0.179431215733824,0.00544450531438937,
0.4));
#30829=CARTESIAN_POINT('Ctrl Pts',(0.180240887278069,-0.000749624549012006,
0.4));
#30830=CARTESIAN_POINT('Ctrl Pts',(0.180730523800757,-0.00697642912666059,
0.4));
#30831=CARTESIAN_POINT('Ctrl Pts',(0.181117091707021,-0.0118924897078438,
0.4));
#30832=CARTESIAN_POINT('Ctrl Pts',(0.181303371987996,-0.0168290189998756,
0.4));
#30833=CARTESIAN_POINT('Ctrl Pts',(0.181285629855571,-0.021746975072603,
0.4));
#30834=CARTESIAN_POINT('Ctrl Pts',(0.181246813532722,-0.0325065030763667,
0.4));
#30835=CARTESIAN_POINT('Ctrl Pts',(0.180236611938718,-0.0432078221541177,
0.4));
#30836=CARTESIAN_POINT('Ctrl Pts',(0.178223999863926,-0.0537244994070257,
0.4));
#30837=CARTESIAN_POINT('Ctrl Pts',(0.177057515641798,-0.059819831060048,
0.4));
#30838=CARTESIAN_POINT('Ctrl Pts',(0.175553812784225,-0.0658533566784224,
0.4));
#30839=CARTESIAN_POINT('Ctrl Pts',(0.173731861666494,-0.071808724503393,
0.4));
#30840=CARTESIAN_POINT('Ctrl Pts',(0.171731410043636,-0.0783475526389198,
0.4));
#30841=CARTESIAN_POINT('Ctrl Pts',(0.169342367274103,-0.084801264593441,
0.4));
#30842=CARTESIAN_POINT('Ctrl Pts',(0.166610322749882,-0.0910962279747303,
0.4));
#30843=CARTESIAN_POINT('Ctrl Pts',(0.161428849033874,-0.103034974585266,
0.4));
#30844=CARTESIAN_POINT('Ctrl Pts',(0.155012393449103,-0.114432718842341,
0.4));
#30845=CARTESIAN_POINT('Ctrl Pts',(0.147536507995649,-0.125146591163663,
0.4));
#30846=CARTESIAN_POINT('Ctrl Pts',(0.143512554735272,-0.130913415940082,
0.4));
#30847=CARTESIAN_POINT('Ctrl Pts',(0.139180426978968,-0.136482273587012,
0.4));
#30848=CARTESIAN_POINT('Ctrl Pts',(0.13456102284103,-0.141828718973796,
0.4));
#30849=CARTESIAN_POINT('Ctrl Pts',(0.131202022825332,-0.145716387080307,
0.4));
#30850=CARTESIAN_POINT('Ctrl Pts',(0.127692523532622,-0.149483993751978,
0.4));
#30851=CARTESIAN_POINT('Ctrl Pts',(0.124053969377856,-0.15310949025686,
0.4));
#30852=CARTESIAN_POINT('Ctrl Pts',(0.117250830652081,-0.159888214613682,
0.4));
#30853=CARTESIAN_POINT('Ctrl Pts',(0.109987812654579,-0.16618218257803,
0.399999999999999));
#30854=CARTESIAN_POINT('Ctrl Pts',(0.102320566390068,-0.171932690825377,
0.399999999999999));
#30855=CARTESIAN_POINT('Ctrl Pts',(0.0968356651066751,-0.176046419402484,
0.4));
#30856=CARTESIAN_POINT('Ctrl Pts',(0.0911417236297836,-0.179882091250733,
0.4));
#30857=CARTESIAN_POINT('Ctrl Pts',(0.0852821558629418,-0.183402277546523,
0.4));
#30858=CARTESIAN_POINT('Ctrl Pts',(0.0761595778105699,-0.1888827456493,
0.4));
#30859=CARTESIAN_POINT('Ctrl Pts',(0.0666264887468849,-0.193608063008219,
0.4));
#30860=CARTESIAN_POINT('Ctrl Pts',(0.0567496916571122,-0.197494094154161,
0.4));
#30861=CARTESIAN_POINT('Ctrl Pts',(0.0555606243966102,-0.197961933309601,
0.4));
#30862=CARTESIAN_POINT('Ctrl Pts',(0.0543665677551527,-0.198417583105329,
0.4));
#30863=CARTESIAN_POINT('Ctrl Pts',(0.0531676903274471,-0.198861095112417,
0.4));
#30864=CARTESIAN_POINT('Ctrl Pts',(-0.0530701539231891,-0.198716381290575,
0.39988111122049));
#30865=CARTESIAN_POINT('Ctrl Pts',(-0.119166933292682,-0.181064257030941,
0.396175457784396));
#30866=CARTESIAN_POINT('Ctrl Pts',(-0.231217597730413,-0.0749271919797139,
0.388764150912208));
#30867=CARTESIAN_POINT('Ctrl Pts',(-0.188233160600942,0.154135205755113,
0.377647190603924));
#30868=CARTESIAN_POINT('Ctrl Pts',(0.027448085609834,0.241502672443478,
0.366530230295642));
#30869=CARTESIAN_POINT('Ctrl Pts',(0.217832547874475,0.107973703950356,
0.355413269987359));
#30870=CARTESIAN_POINT('Ctrl Pts',(0.2088115571148,-0.124576002900519,0.344296309679076));
#30871=CARTESIAN_POINT('Ctrl Pts',(0.00851948372747169,-0.242967349770974,
0.333179349370793));
#30872=CARTESIAN_POINT('Ctrl Pts',(-0.199551799190759,-0.138889905056905,
0.322062389062511));
#30873=CARTESIAN_POINT('Ctrl Pts',(-0.224887572854444,0.0924014979391681,
0.310945428754227));
#30874=CARTESIAN_POINT('Ctrl Pts',(-0.044267354029904,0.239062074042455,
0.299828468445945));
#30875=CARTESIAN_POINT('Ctrl Pts',(0.17688916429529,0.166797563884364,0.288711508137662));
#30876=CARTESIAN_POINT('Ctrl Pts',(0.236054132464953,-0.0582213149159194,
0.277594547829379));
#30877=CARTESIAN_POINT('Ctrl Pts',(0.0790422580723326,-0.229920204906449,
0.266477587521096));
#30878=CARTESIAN_POINT('Ctrl Pts',(-0.1503552283045,-0.191061333140319,
0.255360627212814));
#30879=CARTESIAN_POINT('Ctrl Pts',(-0.242059194800053,0.0227699515372025,
0.24424366690453));
#30880=CARTESIAN_POINT('Ctrl Pts',(-0.112087717542688,0.215748532186423,
0.233126706596248));
#30881=CARTESIAN_POINT('Ctrl Pts',(0.12053246817559,0.211146946028599,0.222009746287965));
#30882=CARTESIAN_POINT('Ctrl Pts',(0.2427702968486,0.0131791041947362,0.210892785979682));
#30883=CARTESIAN_POINT('Ctrl Pts',(0.142681575266364,-0.196857993321032,
0.199775825671399));
#30884=CARTESIAN_POINT('Ctrl Pts',(-0.088073456719532,-0.226614588589072,
0.188658865363117));
#30885=CARTESIAN_POINT('Ctrl Pts',(-0.238171720883513,-0.0488398692285348,
0.177541905054834));
#30886=CARTESIAN_POINT('Ctrl Pts',(-0.170154794877542,0.17366188873646,
0.166424944746551));
#30887=CARTESIAN_POINT('Ctrl Pts',(0.0536881709643731,0.237125892724105,
0.155307984438268));
#30888=CARTESIAN_POINT('Ctrl Pts',(0.22836399769663,0.0834324284708191,
0.144191024129985));
#30889=CARTESIAN_POINT('Ctrl Pts',(0.193906557049213,-0.146667554740565,
0.133074063821703));
#30890=CARTESIAN_POINT('Ctrl Pts',(-0.0181287510056,-0.242450976667101,
0.12195710351342));
#30891=CARTESIAN_POINT('Ctrl Pts',(-0.213561473377095,-0.116200156085957,
0.110840143205137));
#30892=CARTESIAN_POINT('Ctrl Pts',(-0.213417683574561,0.116465305142727,
0.0997231828968541));
#30893=CARTESIAN_POINT('Ctrl Pts',(-0.0178264954593966,0.242473544582663,
0.0886062225885714));
#30894=CARTESIAN_POINT('Ctrl Pts',(0.194086798383876,0.146426051546118,
0.0774892622802885));
#30895=CARTESIAN_POINT('Ctrl Pts',(0.228263539268917,-0.08371507562078,
0.0663723019720058));
#30896=CARTESIAN_POINT('Ctrl Pts',(0.053387176172982,-0.23719429948306,
0.0552553416637228));
#30897=CARTESIAN_POINT('Ctrl Pts',(-0.170358267049339,-0.173446751211026,
0.0441383813554401));
#30898=CARTESIAN_POINT('Ctrl Pts',(-0.238134013450897,0.0491287952340117,
0.0330214210471573));
#30899=CARTESIAN_POINT('Ctrl Pts',(-0.0877476633139311,0.226737044263148,
0.0219044607388744));
#30900=CARTESIAN_POINT('Ctrl Pts',(0.142841392439922,0.196655218102167,
0.0107875004305917));
#30901=CARTESIAN_POINT('Ctrl Pts',(0.242917667120415,-0.0134309867011242,
-0.00032945987769134));
#30902=CARTESIAN_POINT('Ctrl Pts',(0.11992182972462,-0.211425239089247,
-0.0114476947911144));
#30903=CARTESIAN_POINT('Ctrl Pts',(-0.03443369593138,-0.214017241553922,
-0.0188602762684437));
#30904=CARTESIAN_POINT('Ctrl Pts',(-0.0951131155041543,-0.182368133997801,
-0.0225672043096786));
#30905=CARTESIAN_POINT('Ctrl Pts',(-0.0496833462568047,-0.18603478695103,
0.407459442196852));
#30906=CARTESIAN_POINT('Ctrl Pts',(-0.111561990525051,-0.169509178168571,
0.403753788760758));
#30907=CARTESIAN_POINT('Ctrl Pts',(-0.216461855100954,-0.0701455215028423,
0.396342481888569));
#30908=CARTESIAN_POINT('Ctrl Pts',(-0.176220579813749,0.144298673204884,
0.385225521580286));
#30909=CARTESIAN_POINT('Ctrl Pts',(0.0256964157935848,0.22609056145417,
0.374108561272003));
#30910=CARTESIAN_POINT('Ctrl Pts',(0.203931006450699,0.101083085753992,
0.362991600963721));
#30911=CARTESIAN_POINT('Ctrl Pts',(0.195485713298902,-0.116625866515355,
0.351874640655438));
#30912=CARTESIAN_POINT('Ctrl Pts',(0.00797579107409027,-0.227461766650253,
0.340757680347155));
#30913=CARTESIAN_POINT('Ctrl Pts',(-0.18681689052028,-0.130026290379794,
0.329640720038872));
#30914=CARTESIAN_POINT('Ctrl Pts',(-0.210535796959459,0.0865046599149425,
0.318523759730589));
#30915=CARTESIAN_POINT('Ctrl Pts',(-0.04144231956296,0.223805716085013,
0.307406799422307));
#30916=CARTESIAN_POINT('Ctrl Pts',(0.165600529658904,0.156152950550184,
0.296289839114023));
#30917=CARTESIAN_POINT('Ctrl Pts',(0.22098973399588,-0.0545057727302003,
0.285172878805742));
#30918=CARTESIAN_POINT('Ctrl Pts',(0.0739979741232949,-0.215247258719768,
0.274055918497458));
#30919=CARTESIAN_POINT('Ctrl Pts',(-0.140759924687336,-0.178868265285912,
0.262938958189176));
#30920=CARTESIAN_POINT('Ctrl Pts',(-0.226611567912552,0.0213168288170191,
0.251821997880892));
#30921=CARTESIAN_POINT('Ctrl Pts',(-0.104934553042155,0.201979987556277,
0.24070503757261));
#30922=CARTESIAN_POINT('Ctrl Pts',(0.112840380305332,0.197672063393468,
0.229588077264327));
#30923=CARTESIAN_POINT('Ctrl Pts',(0.227277289164333,0.0123380459383872,
0.218471116956044));
#30924=CARTESIAN_POINT('Ctrl Pts',(0.133575985452863,-0.184294996764932,
0.207354156647761));
#30925=CARTESIAN_POINT('Ctrl Pts',(-0.082452823720155,-0.212152598765963,
0.196237196339479));
#30926=CARTESIAN_POINT('Ctrl Pts',(-0.22297218309111,-0.0457230280042223,
0.185120236031196));
#30927=CARTESIAN_POINT('Ctrl Pts',(-0.159295931257184,0.162579210947684,
0.174003275722913));
#30928=CARTESIAN_POINT('Ctrl Pts',(0.0502619229591482,0.221993097131716,
0.16288631541463));
#30929=CARTESIAN_POINT('Ctrl Pts',(0.213790364855006,0.0781079745644107,
0.151769355106347));
#30930=CARTESIAN_POINT('Ctrl Pts',(0.181531913950816,-0.137307589447754,
0.140652394798065));
#30931=CARTESIAN_POINT('Ctrl Pts',(-0.0169718183730586,-0.226978347217279,
0.129535434489782));
#30932=CARTESIAN_POINT('Ctrl Pts',(-0.199932501501024,-0.108784545797044,
0.118418474181499));
#30933=CARTESIAN_POINT('Ctrl Pts',(-0.199797888012663,0.109032773688304,
0.107301513873216));
#30934=CARTESIAN_POINT('Ctrl Pts',(-0.0166888520379352,0.226999474903564,
0.0961845535649328));
#30935=CARTESIAN_POINT('Ctrl Pts',(0.181700652723512,0.137081498397608,
0.0850675932566501));
#30936=CARTESIAN_POINT('Ctrl Pts',(0.213696317438905,-0.0783725838632703,
0.0739506329483673));
#30937=CARTESIAN_POINT('Ctrl Pts',(0.0499801369205431,-0.222057138338313,
0.0628336726400844));
#30938=CARTESIAN_POINT('Ctrl Pts',(-0.159486418331701,-0.16237780297392,
0.0517167123318017));
#30939=CARTESIAN_POINT('Ctrl Pts',(-0.222936882054789,0.0459935154573673,
0.0405997520235189));
#30940=CARTESIAN_POINT('Ctrl Pts',(-0.0821478216543599,0.212267239617864,
0.029482791715236));
#30941=CARTESIAN_POINT('Ctrl Pts',(0.133725603484557,0.184105162165512,
0.0183658314069533));
#30942=CARTESIAN_POINT('Ctrl Pts',(0.227415254625167,-0.012573853918123,
0.00724887109867029));
#30943=CARTESIAN_POINT('Ctrl Pts',(0.112268711309588,-0.197932596470366,
-0.00386936381475281));
#30944=CARTESIAN_POINT('Ctrl Pts',(-0.0322362215179624,-0.200359183665446,
-0.0112819452920821));
#30945=CARTESIAN_POINT('Ctrl Pts',(-0.0890432286666411,-0.170729844890482,
-0.0149888733333169));
#30946=CARTESIAN_POINT('Ctrl Pts',(-0.0462965385904204,-0.173353192611486,
0.415037773173213));
#30947=CARTESIAN_POINT('Ctrl Pts',(-0.103957047757422,-0.1579540993062,
0.411332119737119));
#30948=CARTESIAN_POINT('Ctrl Pts',(-0.201706112471495,-0.0653638510259706,
0.40392081286493));
#30949=CARTESIAN_POINT('Ctrl Pts',(-0.164207999026558,0.134462140654653,
0.392803852556647));
#30950=CARTESIAN_POINT('Ctrl Pts',(0.0239447459773354,0.210678450464861,
0.381686892248365));
#30951=CARTESIAN_POINT('Ctrl Pts',(0.190029465026925,0.0941924675576273,
0.370569931940081));
#30952=CARTESIAN_POINT('Ctrl Pts',(0.182159869483005,-0.108675730130192,
0.359452971631799));
#30953=CARTESIAN_POINT('Ctrl Pts',(0.00743209842070957,-0.211956183529533,
0.348336011323516));
#30954=CARTESIAN_POINT('Ctrl Pts',(-0.174081981849801,-0.121162675702683,
0.337219051015233));
#30955=CARTESIAN_POINT('Ctrl Pts',(-0.196184021064473,0.0806078218907167,
0.326102090706951));
#30956=CARTESIAN_POINT('Ctrl Pts',(-0.0386172850960161,0.208549358127571,
0.314985130398667));
#30957=CARTESIAN_POINT('Ctrl Pts',(0.15431189502252,0.145508337216003,0.303868170090385));
#30958=CARTESIAN_POINT('Ctrl Pts',(0.205925335526805,-0.0507902305444811,
0.292751209782102));
#30959=CARTESIAN_POINT('Ctrl Pts',(0.0689536901742569,-0.200574312533087,
0.281634249473819));
#30960=CARTESIAN_POINT('Ctrl Pts',(-0.131164621070171,-0.166675197431506,
0.270517289165536));
#30961=CARTESIAN_POINT('Ctrl Pts',(-0.211163941025053,0.0198637060968362,
0.259400328857254));
#30962=CARTESIAN_POINT('Ctrl Pts',(-0.0977813885416242,0.188211442926131,
0.248283368548971));
#30963=CARTESIAN_POINT('Ctrl Pts',(0.105148292435073,0.184197180758337,
0.237166408240688));
#30964=CARTESIAN_POINT('Ctrl Pts',(0.211784281480065,0.0114969876820384,
0.226049447932405));
#30965=CARTESIAN_POINT('Ctrl Pts',(0.124470395639363,-0.171732000208833,
0.214932487624122));
#30966=CARTESIAN_POINT('Ctrl Pts',(-0.0768321907207784,-0.197690608942853,
0.20381552731584));
#30967=CARTESIAN_POINT('Ctrl Pts',(-0.207772645298705,-0.0426061867799098,
0.192698567007556));
#30968=CARTESIAN_POINT('Ctrl Pts',(-0.148437067636826,0.151496533158908,
0.181581606699274));
#30969=CARTESIAN_POINT('Ctrl Pts',(0.0468356749539237,0.206860301539328,
0.170464646390991));
#30970=CARTESIAN_POINT('Ctrl Pts',(0.199216732013379,0.0727835206580018,
0.159347686082708));
#30971=CARTESIAN_POINT('Ctrl Pts',(0.169157270852419,-0.127947624154943,
0.148230725774426));
#30972=CARTESIAN_POINT('Ctrl Pts',(-0.0158148857405171,-0.211505717767457,
0.137113765466142));
#30973=CARTESIAN_POINT('Ctrl Pts',(-0.186303529624954,-0.101368935508133,
0.12599680515786));
#30974=CARTESIAN_POINT('Ctrl Pts',(-0.186178092450765,0.101600242233881,
0.114879844849577));
#30975=CARTESIAN_POINT('Ctrl Pts',(-0.015551208616474,0.211525405224465,
0.103762884541294));
#30976=CARTESIAN_POINT('Ctrl Pts',(0.16931450706315,0.1277369452491,0.0926459242330117));
#30977=CARTESIAN_POINT('Ctrl Pts',(0.199129095608893,-0.0730300921057608,
0.0815289639247289));
#30978=CARTESIAN_POINT('Ctrl Pts',(0.0465730976681044,-0.206919977193565,
0.0704120036164461));
#30979=CARTESIAN_POINT('Ctrl Pts',(-0.148614569614064,-0.151308854736816,
0.0592950433081632));
#30980=CARTESIAN_POINT('Ctrl Pts',(-0.207739750658681,0.0428582356807231,
0.0481780829998806));
#30981=CARTESIAN_POINT('Ctrl Pts',(-0.0765479799947886,0.197797434972579,
0.0370611226915976));
#30982=CARTESIAN_POINT('Ctrl Pts',(0.124609814529192,0.171555106228858,
0.025944162383315));
#30983=CARTESIAN_POINT('Ctrl Pts',(0.211912842129918,-0.0117167211351222,
0.0148272020750319));
#30984=CARTESIAN_POINT('Ctrl Pts',(0.104615592894555,-0.184439953851485,
0.00370896716160887));
#30985=CARTESIAN_POINT('Ctrl Pts',(-0.0300387471045446,-0.186701125776971,
-0.00370361431572043));
#30986=CARTESIAN_POINT('Ctrl Pts',(-0.0829733418291278,-0.159091555783164,
-0.00741054235695528));
#30987=CARTESIAN_POINT('Ctrl Pts',(-0.0429097309240361,-0.160671598271941,
0.422616104149575));
#30988=CARTESIAN_POINT('Ctrl Pts',(-0.0963521049897916,-0.14639902044383,
0.41891045071348));
#30989=CARTESIAN_POINT('Ctrl Pts',(-0.186950369842037,-0.0605821805490989,
0.411499143841292));
#30990=CARTESIAN_POINT('Ctrl Pts',(-0.152195418239366,0.124625608104424,
0.400382183533009));
#30991=CARTESIAN_POINT('Ctrl Pts',(0.022193076161086,0.195266339475553,
0.389265223224726));
#30992=CARTESIAN_POINT('Ctrl Pts',(0.17612792360315,0.0873018493612629,
0.378148262916443));
#30993=CARTESIAN_POINT('Ctrl Pts',(0.168834025667108,-0.100725593745027,
0.367031302608161));
#30994=CARTESIAN_POINT('Ctrl Pts',(0.00688840576732832,-0.196450600408813,
0.355914342299878));
#30995=CARTESIAN_POINT('Ctrl Pts',(-0.161347073179323,-0.112299061025572,
0.344797381991595));
#30996=CARTESIAN_POINT('Ctrl Pts',(-0.181832245169488,0.074710983866491,
0.333680421683312));
#30997=CARTESIAN_POINT('Ctrl Pts',(-0.0357922506290721,0.193293000170129,
0.322563461375029));
#30998=CARTESIAN_POINT('Ctrl Pts',(0.143023260386134,0.134863723881822,
0.311446501066746));
#30999=CARTESIAN_POINT('Ctrl Pts',(0.190860937057732,-0.0470746883587621,
0.300329540758464));
#31000=CARTESIAN_POINT('Ctrl Pts',(0.0639094062252192,-0.185901366346407,
0.28921258045018));
#31001=CARTESIAN_POINT('Ctrl Pts',(-0.121569317453007,-0.154482129577099,
0.278095620141899));
#31002=CARTESIAN_POINT('Ctrl Pts',(-0.195716314137552,0.0184105833766533,
0.266978659833615));
#31003=CARTESIAN_POINT('Ctrl Pts',(-0.090628224041093,0.174442898295985,
0.255861699525333));
#31004=CARTESIAN_POINT('Ctrl Pts',(0.0974562045648148,0.170722298123207,
0.244744739217049));
#31005=CARTESIAN_POINT('Ctrl Pts',(0.196291273795798,0.0106559294256891,
0.233627778908767));
#31006=CARTESIAN_POINT('Ctrl Pts',(0.115364805825862,-0.159169003652733,
0.222510818600484));
#31007=CARTESIAN_POINT('Ctrl Pts',(-0.0712115577214017,-0.183228619119744,
0.211393858292202));
#31008=CARTESIAN_POINT('Ctrl Pts',(-0.192573107506301,-0.0394893455555971,
0.200276897983918));
#31009=CARTESIAN_POINT('Ctrl Pts',(-0.137578204016468,0.140413855370133,
0.189159937675636));
#31010=CARTESIAN_POINT('Ctrl Pts',(0.0434094269486991,0.191727505946939,
0.178042977367353));
#31011=CARTESIAN_POINT('Ctrl Pts',(0.184643099171754,0.0674590667515935,
0.16692601705907));
#31012=CARTESIAN_POINT('Ctrl Pts',(0.156782627754022,-0.118587658862133,
0.155809056750787));
#31013=CARTESIAN_POINT('Ctrl Pts',(-0.0146579531079754,-0.196033088317636,
0.144692096442504));
#31014=CARTESIAN_POINT('Ctrl Pts',(-0.172674557748884,-0.09395332521922,
0.133575136134222));
#31015=CARTESIAN_POINT('Ctrl Pts',(-0.172558296888866,0.0941677107794582,
0.122458175825939));
#31016=CARTESIAN_POINT('Ctrl Pts',(-0.014413565195013,0.196051335545365,
0.111341215517656));
#31017=CARTESIAN_POINT('Ctrl Pts',(0.156928361402787,0.118392392100591,
0.100224255209373));
#31018=CARTESIAN_POINT('Ctrl Pts',(0.18456187377888,-0.0676876003482512,
0.0891072949010907));
#31019=CARTESIAN_POINT('Ctrl Pts',(0.043166058415666,-0.191782816048817,
0.0779903345928075));
#31020=CARTESIAN_POINT('Ctrl Pts',(-0.137742720896427,-0.140239906499711,
0.0668733742845249));
#31021=CARTESIAN_POINT('Ctrl Pts',(-0.192542619262574,0.0397229559040788,
0.0557564139762422));
#31022=CARTESIAN_POINT('Ctrl Pts',(-0.0709481383352174,0.183327630327294,
0.0446394536679593));
#31023=CARTESIAN_POINT('Ctrl Pts',(0.115494025573827,0.159005050292203,
0.0335224933596767));
#31024=CARTESIAN_POINT('Ctrl Pts',(0.19641042963467,-0.0108595883521212,
0.0224055330513936));
#31025=CARTESIAN_POINT('Ctrl Pts',(0.0969624744795222,-0.170947311232604,
0.0112872981379705));
#31026=CARTESIAN_POINT('Ctrl Pts',(-0.027841272691127,-0.173043067888495,
0.00387471666064119));
#31027=CARTESIAN_POINT('Ctrl Pts',(-0.0769034549916146,-0.147453266675846,
0.000167788619406336));
#31028=CARTESIAN_POINT('Ctrl Pts',(-0.0769902040670465,-0.147743251885541,
-6.93889390390723E-18));
#31029=CARTESIAN_POINT('Ctrl Pts',(-0.0676919232959199,-0.154046060402415,
-2.05855969193849E-16));
#31030=CARTESIAN_POINT('Ctrl Pts',(-0.0577736401978069,-0.159289942753595,
-1.00246838828094E-16));
#31031=CARTESIAN_POINT('Ctrl Pts',(-0.0474255897416162,-0.163513503779695,
-1.90819582357449E-16));
#31032=CARTESIAN_POINT('Ctrl Pts',(-0.0397423269308822,-0.166649430638389,
-3.11176017719216E-16));
#31033=CARTESIAN_POINT('Ctrl Pts',(-0.0318209566269663,-0.169222252729945,
1.95009950297112E-17));
#31034=CARTESIAN_POINT('Ctrl Pts',(-0.0237275895516037,-0.171234685365662,
-2.0122792321331E-16));
#31035=CARTESIAN_POINT('Ctrl Pts',(-0.0184767120920151,-0.172540327018564,
-2.79520754060125E-16));
#31036=CARTESIAN_POINT('Ctrl Pts',(-0.0131481186698344,-0.173609960486947,
-2.33518219162689E-16));
#31037=CARTESIAN_POINT('Ctrl Pts',(-0.00779661953491697,-0.174437723369069,
-1.66533453693773E-16));
#31038=CARTESIAN_POINT('Ctrl Pts',(0.00418371951149402,-0.176290826532845,
-1.65754361308467E-17));
#31039=CARTESIAN_POINT('Ctrl Pts',(0.0163112126214376,-0.176945748924033,
2.86527215930858E-16));
#31040=CARTESIAN_POINT('Ctrl Pts',(0.0283867514614758,-0.176417025598077,
4.31946145518225E-16));
#31041=CARTESIAN_POINT('Ctrl Pts',(0.0346191147784547,-0.17614414370807,
5.06998995280064E-16));
#31042=CARTESIAN_POINT('Ctrl Pts',(0.0408380822565802,-0.17555520239787,
4.4015761051379E-16));
#31043=CARTESIAN_POINT('Ctrl Pts',(0.0470176916982643,-0.174646980992462,
2.72351585728359E-16));
#31044=CARTESIAN_POINT('Ctrl Pts',(0.0518965299270048,-0.173929934817509,
1.39867735986388E-16));
#31045=CARTESIAN_POINT('Ctrl Pts',(0.0567507558014769,-0.173013065902084,
2.5227236170911E-16));
#31046=CARTESIAN_POINT('Ctrl Pts',(0.0615414748941956,-0.171901420573325,
2.04697370165263E-16));
#31047=CARTESIAN_POINT('Ctrl Pts',(0.0720225956837857,-0.169469366274084,
1.00612947078832E-16));
#31048=CARTESIAN_POINT('Ctrl Pts',(0.0822308156893155,-0.166103230285251,
6.54325850411354E-17));
#31049=CARTESIAN_POINT('Ctrl Pts',(0.0920359693799996,-0.161800897340594,
4.85722573273506E-17));
#31050=CARTESIAN_POINT('Ctrl Pts',(0.097718907582874,-0.159307321714552,
2.35558750287395E-17));
#31051=CARTESIAN_POINT('Ctrl Pts',(0.103266552483572,-0.156498733846988,
1.93700674136354E-16));
#31052=CARTESIAN_POINT('Ctrl Pts',(0.108667183415534,-0.15339726738813,
3.00107161343988E-16));
#31053=CARTESIAN_POINT('Ctrl Pts',(0.11459693992244,-0.149991935465425,
-9.62025511039274E-17));
#31054=CARTESIAN_POINT('Ctrl Pts',(0.120357245189988,-0.146226692136978,
-9.37471224547374E-17));
#31055=CARTESIAN_POINT('Ctrl Pts',(0.125886456988692,-0.142162369288104,
-1.00613961606655E-16));
#31056=CARTESIAN_POINT('Ctrl Pts',(0.136372892719963,-0.134454171104081,
-1.13637276694791E-16));
#31057=CARTESIAN_POINT('Ctrl Pts',(0.146057084193878,-0.125662334494057,
2.63201407223155E-16));
#31058=CARTESIAN_POINT('Ctrl Pts',(0.154838806086005,-0.115989804239992,
1.60461921527855E-16));
#31059=CARTESIAN_POINT('Ctrl Pts',(0.159565621700614,-0.110783505566531,
1.05161763860969E-16));
#31060=CARTESIAN_POINT('Ctrl Pts',(0.164030860393261,-0.105320811841541,
2.34445481277501E-16));
#31061=CARTESIAN_POINT('Ctrl Pts',(0.168215340079027,-0.0996275370064118,
1.8995222061946E-16));
#31062=CARTESIAN_POINT('Ctrl Pts',(0.171258070102838,-0.0954876917746175,
1.57599099030174E-16));
#31063=CARTESIAN_POINT('Ctrl Pts',(0.174150262314154,-0.0912278383229185,
-1.38974090381786E-17));
#31064=CARTESIAN_POINT('Ctrl Pts',(0.176875192571848,-0.0868737897286597,
-2.68882138776405E-17));
#31065=CARTESIAN_POINT('Ctrl Pts',(0.18196979446539,-0.0787333449777348,
-5.11761672103458E-17));
#31066=CARTESIAN_POINT('Ctrl Pts',(0.186489538005871,-0.0702524649460043,
-1.10733251100512E-16));
#31067=CARTESIAN_POINT('Ctrl Pts',(0.190389583958077,-0.0614984559805871,
1.94289029309402E-16));
#31068=CARTESIAN_POINT('Ctrl Pts',(0.193180561397451,-0.0552338524795093,
4.12571150485138E-16));
#31069=CARTESIAN_POINT('Ctrl Pts',(0.19565375183857,-0.0488272373071404,
6.43798831786931E-17));
#31070=CARTESIAN_POINT('Ctrl Pts',(0.197782303704477,-0.0423293043071611,
-3.20923843055709E-17));
#31071=CARTESIAN_POINT('Ctrl Pts',(0.201094791365034,-0.0322171133728858,
-1.82224124455317E-16));
#31072=CARTESIAN_POINT('Ctrl Pts',(0.203579910696782,-0.0218728104555898,
-6.96994360509918E-17));
#31073=CARTESIAN_POINT('Ctrl Pts',(0.205170522984607,-0.0113802171361648,
-1.25713241899694E-16));
#31074=CARTESIAN_POINT('Ctrl Pts',(0.205362040344674,-0.0101168584986283,
-9.17536921087371E-17));
#31075=CARTESIAN_POINT('Ctrl Pts',(0.205540563699428,-0.00885134802550821,
-3.06470418352831E-16));
#31076=CARTESIAN_POINT('Ctrl Pts',(0.205706180843763,-0.00758383860674098,
-1.47153339860595E-16));
#31077=CARTESIAN_POINT('Ctrl Pts',(-0.0530170217188623,-0.198517432567172,
0.4));
#31078=CARTESIAN_POINT('Ctrl Pts',(-0.0654220238787413,-0.193924320176368,
0.4));
#31079=CARTESIAN_POINT('Ctrl Pts',(-0.07727288556064,-0.188065277790972,
0.4));
#31080=CARTESIAN_POINT('Ctrl Pts',(-0.0884517548081647,-0.181103168839149,
0.4));
#31081=CARTESIAN_POINT('Ctrl Pts',(-0.0952010467673211,-0.17689976463727,
0.4));
#31082=CARTESIAN_POINT('Ctrl Pts',(-0.101704904097436,-0.172293295443026,
0.4));
#31083=CARTESIAN_POINT('Ctrl Pts',(-0.107931126215051,-0.167313289922026,
0.4));
#31084=CARTESIAN_POINT('Ctrl Pts',(-0.111959846876041,-0.164090942444648,
0.4));
#31085=CARTESIAN_POINT('Ctrl Pts',(-0.11587376397307,-0.160710653528623,
0.4));
#31086=CARTESIAN_POINT('Ctrl Pts',(-0.119657579752374,-0.157184731207288,
0.4));
#31087=CARTESIAN_POINT('Ctrl Pts',(-0.123317881187486,-0.153773904865407,
0.4));
#31088=CARTESIAN_POINT('Ctrl Pts',(-0.126848621970303,-0.150234155769173,
0.4));
#31089=CARTESIAN_POINT('Ctrl Pts',(-0.130239379311871,-0.146577572125245,
0.4));
#31090=CARTESIAN_POINT('Ctrl Pts',(-0.138953512703323,-0.137180273993772,
0.4));
#31091=CARTESIAN_POINT('Ctrl Pts',(-0.146755875032497,-0.127003654809211,
0.4));
#31092=CARTESIAN_POINT('Ctrl Pts',(-0.153503490990357,-0.116175026119951,
0.4));
#31093=CARTESIAN_POINT('Ctrl Pts',(-0.156641420012712,-0.111139252233509,
0.4));
#31094=CARTESIAN_POINT('Ctrl Pts',(-0.159550584997633,-0.105962198003635,
0.4));
#31095=CARTESIAN_POINT('Ctrl Pts',(-0.162212724451348,-0.100655900626943,
0.4));
#31096=CARTESIAN_POINT('Ctrl Pts',(-0.164244214036353,-0.0966066432371229,
0.4));
#31097=CARTESIAN_POINT('Ctrl Pts',(-0.166130198465154,-0.0924843279899854,
0.4));
#31098=CARTESIAN_POINT('Ctrl Pts',(-0.16785638026916,-0.0883115908809607,
0.4));
#31099=CARTESIAN_POINT('Ctrl Pts',(-0.172012349337959,-0.0782652757610305,
0.4));
#31100=CARTESIAN_POINT('Ctrl Pts',(-0.175258071106289,-0.0679005050150562,
0.4));
#31101=CARTESIAN_POINT('Ctrl Pts',(-0.177491918105115,-0.0572965665658759,
0.4));
#31102=CARTESIAN_POINT('Ctrl Pts',(-0.179346683049967,-0.0484921080137729,
0.4));
#31103=CARTESIAN_POINT('Ctrl Pts',(-0.180503025417514,-0.039522267403315,
0.4));
#31104=CARTESIAN_POINT('Ctrl Pts',(-0.180973680426715,-0.0304659686020515,
0.4));
#31105=CARTESIAN_POINT('Ctrl Pts',(-0.181212650830767,-0.0258677228776098,
0.4));
#31106=CARTESIAN_POINT('Ctrl Pts',(-0.181273928531148,-0.0212541273507348,
0.4));
#31107=CARTESIAN_POINT('Ctrl Pts',(-0.181160938580718,-0.0166503054466016,
0.4));
#31108=CARTESIAN_POINT('Ctrl Pts',(-0.180882194042426,-0.00529274483024155,
0.4));
#31109=CARTESIAN_POINT('Ctrl Pts',(-0.179547011733344,0.00603339551763739,
0.4));
#31110=CARTESIAN_POINT('Ctrl Pts',(-0.177192981605961,0.0171689196549591,
0.4));
#31111=CARTESIAN_POINT('Ctrl Pts',(-0.175802060433226,0.0237485450012686,
0.4));
#31112=CARTESIAN_POINT('Ctrl Pts',(-0.174054789653161,0.0302612200901589,
0.4));
#31113=CARTESIAN_POINT('Ctrl Pts',(-0.171953235151015,0.0366712838759848,
0.4));
#31114=CARTESIAN_POINT('Ctrl Pts',(-0.170342278092587,0.0415849501597783,
0.4));
#31115=CARTESIAN_POINT('Ctrl Pts',(-0.168523879724122,0.0464340797721413,
0.4));
#31116=CARTESIAN_POINT('Ctrl Pts',(-0.166506993102895,0.0511852100193018,
0.4));
#31117=CARTESIAN_POINT('Ctrl Pts',(-0.163456650544741,0.0583708270191453,
0.4));
#31118=CARTESIAN_POINT('Ctrl Pts',(-0.159949186498915,0.0653438287379616,
0.4));
#31119=CARTESIAN_POINT('Ctrl Pts',(-0.155990069415437,0.0720453408263799,
0.4));
#31120=CARTESIAN_POINT('Ctrl Pts',(-0.152999118912724,0.0771080582270448,
0.4));
#31121=CARTESIAN_POINT('Ctrl Pts',(-0.149749165779154,0.0820158613244291,
0.4));
#31122=CARTESIAN_POINT('Ctrl Pts',(-0.146256365994585,0.0867220621721572,
0.4));
#31123=CARTESIAN_POINT('Ctrl Pts',(-0.141169509830996,0.0935760956885117,
0.4));
#31124=CARTESIAN_POINT('Ctrl Pts',(-0.135561760713222,0.100014759881837,
0.4));
#31125=CARTESIAN_POINT('Ctrl Pts',(-0.129436334451722,0.105951160758884,
0.4));
#31126=CARTESIAN_POINT('Ctrl Pts',(-0.128680208499678,0.106683953314577,
0.4));
#31127=CARTESIAN_POINT('Ctrl Pts',(-0.127916183191217,0.107409072087309,
0.4));
#31128=CARTESIAN_POINT('Ctrl Pts',(-0.127144402274346,0.108126457236474,
0.4));
#31129=CARTESIAN_POINT('Origin',(0.,0.,0.4));
#31130=CARTESIAN_POINT('',(0.202072594216369,-0.35,0.4));
#31131=CARTESIAN_POINT('',(0.404145188432738,0.,0.4));
#31132=CARTESIAN_POINT('',(0.202072594216369,-0.35,0.4));
#31133=CARTESIAN_POINT('',(0.202072594216369,0.35,0.4));
#31134=CARTESIAN_POINT('',(0.404145188432738,0.,0.4));
#31135=CARTESIAN_POINT('',(-0.202072594216369,0.35,0.4));
#31136=CARTESIAN_POINT('',(0.202072594216369,0.35,0.4));
#31137=CARTESIAN_POINT('',(-0.404145188432738,5.55111512312578E-17,0.4));
#31138=CARTESIAN_POINT('',(-0.202072594216369,0.35,0.4));
#31139=CARTESIAN_POINT('',(-0.202072594216369,-0.35,0.4));
#31140=CARTESIAN_POINT('',(-0.404145188432738,4.94935111404957E-17,0.4));
#31141=CARTESIAN_POINT('',(-0.202072594216369,-0.35,0.4));
#31142=CARTESIAN_POINT('Origin',(-0.202072594216369,-0.35,0.));
#31143=CARTESIAN_POINT('',(-0.202072594216369,-0.35,0.));
#31144=CARTESIAN_POINT('',(0.202072594216369,-0.35,0.));
#31145=CARTESIAN_POINT('',(-0.202072594216369,-0.35,0.));
#31146=CARTESIAN_POINT('',(0.202072594216369,-0.35,0.));
#31147=CARTESIAN_POINT('',(-0.202072594216369,-0.35,0.));
#31148=CARTESIAN_POINT('Origin',(-0.404145188432738,4.94935111404957E-17,
0.));
#31149=CARTESIAN_POINT('',(-0.404145188432738,4.94935111404957E-17,0.));
#31150=CARTESIAN_POINT('',(-0.404145188432738,4.94935111404957E-17,0.));
#31151=CARTESIAN_POINT('',(-0.404145188432738,4.94935111404957E-17,0.));
#31152=CARTESIAN_POINT('Origin',(-0.202072594216369,0.35,0.));
#31153=CARTESIAN_POINT('',(-0.202072594216369,0.35,0.));
#31154=CARTESIAN_POINT('',(-0.202072594216369,0.35,0.));
#31155=CARTESIAN_POINT('',(-0.202072594216369,0.35,0.));
#31156=CARTESIAN_POINT('Origin',(0.202072594216369,0.35,0.));
#31157=CARTESIAN_POINT('',(0.202072594216369,0.35,0.));
#31158=CARTESIAN_POINT('',(0.202072594216369,0.35,0.));
#31159=CARTESIAN_POINT('',(0.202072594216369,0.35,0.));
#31160=CARTESIAN_POINT('Origin',(0.404145188432738,0.,0.));
#31161=CARTESIAN_POINT('',(0.404145188432738,0.,0.));
#31162=CARTESIAN_POINT('',(0.404145188432738,0.,0.));
#31163=CARTESIAN_POINT('',(0.404145188432738,0.,0.));
#31164=CARTESIAN_POINT('Origin',(0.202072594216369,-0.35,0.));
#31165=CARTESIAN_POINT('',(0.202072594216369,-0.35,0.));
#31166=CARTESIAN_POINT('Origin',(0.,0.,0.));
#31167=CARTESIAN_POINT('',(0.,0.,0.));
#31168=CARTESIAN_POINT('Origin',(0.,51.,60.));
#31169=CARTESIAN_POINT('',(0.,51.,60.41));
#31170=CARTESIAN_POINT('Origin',(0.,51.,60.));
#31171=CARTESIAN_POINT('',(1.5,51.,60.41));
#31172=CARTESIAN_POINT('',(0.,51.,60.41));
#31173=CARTESIAN_POINT('Origin',(1.5,51.,60.));
#31174=CARTESIAN_POINT('Origin',(1.5,51.,60.));
#31175=CARTESIAN_POINT('Origin',(0.,9.,120.));
#31176=CARTESIAN_POINT('',(0.,9.,120.41));
#31177=CARTESIAN_POINT('Origin',(0.,9.,120.));
#31178=CARTESIAN_POINT('',(1.5,9.,120.41));
#31179=CARTESIAN_POINT('',(0.,9.,120.41));
#31180=CARTESIAN_POINT('Origin',(1.5,9.,120.));
#31181=CARTESIAN_POINT('Origin',(1.5,9.,120.));
#31182=CARTESIAN_POINT('Origin',(0.,9.,60.));
#31183=CARTESIAN_POINT('',(0.,9.,60.41));
#31184=CARTESIAN_POINT('Origin',(0.,9.,60.));
#31185=CARTESIAN_POINT('',(1.5,9.,60.41));
#31186=CARTESIAN_POINT('',(0.,9.,60.41));
#31187=CARTESIAN_POINT('Origin',(1.5,9.,60.));
#31188=CARTESIAN_POINT('Origin',(1.5,9.,60.));
#31189=CARTESIAN_POINT('Origin',(0.,51.,120.));
#31190=CARTESIAN_POINT('',(0.,51.,120.41));
#31191=CARTESIAN_POINT('Origin',(0.,51.,120.));
#31192=CARTESIAN_POINT('',(1.5,51.,120.41));
#31193=CARTESIAN_POINT('',(0.,51.,120.41));
#31194=CARTESIAN_POINT('Origin',(1.5,51.,120.));
#31195=CARTESIAN_POINT('Origin',(1.5,51.,120.));
#31196=CARTESIAN_POINT('Origin',(1.81,58.82,0.));
#31197=CARTESIAN_POINT('',(1.3,58.82,134.08));
#31198=CARTESIAN_POINT('',(1.8,58.82,134.08));
#31199=CARTESIAN_POINT('',(1.6825,58.82,134.08));
#31200=CARTESIAN_POINT('',(1.3,58.82,90.92));
#31201=CARTESIAN_POINT('',(1.3,58.82,0.));
#31202=CARTESIAN_POINT('',(1.8,58.82,90.92));
#31203=CARTESIAN_POINT('',(1.6825,58.82,90.92));
#31204=CARTESIAN_POINT('',(1.8,58.82,0.));
#31205=CARTESIAN_POINT('Origin',(1.81,58.82,0.));
#31206=CARTESIAN_POINT('',(1.3,58.82,89.08));
#31207=CARTESIAN_POINT('',(1.8,58.82,89.08));
#31208=CARTESIAN_POINT('',(1.6825,58.82,89.08));
#31209=CARTESIAN_POINT('',(1.3,58.82,45.92));
#31210=CARTESIAN_POINT('',(1.3,58.82,0.));
#31211=CARTESIAN_POINT('',(1.8,58.82,45.92));
#31212=CARTESIAN_POINT('',(1.6825,58.82,45.92));
#31213=CARTESIAN_POINT('',(1.8,58.82,0.));
#31214=CARTESIAN_POINT('Origin',(1.81,58.82,0.));
#31215=CARTESIAN_POINT('',(1.3,58.82,44.08));
#31216=CARTESIAN_POINT('',(1.8,58.82,44.08));
#31217=CARTESIAN_POINT('',(1.6825,58.82,44.08));
#31218=CARTESIAN_POINT('',(1.3,58.82,1.82));
#31219=CARTESIAN_POINT('',(1.3,58.82,0.));
#31220=CARTESIAN_POINT('',(1.8,58.82,1.82));
#31221=CARTESIAN_POINT('',(1.6825,58.82,1.82));
#31222=CARTESIAN_POINT('',(1.8,58.82,0.));
#31223=CARTESIAN_POINT('Origin',(1.81,58.82,0.));
#31224=CARTESIAN_POINT('',(1.3,58.82,178.18));
#31225=CARTESIAN_POINT('',(1.8,58.82,178.18));
#31226=CARTESIAN_POINT('',(1.6825,58.82,178.18));
#31227=CARTESIAN_POINT('',(1.3,58.82,135.92));
#31228=CARTESIAN_POINT('',(1.3,58.82,0.));
#31229=CARTESIAN_POINT('',(1.8,58.82,135.92));
#31230=CARTESIAN_POINT('',(1.6825,58.82,135.92));
#31231=CARTESIAN_POINT('',(1.8,58.82,0.));
#31232=CARTESIAN_POINT('Origin',(1.3,58.18,0.));
#31233=CARTESIAN_POINT('',(1.8,58.18,44.08));
#31234=CARTESIAN_POINT('',(1.3,58.18,44.08));
#31235=CARTESIAN_POINT('',(1.4275,58.18,44.08));
#31236=CARTESIAN_POINT('',(1.8,58.18,1.82));
#31237=CARTESIAN_POINT('',(1.8,58.18,0.));
#31238=CARTESIAN_POINT('',(1.3,58.18,1.82));
#31239=CARTESIAN_POINT('',(1.4275,58.18,1.82));
#31240=CARTESIAN_POINT('',(1.3,58.18,0.));
#31241=CARTESIAN_POINT('Origin',(1.3,58.18,0.));
#31242=CARTESIAN_POINT('',(1.8,58.18,89.08));
#31243=CARTESIAN_POINT('',(1.3,58.18,89.08));
#31244=CARTESIAN_POINT('',(1.4275,58.18,89.08));
#31245=CARTESIAN_POINT('',(1.8,58.18,45.92));
#31246=CARTESIAN_POINT('',(1.8,58.18,0.));
#31247=CARTESIAN_POINT('',(1.3,58.18,45.92));
#31248=CARTESIAN_POINT('',(1.4275,58.18,45.92));
#31249=CARTESIAN_POINT('',(1.3,58.18,0.));
#31250=CARTESIAN_POINT('Origin',(1.3,58.18,0.));
#31251=CARTESIAN_POINT('',(1.8,58.18,134.08));
#31252=CARTESIAN_POINT('',(1.3,58.18,134.08));
#31253=CARTESIAN_POINT('',(1.4275,58.18,134.08));
#31254=CARTESIAN_POINT('',(1.8,58.18,90.92));
#31255=CARTESIAN_POINT('',(1.8,58.18,0.));
#31256=CARTESIAN_POINT('',(1.3,58.18,90.92));
#31257=CARTESIAN_POINT('',(1.4275,58.18,90.92));
#31258=CARTESIAN_POINT('',(1.3,58.18,0.));
#31259=CARTESIAN_POINT('Origin',(1.3,58.18,0.));
#31260=CARTESIAN_POINT('',(1.8,58.18,178.18));
#31261=CARTESIAN_POINT('',(1.3,58.18,178.18));
#31262=CARTESIAN_POINT('',(1.4275,58.18,178.18));
#31263=CARTESIAN_POINT('',(1.8,58.18,135.92));
#31264=CARTESIAN_POINT('',(1.8,58.18,0.));
#31265=CARTESIAN_POINT('',(1.3,58.18,135.92));
#31266=CARTESIAN_POINT('',(1.4275,58.18,135.92));
#31267=CARTESIAN_POINT('',(1.3,58.18,0.));
#31268=CARTESIAN_POINT('Origin',(1.3,60.,178.18));
#31269=CARTESIAN_POINT('',(1.3,60.,178.18));
#31270=CARTESIAN_POINT('',(1.3,60.,178.18));
#31271=CARTESIAN_POINT('',(1.3,60.,180.));
#31272=CARTESIAN_POINT('',(1.3,60.,89.09));
#31273=CARTESIAN_POINT('',(1.3,0.,180.));
#31274=CARTESIAN_POINT('',(1.3,45.,180.));
#31275=CARTESIAN_POINT('',(1.3,0.,178.18));
#31276=CARTESIAN_POINT('',(1.3,0.,89.09));
#31277=CARTESIAN_POINT('',(1.3,60.,178.18));
#31278=CARTESIAN_POINT('',(1.3,0.,135.92));
#31279=CARTESIAN_POINT('',(1.3,60.,135.92));
#31280=CARTESIAN_POINT('',(1.3,0.,134.08));
#31281=CARTESIAN_POINT('',(1.3,0.,67.04));
#31282=CARTESIAN_POINT('',(1.3,60.,134.08));
#31283=CARTESIAN_POINT('',(1.3,0.,90.92));
#31284=CARTESIAN_POINT('',(1.3,60.,90.92));
#31285=CARTESIAN_POINT('',(1.3,0.,89.08));
#31286=CARTESIAN_POINT('',(1.3,0.,44.54));
#31287=CARTESIAN_POINT('',(1.3,60.,89.08));
#31288=CARTESIAN_POINT('',(1.3,0.,45.92));
#31289=CARTESIAN_POINT('',(1.3,60.,45.92));
#31290=CARTESIAN_POINT('',(1.3,0.,44.08));
#31291=CARTESIAN_POINT('',(1.3,0.,22.04));
#31292=CARTESIAN_POINT('',(1.3,60.,44.08));
#31293=CARTESIAN_POINT('',(1.3,0.,1.82));
#31294=CARTESIAN_POINT('',(1.3,60.,1.82));
#31295=CARTESIAN_POINT('',(1.3,0.,0.));
#31296=CARTESIAN_POINT('',(1.3,0.,0.));
#31297=CARTESIAN_POINT('',(1.3,60.,0.));
#31298=CARTESIAN_POINT('',(1.3,45.,0.));
#31299=CARTESIAN_POINT('',(1.3,60.,1.82));
#31300=CARTESIAN_POINT('',(1.3,60.,0.));
#31301=CARTESIAN_POINT('',(1.3,60.,1.82));
#31302=CARTESIAN_POINT('',(1.3,60.,44.08));
#31303=CARTESIAN_POINT('',(1.3,60.,44.08));
#31304=CARTESIAN_POINT('',(1.3,60.,45.92));
#31305=CARTESIAN_POINT('',(1.3,60.,22.04));
#31306=CARTESIAN_POINT('',(1.3,60.,45.92));
#31307=CARTESIAN_POINT('',(1.3,60.,89.08));
#31308=CARTESIAN_POINT('',(1.3,60.,89.08));
#31309=CARTESIAN_POINT('',(1.3,60.,90.92));
#31310=CARTESIAN_POINT('',(1.3,60.,44.54));
#31311=CARTESIAN_POINT('',(1.3,60.,90.92));
#31312=CARTESIAN_POINT('',(1.3,60.,134.08));
#31313=CARTESIAN_POINT('',(1.3,60.,134.08));
#31314=CARTESIAN_POINT('',(1.3,60.,135.92));
#31315=CARTESIAN_POINT('',(1.3,60.,67.04));
#31316=CARTESIAN_POINT('',(1.3,60.,135.92));
#31317=CARTESIAN_POINT('Origin',(1.555,30.,178.18));
#31318=CARTESIAN_POINT('',(1.8,0.,178.18));
#31319=CARTESIAN_POINT('',(0.7775,0.,178.18));
#31320=CARTESIAN_POINT('',(1.8,15.,178.18));
#31321=CARTESIAN_POINT('Origin',(1.555,30.,178.18));
#31322=CARTESIAN_POINT('',(1.8,60.,178.18));
#31323=CARTESIAN_POINT('',(1.8,15.,178.18));
#31324=CARTESIAN_POINT('',(1.6775,60.,178.18));
#31325=CARTESIAN_POINT('Origin',(1.8,0.,0.));
#31326=CARTESIAN_POINT('',(1.8,0.,135.92));
#31327=CARTESIAN_POINT('',(1.8,0.,0.));
#31328=CARTESIAN_POINT('',(1.8,15.,135.92));
#31329=CARTESIAN_POINT('Origin',(1.8,0.,0.));
#31330=CARTESIAN_POINT('',(1.8,60.,135.92));
#31331=CARTESIAN_POINT('',(1.8,15.,135.92));
#31332=CARTESIAN_POINT('',(1.8,60.,0.));
#31333=CARTESIAN_POINT('Origin',(1.555,30.,135.92));
#31334=CARTESIAN_POINT('',(0.7775,0.,135.92));
#31335=CARTESIAN_POINT('Origin',(1.555,30.,135.92));
#31336=CARTESIAN_POINT('',(1.6775,60.,135.92));
#31337=CARTESIAN_POINT('Origin',(1.555,30.,134.08));
#31338=CARTESIAN_POINT('',(1.8,0.,134.08));
#31339=CARTESIAN_POINT('',(0.7775,0.,134.08));
#31340=CARTESIAN_POINT('',(1.8,15.,134.08));
#31341=CARTESIAN_POINT('Origin',(1.555,30.,134.08));
#31342=CARTESIAN_POINT('',(1.8,60.,134.08));
#31343=CARTESIAN_POINT('',(1.8,15.,134.08));
#31344=CARTESIAN_POINT('',(1.6775,60.,134.08));
#31345=CARTESIAN_POINT('Origin',(1.8,0.,0.));
#31346=CARTESIAN_POINT('',(1.8,0.,90.92));
#31347=CARTESIAN_POINT('',(1.8,0.,0.));
#31348=CARTESIAN_POINT('',(1.8,15.,90.92));
#31349=CARTESIAN_POINT('Origin',(1.8,0.,0.));
#31350=CARTESIAN_POINT('',(1.8,60.,90.92));
#31351=CARTESIAN_POINT('',(1.8,15.,90.92));
#31352=CARTESIAN_POINT('',(1.8,60.,0.));
#31353=CARTESIAN_POINT('Origin',(1.555,30.,90.92));
#31354=CARTESIAN_POINT('',(0.7775,0.,90.92));
#31355=CARTESIAN_POINT('Origin',(1.555,30.,90.92));
#31356=CARTESIAN_POINT('',(1.6775,60.,90.92));
#31357=CARTESIAN_POINT('Origin',(1.555,30.,89.08));
#31358=CARTESIAN_POINT('',(1.8,0.,89.08));
#31359=CARTESIAN_POINT('',(0.7775,0.,89.08));
#31360=CARTESIAN_POINT('',(1.8,15.,89.08));
#31361=CARTESIAN_POINT('Origin',(1.555,30.,89.08));
#31362=CARTESIAN_POINT('',(1.8,60.,89.08));
#31363=CARTESIAN_POINT('',(1.8,15.,89.08));
#31364=CARTESIAN_POINT('',(1.6775,60.,89.08));
#31365=CARTESIAN_POINT('Origin',(1.8,0.,0.));
#31366=CARTESIAN_POINT('',(1.8,0.,45.92));
#31367=CARTESIAN_POINT('',(1.8,0.,0.));
#31368=CARTESIAN_POINT('',(1.8,15.,45.92));
#31369=CARTESIAN_POINT('Origin',(1.8,0.,0.));
#31370=CARTESIAN_POINT('',(1.8,60.,45.92));
#31371=CARTESIAN_POINT('',(1.8,15.,45.92));
#31372=CARTESIAN_POINT('',(1.8,60.,0.));
#31373=CARTESIAN_POINT('Origin',(1.555,30.,45.92));
#31374=CARTESIAN_POINT('',(0.7775,0.,45.92));
#31375=CARTESIAN_POINT('Origin',(1.555,30.,45.92));
#31376=CARTESIAN_POINT('',(1.6775,60.,45.92));
#31377=CARTESIAN_POINT('Origin',(1.555,30.,44.08));
#31378=CARTESIAN_POINT('',(1.8,0.,44.08));
#31379=CARTESIAN_POINT('',(0.7775,0.,44.08));
#31380=CARTESIAN_POINT('',(1.8,15.,44.08));
#31381=CARTESIAN_POINT('Origin',(1.555,30.,44.08));
#31382=CARTESIAN_POINT('',(1.8,60.,44.08));
#31383=CARTESIAN_POINT('',(1.8,15.,44.08));
#31384=CARTESIAN_POINT('',(1.6775,60.,44.08));
#31385=CARTESIAN_POINT('Origin',(1.8,0.,0.));
#31386=CARTESIAN_POINT('',(1.8,0.,1.82));
#31387=CARTESIAN_POINT('',(1.8,0.,0.));
#31388=CARTESIAN_POINT('',(1.8,15.,1.82));
#31389=CARTESIAN_POINT('Origin',(1.8,0.,0.));
#31390=CARTESIAN_POINT('',(1.8,60.,1.82));
#31391=CARTESIAN_POINT('',(1.8,15.,1.82));
#31392=CARTESIAN_POINT('',(1.8,60.,0.));
#31393=CARTESIAN_POINT('Origin',(1.555,30.,1.82));
#31394=CARTESIAN_POINT('',(0.7775,0.,1.82));
#31395=CARTESIAN_POINT('Origin',(1.555,30.,1.82));
#31396=CARTESIAN_POINT('',(1.6775,60.,1.82));
#31397=CARTESIAN_POINT('Origin',(1.8,60.,0.));
#31398=CARTESIAN_POINT('',(0.,60.,0.));
#31399=CARTESIAN_POINT('',(1.8,60.,0.));
#31400=CARTESIAN_POINT('',(0.,60.,180.));
#31401=CARTESIAN_POINT('',(0.,60.,0.));
#31402=CARTESIAN_POINT('',(1.8,60.,180.));
#31403=CARTESIAN_POINT('Origin',(0.9,30.,0.));
#31404=CARTESIAN_POINT('',(0.,0.,0.));
#31405=CARTESIAN_POINT('',(0.,0.,0.));
#31406=CARTESIAN_POINT('',(0.,60.,0.));
#31407=CARTESIAN_POINT('Origin',(0.,0.,0.));
#31408=CARTESIAN_POINT('',(0.,0.,180.));
#31409=CARTESIAN_POINT('',(0.,0.,180.));
#31410=CARTESIAN_POINT('',(0.,0.,0.));
#31411=CARTESIAN_POINT('Origin',(0.,60.,0.));
#31412=CARTESIAN_POINT('',(0.,60.,180.));
#31413=CARTESIAN_POINT('Origin',(0.9,30.,180.));
#31414=CARTESIAN_POINT('',(0.,0.,0.));
#31415=CARTESIAN_POINT('Origin',(0.,58.18,1.3));
#31416=CARTESIAN_POINT('',(57.36,58.18,1.8));
#31417=CARTESIAN_POINT('',(0.,58.18,1.8));
#31418=CARTESIAN_POINT('',(14.34,58.18,1.8));
#31419=CARTESIAN_POINT('',(57.36,58.18,1.3));
#31420=CARTESIAN_POINT('',(57.36,58.18,0.65));
#31421=CARTESIAN_POINT('',(0.,58.18,1.3));
#31422=CARTESIAN_POINT('',(0.,58.18,1.3));
#31423=CARTESIAN_POINT('',(0.,58.18,0.65));
#31424=CARTESIAN_POINT('Origin',(57.36,58.82,1.3));
#31425=CARTESIAN_POINT('',(0.,58.82,1.8));
#31426=CARTESIAN_POINT('',(57.36,58.82,1.8));
#31427=CARTESIAN_POINT('',(43.02,58.82,1.8));
#31428=CARTESIAN_POINT('',(0.,58.82,1.3));
#31429=CARTESIAN_POINT('',(0.,58.82,0.65));
#31430=CARTESIAN_POINT('',(57.36,58.82,1.3));
#31431=CARTESIAN_POINT('',(57.36,58.82,1.3));
#31432=CARTESIAN_POINT('',(57.36,58.82,0.65));
#31433=CARTESIAN_POINT('Origin',(28.68,58.5,1.3));
#31434=CARTESIAN_POINT('',(0.,59.25,1.3));
#31435=CARTESIAN_POINT('',(57.36,29.25,1.3));
#31436=CARTESIAN_POINT('Origin',(57.36,0.,0.));
#31437=CARTESIAN_POINT('',(57.36,0.,1.8));
#31438=CARTESIAN_POINT('',(57.36,0.,1.8));
#31439=CARTESIAN_POINT('',(57.36,0.,0.));
#31440=CARTESIAN_POINT('',(57.36,0.,0.));
#31441=CARTESIAN_POINT('',(57.36,60.,0.));
#31442=CARTESIAN_POINT('',(57.36,0.,0.));
#31443=CARTESIAN_POINT('',(57.36,60.,1.8));
#31444=CARTESIAN_POINT('',(57.36,60.,0.));
#31445=CARTESIAN_POINT('',(57.36,0.,1.8));
#31446=CARTESIAN_POINT('Origin',(28.68,30.,1.8));
#31447=CARTESIAN_POINT('',(0.,0.,1.8));
#31448=CARTESIAN_POINT('',(0.,60.,1.8));
#31449=CARTESIAN_POINT('',(0.,0.,1.8));
#31450=CARTESIAN_POINT('Origin',(57.36,60.,0.));
#31451=CARTESIAN_POINT('',(0.,60.,0.));
#31452=CARTESIAN_POINT('',(57.36,60.,0.));
#31453=CARTESIAN_POINT('',(0.,60.,1.8));
#31454=CARTESIAN_POINT('',(0.,60.,0.));
#31455=CARTESIAN_POINT('',(57.36,60.,1.8));
#31456=CARTESIAN_POINT('Origin',(0.,0.,0.));
#31457=CARTESIAN_POINT('',(0.,0.,0.));
#31458=CARTESIAN_POINT('',(0.,0.,0.));
#31459=CARTESIAN_POINT('',(0.,0.,0.));
#31460=CARTESIAN_POINT('Origin',(0.,60.,0.));
#31461=CARTESIAN_POINT('',(0.,60.,1.8));
#31462=CARTESIAN_POINT('',(0.,60.,0.));
#31463=CARTESIAN_POINT('Origin',(28.68,30.,1.8));
#31464=CARTESIAN_POINT('Origin',(28.68,30.,0.));
#31465=CARTESIAN_POINT('',(0.,0.,0.));
#31466=CARTESIAN_POINT('Origin',(57.36,57.6,0.));
#31467=CARTESIAN_POINT('',(57.36,57.6,0.));
#31468=CARTESIAN_POINT('',(0.,57.6,0.));
#31469=CARTESIAN_POINT('',(57.36,57.6,0.));
#31470=CARTESIAN_POINT('',(0.,57.6,1.8));
#31471=CARTESIAN_POINT('',(0.,57.6,0.));
#31472=CARTESIAN_POINT('',(57.36,57.6,1.8));
#31473=CARTESIAN_POINT('',(57.36,57.6,1.8));
#31474=CARTESIAN_POINT('',(57.36,57.6,0.));
#31475=CARTESIAN_POINT('Origin',(57.36,0.6,0.));
#31476=CARTESIAN_POINT('',(57.36,0.6,0.));
#31477=CARTESIAN_POINT('',(57.36,0.6,0.));
#31478=CARTESIAN_POINT('',(57.36,0.600000000000001,1.8));
#31479=CARTESIAN_POINT('',(57.36,0.6,1.8));
#31480=CARTESIAN_POINT('',(57.36,0.6,0.));
#31481=CARTESIAN_POINT('Origin',(0.,0.6,0.));
#31482=CARTESIAN_POINT('',(0.,0.600000000000001,0.));
#31483=CARTESIAN_POINT('',(0.,0.6,0.));
#31484=CARTESIAN_POINT('',(0.,0.600000000000001,1.8));
#31485=CARTESIAN_POINT('',(0.,0.6,1.8));
#31486=CARTESIAN_POINT('',(0.,0.600000000000001,0.));
#31487=CARTESIAN_POINT('Origin',(0.,57.6,0.));
#31488=CARTESIAN_POINT('',(0.,57.6,0.));
#31489=CARTESIAN_POINT('',(0.,57.6,1.8));
#31490=CARTESIAN_POINT('Origin',(28.68,29.1,1.8));
#31491=CARTESIAN_POINT('Origin',(28.68,29.1,0.));
#31492=CARTESIAN_POINT('',(0.,0.,0.));
#31493=CARTESIAN_POINT('Origin',(0.,0.,0.));
#31494=CARTESIAN_POINT('',(-0.4,-4.89858719658941E-17,2.8));
#31495=CARTESIAN_POINT('Origin',(0.,0.,2.8));
#31496=CARTESIAN_POINT('',(-0.4,-4.89858719658941E-17,0.));
#31497=CARTESIAN_POINT('',(-0.4,-4.89858719658941E-17,0.));
#31498=CARTESIAN_POINT('Origin',(0.,0.,0.));
#31499=CARTESIAN_POINT('Origin',(0.,0.,2.8));
#31500=CARTESIAN_POINT('Origin',(0.,0.,0.));
#31501=CARTESIAN_POINT('',(0.,0.,0.));
#31502=CARTESIAN_POINT('',(1.32,0.,0.));
#31503=CARTESIAN_POINT('',(1.32,58.2,1.32));
#31504=CARTESIAN_POINT('',(1.32,0.,44.1));
#31505=CARTESIAN_POINT('',(0.,0.,0.));
#31506=CARTESIAN_POINT('',(1.8,-0.4,5.));
#31507=CARTESIAN_POINT('',(1.8,-0.4,5.));
#31508=CARTESIAN_POINT('',(1.8,-0.4,5.));
#31509=CARTESIAN_POINT('',(2.,1.6,60.));
#31510=CARTESIAN_POINT('',(0.,1.6,60.));
#31511=CARTESIAN_POINT('',(80.,0.,0.));
#31512=CARTESIAN_POINT('',(81.32,0.,0.));
#31513=CARTESIAN_POINT('',(81.32,58.2,1.32));
#31514=CARTESIAN_POINT('',(81.32,0.,44.1));
#31515=CARTESIAN_POINT('',(78.6,9.,60.));
#31516=CARTESIAN_POINT('',(80.,0.,180.));
#31517=CARTESIAN_POINT('',(78.68,0.,180.));
#31518=CARTESIAN_POINT('',(1.32,0.,89.1));
#31519=CARTESIAN_POINT('',(1.32,0.,134.1));
#31520=CARTESIAN_POINT('',(3.4,1.77635683940025E-15,60.));
#31521=CARTESIAN_POINT('',(3.4,-2.,60.));
#31522=CARTESIAN_POINT('',(2.,1.6,120.));
#31523=CARTESIAN_POINT('',(0.,1.6,120.));
#31524=CARTESIAN_POINT('',(3.4,2.22044604925031E-15,120.));
#31525=CARTESIAN_POINT('',(3.4,-2.,120.));
#31526=CARTESIAN_POINT('',(140.,0.,180.));
#31527=CARTESIAN_POINT('',(138.68,0.,180.));
#31528=CARTESIAN_POINT('',(81.32,0.,89.1));
#31529=CARTESIAN_POINT('',(81.32,0.,134.1));
#31530=CARTESIAN_POINT('',(78.6,9.,120.));
#31531=CARTESIAN_POINT('',(78.6,51.,60.));
#31532=CARTESIAN_POINT('',(78.6,51.,120.));
#31533=UNCERTAINTY_MEASURE_WITH_UNIT(LENGTH_MEASURE(0.001),#31567,
'DISTANCE_ACCURACY_VALUE',
'Maximum model space distance between geometric entities at asserted c
onnectivities');
#31534=UNCERTAINTY_MEASURE_WITH_UNIT(LENGTH_MEASURE(0.001),#31567,
'DISTANCE_ACCURACY_VALUE',
'Maximum model space distance between geometric entities at asserted c
onnectivities');
#31535=UNCERTAINTY_MEASURE_WITH_UNIT(LENGTH_MEASURE(0.001),#31567,
'DISTANCE_ACCURACY_VALUE',
'Maximum model space distance between geometric entities at asserted c
onnectivities');
#31536=UNCERTAINTY_MEASURE_WITH_UNIT(LENGTH_MEASURE(0.001),#31567,
'DISTANCE_ACCURACY_VALUE',
'Maximum model space distance between geometric entities at asserted c
onnectivities');
#31537=UNCERTAINTY_MEASURE_WITH_UNIT(LENGTH_MEASURE(0.001),#31567,
'DISTANCE_ACCURACY_VALUE',
'Maximum model space distance between geometric entities at asserted c
onnectivities');
#31538=UNCERTAINTY_MEASURE_WITH_UNIT(LENGTH_MEASURE(0.001),#31567,
'DISTANCE_ACCURACY_VALUE',
'Maximum model space distance between geometric entities at asserted c
onnectivities');
#31539=UNCERTAINTY_MEASURE_WITH_UNIT(LENGTH_MEASURE(0.001),#31567,
'DISTANCE_ACCURACY_VALUE',
'Maximum model space distance between geometric entities at asserted c
onnectivities');
#31540=UNCERTAINTY_MEASURE_WITH_UNIT(LENGTH_MEASURE(0.001),#31567,
'DISTANCE_ACCURACY_VALUE',
'Maximum model space distance between geometric entities at asserted c
onnectivities');
#31541=UNCERTAINTY_MEASURE_WITH_UNIT(LENGTH_MEASURE(0.001),#31567,
'DISTANCE_ACCURACY_VALUE',
'Maximum model space distance between geometric entities at asserted c
onnectivities');
#31542=UNCERTAINTY_MEASURE_WITH_UNIT(LENGTH_MEASURE(0.001),#31567,
'DISTANCE_ACCURACY_VALUE',
'Maximum model space distance between geometric entities at asserted c
onnectivities');
#31543=UNCERTAINTY_MEASURE_WITH_UNIT(LENGTH_MEASURE(0.001),#31567,
'DISTANCE_ACCURACY_VALUE',
'Maximum model space distance between geometric entities at asserted c
onnectivities');
#31544=UNCERTAINTY_MEASURE_WITH_UNIT(LENGTH_MEASURE(0.001),#31567,
'DISTANCE_ACCURACY_VALUE',
'Maximum model space distance between geometric entities at asserted c
onnectivities');
#31545=UNCERTAINTY_MEASURE_WITH_UNIT(LENGTH_MEASURE(0.001),#31567,
'DISTANCE_ACCURACY_VALUE',
'Maximum model space distance between geometric entities at asserted c
onnectivities');
#31546=UNCERTAINTY_MEASURE_WITH_UNIT(LENGTH_MEASURE(0.001),#31567,
'DISTANCE_ACCURACY_VALUE',
'Maximum model space distance between geometric entities at asserted c
onnectivities');
#31547=UNCERTAINTY_MEASURE_WITH_UNIT(LENGTH_MEASURE(0.001),#31567,
'DISTANCE_ACCURACY_VALUE',
'Maximum model space distance between geometric entities at asserted c
onnectivities');
#31548=UNCERTAINTY_MEASURE_WITH_UNIT(LENGTH_MEASURE(0.001),#31567,
'DISTANCE_ACCURACY_VALUE',
'Maximum model space distance between geometric entities at asserted c
onnectivities');
#31549=UNCERTAINTY_MEASURE_WITH_UNIT(LENGTH_MEASURE(0.001),#31567,
'DISTANCE_ACCURACY_VALUE',
'Maximum model space distance between geometric entities at asserted c
onnectivities');
#31550=(
GEOMETRIC_REPRESENTATION_CONTEXT(3)
GLOBAL_UNCERTAINTY_ASSIGNED_CONTEXT((#31533))
GLOBAL_UNIT_ASSIGNED_CONTEXT((#31567,#31569,#31570))
REPRESENTATION_CONTEXT('','3D')
);
#31551=(
GEOMETRIC_REPRESENTATION_CONTEXT(3)
GLOBAL_UNCERTAINTY_ASSIGNED_CONTEXT((#31534))
GLOBAL_UNIT_ASSIGNED_CONTEXT((#31567,#31569,#31570))
REPRESENTATION_CONTEXT('','3D')
);
#31552=(
GEOMETRIC_REPRESENTATION_CONTEXT(3)
GLOBAL_UNCERTAINTY_ASSIGNED_CONTEXT((#31535))
GLOBAL_UNIT_ASSIGNED_CONTEXT((#31567,#31569,#31570))
REPRESENTATION_CONTEXT('','3D')
);
#31553=(
GEOMETRIC_REPRESENTATION_CONTEXT(3)
GLOBAL_UNCERTAINTY_ASSIGNED_CONTEXT((#31536))
GLOBAL_UNIT_ASSIGNED_CONTEXT((#31567,#31569,#31570))
REPRESENTATION_CONTEXT('','3D')
);
#31554=(
GEOMETRIC_REPRESENTATION_CONTEXT(3)
GLOBAL_UNCERTAINTY_ASSIGNED_CONTEXT((#31537))
GLOBAL_UNIT_ASSIGNED_CONTEXT((#31567,#31569,#31570))
REPRESENTATION_CONTEXT('','3D')
);
#31555=(
GEOMETRIC_REPRESENTATION_CONTEXT(3)
GLOBAL_UNCERTAINTY_ASSIGNED_CONTEXT((#31538))
GLOBAL_UNIT_ASSIGNED_CONTEXT((#31567,#31569,#31570))
REPRESENTATION_CONTEXT('','3D')
);
#31556=(
GEOMETRIC_REPRESENTATION_CONTEXT(3)
GLOBAL_UNCERTAINTY_ASSIGNED_CONTEXT((#31539))
GLOBAL_UNIT_ASSIGNED_CONTEXT((#31567,#31569,#31570))
REPRESENTATION_CONTEXT('','3D')
);
#31557=(
GEOMETRIC_REPRESENTATION_CONTEXT(3)
GLOBAL_UNCERTAINTY_ASSIGNED_CONTEXT((#31540))
GLOBAL_UNIT_ASSIGNED_CONTEXT((#31567,#31569,#31570))
REPRESENTATION_CONTEXT('','3D')
);
#31558=(
GEOMETRIC_REPRESENTATION_CONTEXT(3)
GLOBAL_UNCERTAINTY_ASSIGNED_CONTEXT((#31541))
GLOBAL_UNIT_ASSIGNED_CONTEXT((#31567,#31569,#31570))
REPRESENTATION_CONTEXT('','3D')
);
#31559=(
GEOMETRIC_REPRESENTATION_CONTEXT(3)
GLOBAL_UNCERTAINTY_ASSIGNED_CONTEXT((#31542))
GLOBAL_UNIT_ASSIGNED_CONTEXT((#31567,#31569,#31570))
REPRESENTATION_CONTEXT('','3D')
);
#31560=(
GEOMETRIC_REPRESENTATION_CONTEXT(3)
GLOBAL_UNCERTAINTY_ASSIGNED_CONTEXT((#31543))
GLOBAL_UNIT_ASSIGNED_CONTEXT((#31567,#31569,#31570))
REPRESENTATION_CONTEXT('','3D')
);
#31561=(
GEOMETRIC_REPRESENTATION_CONTEXT(3)
GLOBAL_UNCERTAINTY_ASSIGNED_CONTEXT((#31544))
GLOBAL_UNIT_ASSIGNED_CONTEXT((#31567,#31569,#31570))
REPRESENTATION_CONTEXT('','3D')
);
#31562=(
GEOMETRIC_REPRESENTATION_CONTEXT(3)
GLOBAL_UNCERTAINTY_ASSIGNED_CONTEXT((#31545))
GLOBAL_UNIT_ASSIGNED_CONTEXT((#31567,#31569,#31570))
REPRESENTATION_CONTEXT('','3D')
);
#31563=(
GEOMETRIC_REPRESENTATION_CONTEXT(3)
GLOBAL_UNCERTAINTY_ASSIGNED_CONTEXT((#31546))
GLOBAL_UNIT_ASSIGNED_CONTEXT((#31567,#31569,#31570))
REPRESENTATION_CONTEXT('','3D')
);
#31564=(
GEOMETRIC_REPRESENTATION_CONTEXT(3)
GLOBAL_UNCERTAINTY_ASSIGNED_CONTEXT((#31547))
GLOBAL_UNIT_ASSIGNED_CONTEXT((#31567,#31569,#31570))
REPRESENTATION_CONTEXT('','3D')
);
#31565=(
GEOMETRIC_REPRESENTATION_CONTEXT(3)
GLOBAL_UNCERTAINTY_ASSIGNED_CONTEXT((#31548))
GLOBAL_UNIT_ASSIGNED_CONTEXT((#31567,#31569,#31570))
REPRESENTATION_CONTEXT('','3D')
);
#31566=(
GEOMETRIC_REPRESENTATION_CONTEXT(3)
GLOBAL_UNCERTAINTY_ASSIGNED_CONTEXT((#31549))
GLOBAL_UNIT_ASSIGNED_CONTEXT((#31567,#31569,#31570))
REPRESENTATION_CONTEXT('','3D')
);
#31567=(
LENGTH_UNIT()
NAMED_UNIT(*)
SI_UNIT(.CENTI.,.METRE.)
);
#31568=(
LENGTH_UNIT()
NAMED_UNIT(*)
SI_UNIT($,.METRE.)
);
#31569=(
NAMED_UNIT(*)
PLANE_ANGLE_UNIT()
SI_UNIT($,.RADIAN.)
);
#31570=(
NAMED_UNIT(*)
SI_UNIT($,.STERADIAN.)
SOLID_ANGLE_UNIT()
);
#31571=SHAPE_DEFINITION_REPRESENTATION(#31587,#31635);
#31572=SHAPE_DEFINITION_REPRESENTATION(#31588,#31636);
#31573=SHAPE_DEFINITION_REPRESENTATION(#31589,#31637);
#31574=SHAPE_DEFINITION_REPRESENTATION(#31590,#31638);
#31575=SHAPE_DEFINITION_REPRESENTATION(#31591,#31639);
#31576=SHAPE_DEFINITION_REPRESENTATION(#31592,#31640);
#31577=SHAPE_DEFINITION_REPRESENTATION(#31593,#31641);
#31578=SHAPE_DEFINITION_REPRESENTATION(#31594,#31642);
#31579=SHAPE_DEFINITION_REPRESENTATION(#31595,#31643);
#31580=SHAPE_DEFINITION_REPRESENTATION(#31596,#31644);
#31581=SHAPE_DEFINITION_REPRESENTATION(#31597,#31645);
#31582=SHAPE_DEFINITION_REPRESENTATION(#31598,#31646);
#31583=SHAPE_DEFINITION_REPRESENTATION(#31599,#31647);
#31584=SHAPE_DEFINITION_REPRESENTATION(#31600,#31648);
#31585=SHAPE_DEFINITION_REPRESENTATION(#31601,#31649);
#31586=SHAPE_DEFINITION_REPRESENTATION(#31602,#31650);
#31587=PRODUCT_DEFINITION_SHAPE('',$,#31652);
#31588=PRODUCT_DEFINITION_SHAPE('',$,#31653);
#31589=PRODUCT_DEFINITION_SHAPE('',$,#31654);
#31590=PRODUCT_DEFINITION_SHAPE('',$,#31655);
#31591=PRODUCT_DEFINITION_SHAPE('',$,#31656);
#31592=PRODUCT_DEFINITION_SHAPE('',$,#31657);
#31593=PRODUCT_DEFINITION_SHAPE('',$,#31658);
#31594=PRODUCT_DEFINITION_SHAPE('',$,#31659);
#31595=PRODUCT_DEFINITION_SHAPE('',$,#31660);
#31596=PRODUCT_DEFINITION_SHAPE('',$,#31661);
#31597=PRODUCT_DEFINITION_SHAPE('',$,#31662);
#31598=PRODUCT_DEFINITION_SHAPE('',$,#31663);
#31599=PRODUCT_DEFINITION_SHAPE('',$,#31664);
#31600=PRODUCT_DEFINITION_SHAPE('',$,#31665);
#31601=PRODUCT_DEFINITION_SHAPE('',$,#31666);
#31602=PRODUCT_DEFINITION_SHAPE('',$,#31667);
#31603=PRODUCT_DEFINITION_SHAPE($,$,#107);
#31604=PRODUCT_DEFINITION_SHAPE($,$,#108);
#31605=PRODUCT_DEFINITION_SHAPE($,$,#109);
#31606=PRODUCT_DEFINITION_SHAPE($,$,#110);
#31607=PRODUCT_DEFINITION_SHAPE($,$,#111);
#31608=PRODUCT_DEFINITION_SHAPE($,$,#112);
#31609=PRODUCT_DEFINITION_SHAPE($,$,#113);
#31610=PRODUCT_DEFINITION_SHAPE($,$,#114);
#31611=PRODUCT_DEFINITION_SHAPE($,$,#115);
#31612=PRODUCT_DEFINITION_SHAPE($,$,#116);
#31613=PRODUCT_DEFINITION_SHAPE($,$,#117);
#31614=PRODUCT_DEFINITION_SHAPE($,$,#118);
#31615=PRODUCT_DEFINITION_SHAPE($,$,#119);
#31616=PRODUCT_DEFINITION_SHAPE($,$,#120);
#31617=PRODUCT_DEFINITION_SHAPE($,$,#121);
#31618=PRODUCT_DEFINITION_SHAPE($,$,#122);
#31619=PRODUCT_DEFINITION_SHAPE($,$,#123);
#31620=PRODUCT_DEFINITION_SHAPE($,$,#124);
#31621=PRODUCT_DEFINITION_SHAPE($,$,#125);
#31622=PRODUCT_DEFINITION_SHAPE($,$,#126);
#31623=PRODUCT_DEFINITION_SHAPE($,$,#127);
#31624=PRODUCT_DEFINITION_SHAPE($,$,#128);
#31625=PRODUCT_DEFINITION_SHAPE($,$,#129);
#31626=PRODUCT_DEFINITION_SHAPE($,$,#130);
#31627=PRODUCT_DEFINITION_SHAPE($,$,#131);
#31628=PRODUCT_DEFINITION_SHAPE($,$,#132);
#31629=PRODUCT_DEFINITION_SHAPE($,$,#133);
#31630=PRODUCT_DEFINITION_SHAPE($,$,#134);
#31631=PRODUCT_DEFINITION_SHAPE($,$,#135);
#31632=PRODUCT_DEFINITION_SHAPE($,$,#136);
#31633=PRODUCT_DEFINITION_SHAPE($,$,#137);
#31634=PRODUCT_DEFINITION_SHAPE($,$,#138);
#31635=SHAPE_REPRESENTATION('',(#5896,#6250,#6251,#6252,#6253,#6254,#6255,
#6256,#6257,#6258,#6259,#6260,#6261,#6262,#6263,#6264,#6265,#6266,#6267,
#6268,#6269,#6270,#6271,#6272,#6273,#6274,#6275,#6276,#6277,#6278,#6279,
#6280,#6281),#31550);
#31636=SHAPE_REPRESENTATION('',(#5897),#31551);
#31637=SHAPE_REPRESENTATION('',(#5904),#31552);
#31638=SHAPE_REPRESENTATION('',(#5925),#31553);
#31639=SHAPE_REPRESENTATION('',(#5958),#31554);
#31640=SHAPE_REPRESENTATION('',(#5987),#31555);
#31641=SHAPE_REPRESENTATION('',(#6001),#31556);
#31642=SHAPE_REPRESENTATION('',(#6008),#31557);
#31643=SHAPE_REPRESENTATION('',(#6069),#31558);
#31644=SHAPE_REPRESENTATION('',(#6080),#31559);
#31645=SHAPE_REPRESENTATION('',(#6089),#31560);
#31646=SHAPE_REPRESENTATION('',(#6143),#31561);
#31647=SHAPE_REPRESENTATION('',(#6171),#31562);
#31648=SHAPE_REPRESENTATION('',(#6226),#31563);
#31649=SHAPE_REPRESENTATION('',(#6237),#31564);
#31650=SHAPE_REPRESENTATION('',(#6244),#31565);
#31651=PRODUCT_DEFINITION_CONTEXT('part definition',#31701,'design');
#31652=PRODUCT_DEFINITION('TAS-022','TAS-022',#31668,#31651);
#31653=PRODUCT_DEFINITION('Captured back panel_Right',
'Captured back panel_Right',#31669,#31651);
#31654=PRODUCT_DEFINITION('Door panel','Door panel',#31670,#31651);
#31655=PRODUCT_DEFINITION('Fabricated case hinge leaf',
'Fabricated case hinge leaf',#31671,#31651);
#31656=PRODUCT_DEFINITION('Fabricated door hinge leaf',
'Fabricated door hinge leaf',#31672,#31651);
#31657=PRODUCT_DEFINITION('Retained hinge pin','Retained hinge pin',#31673,
#31651);
#31658=PRODUCT_DEFINITION('Captured back panel_Left',
'Captured back panel_Left',#31674,#31651);
#31659=PRODUCT_DEFINITION('Universal side panel','Universal side panel',
#31675,#31651);
#31660=PRODUCT_DEFINITION('Horizontal closure panel',
'Horizontal closure panel',#31676,#31651);
#31661=PRODUCT_DEFINITION('Fixed shelf','Fixed shelf',#31677,#31651);
#31662=PRODUCT_DEFINITION('Socket head screw M4x24',
'Socket head screw M4x24',#31678,#31651);
#31663=PRODUCT_DEFINITION('Hex nut M4','Hex nut M4',#31679,#31651);
#31664=PRODUCT_DEFINITION('Universal side panel_1',
'Universal side panel_Left',#31680,#31651);
#31665=PRODUCT_DEFINITION('Horizontal closure panel_1',
'Horizontal closure panel_Bottom',#31681,#31651);
#31666=PRODUCT_DEFINITION('Fixed shelf_Middle','Fixed shelf_Middle',#31682,
#31651);
#31667=PRODUCT_DEFINITION('Bay coupling dowel','Bay coupling dowel',#31683,
#31651);
#31668=PRODUCT_DEFINITION_FORMATION('',$,#31703);
#31669=PRODUCT_DEFINITION_FORMATION('',$,#31704);
#31670=PRODUCT_DEFINITION_FORMATION('',$,#31705);
#31671=PRODUCT_DEFINITION_FORMATION('',$,#31706);
#31672=PRODUCT_DEFINITION_FORMATION('',$,#31707);
#31673=PRODUCT_DEFINITION_FORMATION('',$,#31708);
#31674=PRODUCT_DEFINITION_FORMATION('',$,#31709);
#31675=PRODUCT_DEFINITION_FORMATION('',$,#31710);
#31676=PRODUCT_DEFINITION_FORMATION('',$,#31711);
#31677=PRODUCT_DEFINITION_FORMATION('',$,#31712);
#31678=PRODUCT_DEFINITION_FORMATION('',$,#31713);
#31679=PRODUCT_DEFINITION_FORMATION('',$,#31714);
#31680=PRODUCT_DEFINITION_FORMATION('',$,#31715);
#31681=PRODUCT_DEFINITION_FORMATION('',$,#31716);
#31682=PRODUCT_DEFINITION_FORMATION('',$,#31717);
#31683=PRODUCT_DEFINITION_FORMATION('',$,#31718);
#31684=PRODUCT_RELATED_PRODUCT_CATEGORY('TAS-022','TAS-022',(#31703));
#31685=PRODUCT_RELATED_PRODUCT_CATEGORY('Captured back panel_Right',
'Captured back panel_Right',(#31704));
#31686=PRODUCT_RELATED_PRODUCT_CATEGORY('Door panel','Door panel',(#31705));
#31687=PRODUCT_RELATED_PRODUCT_CATEGORY('Fabricated case hinge leaf',
'Fabricated case hinge leaf',(#31706));
#31688=PRODUCT_RELATED_PRODUCT_CATEGORY('Fabricated door hinge leaf',
'Fabricated door hinge leaf',(#31707));
#31689=PRODUCT_RELATED_PRODUCT_CATEGORY('Retained hinge pin',
'Retained hinge pin',(#31708));
#31690=PRODUCT_RELATED_PRODUCT_CATEGORY('Captured back panel_Left',
'Captured back panel_Left',(#31709));
#31691=PRODUCT_RELATED_PRODUCT_CATEGORY('Universal side panel',
'Universal side panel',(#31710));
#31692=PRODUCT_RELATED_PRODUCT_CATEGORY('Horizontal closure panel',
'Horizontal closure panel',(#31711));
#31693=PRODUCT_RELATED_PRODUCT_CATEGORY('Fixed shelf','Fixed shelf',(#31712));
#31694=PRODUCT_RELATED_PRODUCT_CATEGORY('Socket head screw M4x24',
'Socket head screw M4x24',(#31713));
#31695=PRODUCT_RELATED_PRODUCT_CATEGORY('Hex nut M4','Hex nut M4',(#31714));
#31696=PRODUCT_RELATED_PRODUCT_CATEGORY('Universal side panel_Left',
'Universal side panel_Left',(#31715));
#31697=PRODUCT_RELATED_PRODUCT_CATEGORY(
'Horizontal closure panel_Bottom','Horizontal closure panel_Bottom',(#31716));
#31698=PRODUCT_RELATED_PRODUCT_CATEGORY('Fixed shelf_Middle',
'Fixed shelf_Middle',(#31717));
#31699=PRODUCT_RELATED_PRODUCT_CATEGORY('Bay coupling dowel',
'Bay coupling dowel',(#31718));
#31700=APPLICATION_PROTOCOL_DEFINITION('international standard',
'automotive_design',2009,#31701);
#31701=APPLICATION_CONTEXT(
'Core Data for Automotive Mechanical Design Process');
#31702=PRODUCT_CONTEXT('part definition',#31701,'mechanical');
#31703=PRODUCT('TAS-022','TAS-022',$,(#31702));
#31704=PRODUCT('Captured back panel_Right','Captured back panel_Right',
$,(#31702));
#31705=PRODUCT('Door panel','Door panel','Door panel',(#31702));
#31706=PRODUCT('Fabricated case hinge leaf',
'Fabricated case hinge leaf',$,(#31702));
#31707=PRODUCT('Fabricated door hinge leaf',
'Fabricated door hinge leaf',$,(#31702));
#31708=PRODUCT('Retained hinge pin','Retained hinge pin',$,(#31702));
#31709=PRODUCT('Captured back panel_Left','Captured back panel_Left',$,
(#31702));
#31710=PRODUCT('Universal side panel','Universal side panel',$,(#31702));
#31711=PRODUCT('Horizontal closure panel','Horizontal closure panel',$,
(#31702));
#31712=PRODUCT('Fixed shelf','Fixed shelf',$,(#31702));
#31713=PRODUCT('Socket head screw M4x24','Socket head screw M4x24',$,(#31702));
#31714=PRODUCT('Hex nut M4','Hex nut M4',$,(#31702));
#31715=PRODUCT('Universal side panel_1','Universal side panel_Left',$,(#31702));
#31716=PRODUCT('Horizontal closure panel_1',
'Horizontal closure panel_Bottom',$,(#31702));
#31717=PRODUCT('Fixed shelf_Middle','Fixed shelf_Middle',$,(#31702));
#31718=PRODUCT('Bay coupling dowel','Bay coupling dowel',$,(#31702));
#31719=PRESENTATION_STYLE_ASSIGNMENT((#31726));
#31720=PRESENTATION_STYLE_ASSIGNMENT((#31727));
#31721=PRESENTATION_STYLE_ASSIGNMENT((#31728));
#31722=PRESENTATION_STYLE_ASSIGNMENT((#31729));
#31723=PRESENTATION_STYLE_ASSIGNMENT((#31730));
#31724=PRESENTATION_STYLE_ASSIGNMENT((#31731));
#31725=PRESENTATION_STYLE_ASSIGNMENT((#31732));
#31726=SURFACE_STYLE_USAGE(.BOTH.,#31733);
#31727=SURFACE_STYLE_USAGE(.BOTH.,#31734);
#31728=SURFACE_STYLE_USAGE(.BOTH.,#31735);
#31729=SURFACE_STYLE_USAGE(.BOTH.,#31736);
#31730=SURFACE_STYLE_USAGE(.BOTH.,#31737);
#31731=SURFACE_STYLE_USAGE(.BOTH.,#31738);
#31732=SURFACE_STYLE_USAGE(.BOTH.,#31739);
#31733=SURFACE_SIDE_STYLE('',(#31740));
#31734=SURFACE_SIDE_STYLE('',(#31741));
#31735=SURFACE_SIDE_STYLE('',(#31742));
#31736=SURFACE_SIDE_STYLE('',(#31743));
#31737=SURFACE_SIDE_STYLE('',(#31744));
#31738=SURFACE_SIDE_STYLE('',(#31745));
#31739=SURFACE_SIDE_STYLE('',(#31746));
#31740=SURFACE_STYLE_FILL_AREA(#31747);
#31741=SURFACE_STYLE_FILL_AREA(#31748);
#31742=SURFACE_STYLE_FILL_AREA(#31749);
#31743=SURFACE_STYLE_FILL_AREA(#31750);
#31744=SURFACE_STYLE_FILL_AREA(#31751);
#31745=SURFACE_STYLE_FILL_AREA(#31752);
#31746=SURFACE_STYLE_FILL_AREA(#31753);
#31747=FILL_AREA_STYLE('Steel - Satin',(#31754));
#31748=FILL_AREA_STYLE('Opaque(155,165,179)',(#31755));
#31749=FILL_AREA_STYLE('Opaque(70,153,204)',(#31756));
#31750=FILL_AREA_STYLE('Opaque(75,81,92)',(#31757));
#31751=FILL_AREA_STYLE('Opaque(24,59,110)',(#31758));
#31752=FILL_AREA_STYLE('Opaque(169,210,234)',(#31759));
#31753=FILL_AREA_STYLE('Opaque(112,122,133)',(#31760));
#31754=FILL_AREA_STYLE_COLOUR('Steel - Satin',#31761);
#31755=FILL_AREA_STYLE_COLOUR('Opaque(155,165,179)',#31762);
#31756=FILL_AREA_STYLE_COLOUR('Opaque(70,153,204)',#31763);
#31757=FILL_AREA_STYLE_COLOUR('Opaque(75,81,92)',#31764);
#31758=FILL_AREA_STYLE_COLOUR('Opaque(24,59,110)',#31765);
#31759=FILL_AREA_STYLE_COLOUR('Opaque(169,210,234)',#31766);
#31760=FILL_AREA_STYLE_COLOUR('Opaque(112,122,133)',#31767);
#31761=COLOUR_RGB('Steel - Satin',0.627450980392157,0.627450980392157,0.627450980392157);
#31762=COLOUR_RGB('Opaque(155,165,179)',0.607843137254902,0.647058823529412,
0.701960784313725);
#31763=COLOUR_RGB('Opaque(70,153,204)',0.274509803921569,0.6,0.8);
#31764=COLOUR_RGB('Opaque(75,81,92)',0.294117647058824,0.317647058823529,
0.36078431372549);
#31765=COLOUR_RGB('Opaque(24,59,110)',0.0941176470588235,0.231372549019608,
0.431372549019608);
#31766=COLOUR_RGB('Opaque(169,210,234)',0.662745098039216,0.823529411764706,
0.917647058823529);
#31767=COLOUR_RGB('Opaque(112,122,133)',0.43921568627451,0.47843137254902,
0.52156862745098);
ENDSEC;
END-ISO-10303-21;
